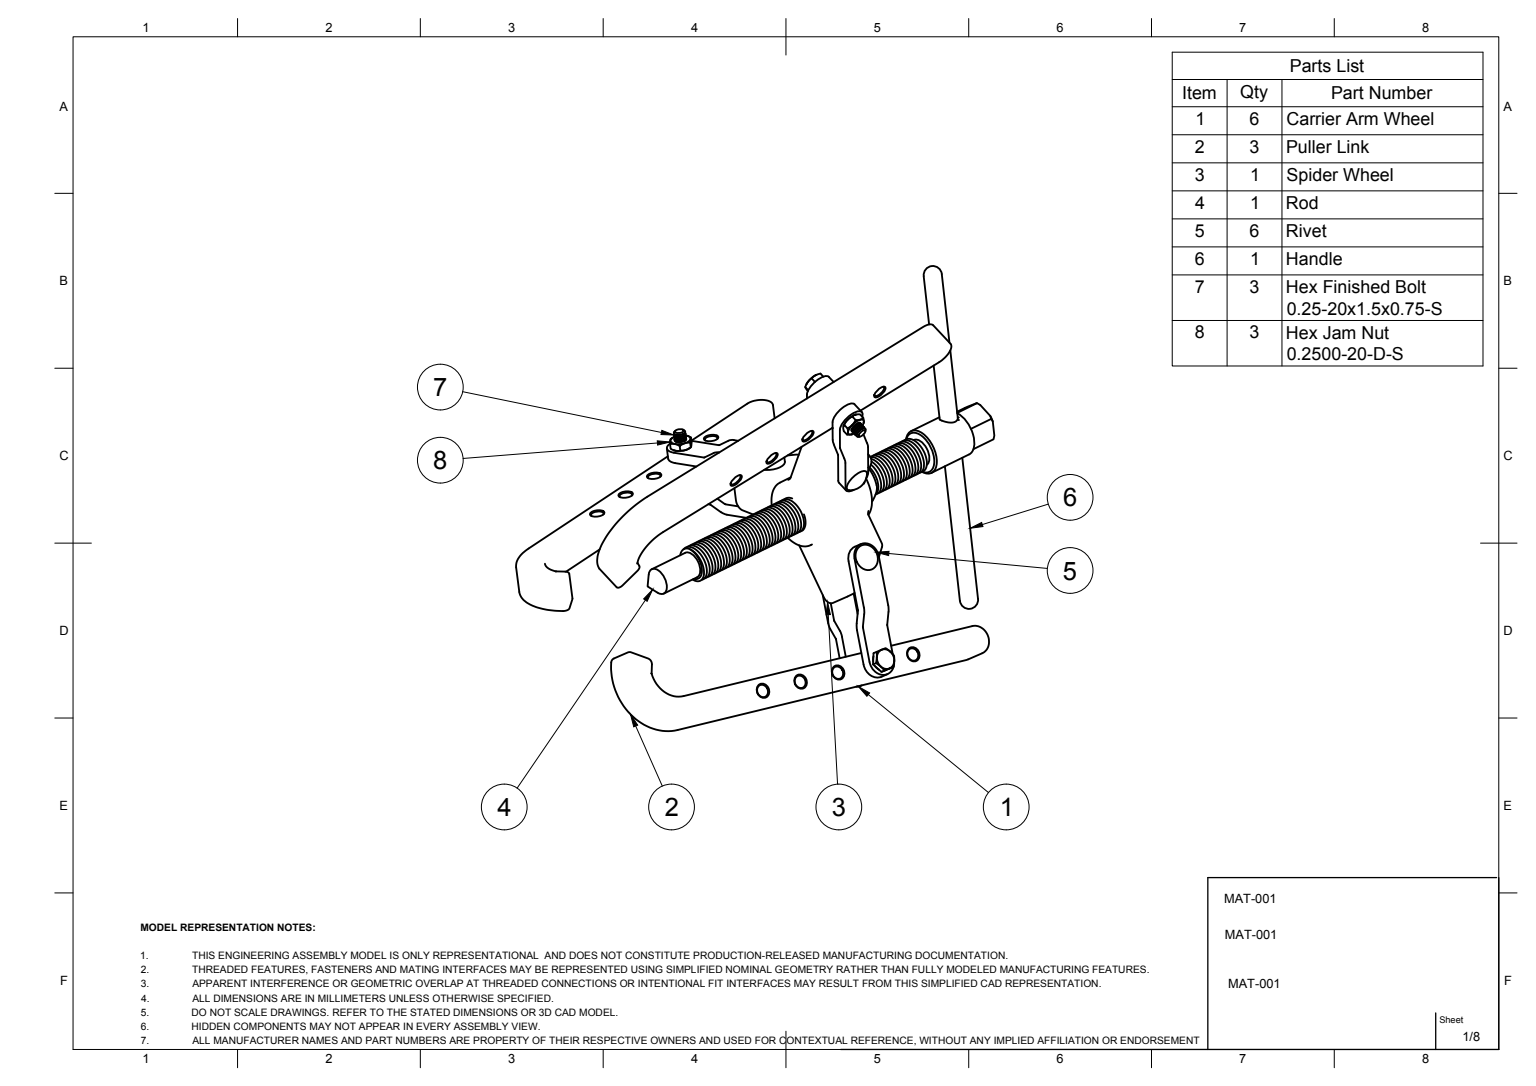
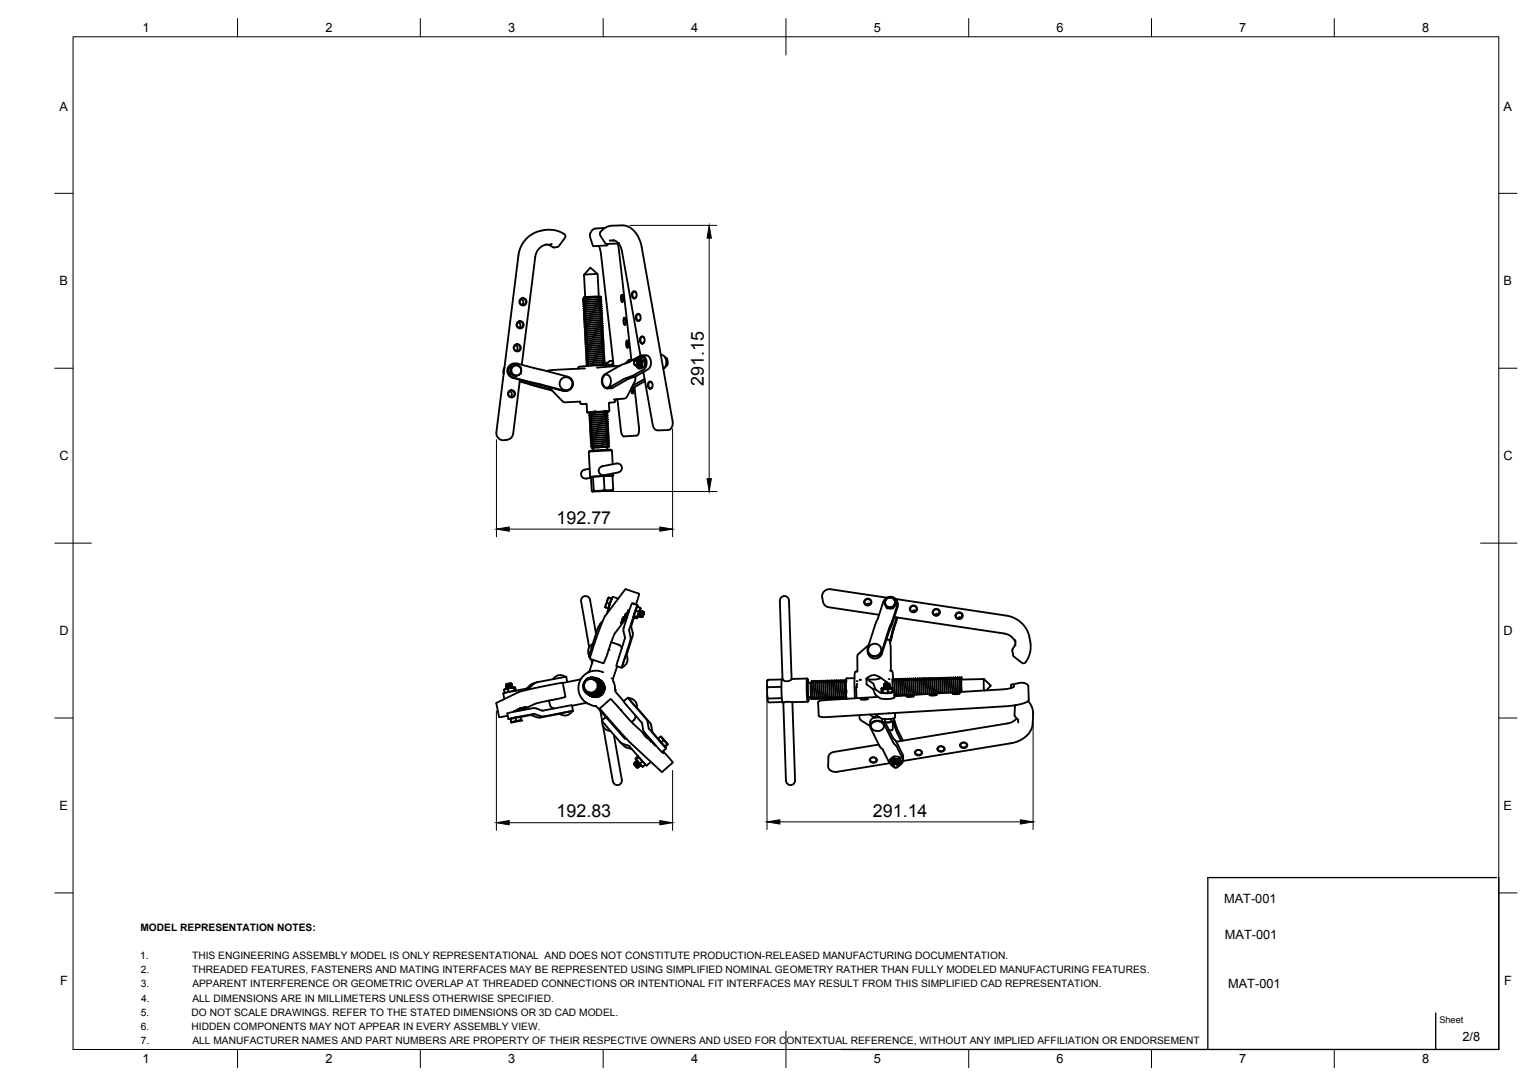
ISO-10303-21;
HEADER;
/* Generated by software containing ST-Developer
 * from STEP Tools, Inc. (www.steptools.com) 
 */

FILE_DESCRIPTION(
/* description */ ('STEP AP214'),
/* implementation_level */ '2;1');

FILE_NAME(
/* name */ 'MAT-001.step',
/* time_stamp */ '2026-11-14T04:30:00-08:00',
/* author */ (''),
/* organization */ (''),
/* preprocessor_version */ 'ST-DEVELOPER v20.2',
/* originating_system */ 'Autodesk Translation Framework v15.17.0.0',
/* authorisation */ '');

FILE_SCHEMA (('AUTOMOTIVE_DESIGN { 1 0 10303 214 3 1 1 }'));
ENDSEC;

DATA;
#10=MECHANICAL_DESIGN_GEOMETRIC_PRESENTATION_REPRESENTATION('',(#123,#124,
#125,#126,#127,#128,#129,#130),#40809);
#11=ITEM_DEFINED_TRANSFORMATION($,$,#7014,#7161);
#12=ITEM_DEFINED_TRANSFORMATION($,$,#7055,#7162);
#13=ITEM_DEFINED_TRANSFORMATION($,$,#6396,#7163);
#14=ITEM_DEFINED_TRANSFORMATION($,$,#6698,#7164);
#15=ITEM_DEFINED_TRANSFORMATION($,$,#6828,#7165);
#16=ITEM_DEFINED_TRANSFORMATION($,$,#6744,#7166);
#17=ITEM_DEFINED_TRANSFORMATION($,$,#6836,#7167);
#18=ITEM_DEFINED_TRANSFORMATION($,$,#6754,#7168);
#19=ITEM_DEFINED_TRANSFORMATION($,$,#7014,#7169);
#20=ITEM_DEFINED_TRANSFORMATION($,$,#6828,#7170);
#21=ITEM_DEFINED_TRANSFORMATION($,$,#7014,#7171);
#22=ITEM_DEFINED_TRANSFORMATION($,$,#7014,#7172);
#23=ITEM_DEFINED_TRANSFORMATION($,$,#6828,#7173);
#24=ITEM_DEFINED_TRANSFORMATION($,$,#6828,#7174);
#25=ITEM_DEFINED_TRANSFORMATION($,$,#6754,#7175);
#26=ITEM_DEFINED_TRANSFORMATION($,$,#6754,#7176);
#27=ITEM_DEFINED_TRANSFORMATION($,$,#6828,#7177);
#28=ITEM_DEFINED_TRANSFORMATION($,$,#6828,#7178);
#29=ITEM_DEFINED_TRANSFORMATION($,$,#6836,#7179);
#30=ITEM_DEFINED_TRANSFORMATION($,$,#6836,#7180);
#31=ITEM_DEFINED_TRANSFORMATION($,$,#7014,#7181);
#32=ITEM_DEFINED_TRANSFORMATION($,$,#7014,#7182);
#33=ITEM_DEFINED_TRANSFORMATION($,$,#7055,#7183);
#34=ITEM_DEFINED_TRANSFORMATION($,$,#7055,#7184);
#35=(
REPRESENTATION_RELATIONSHIP($,$,#40863,#40856)
REPRESENTATION_RELATIONSHIP_WITH_TRANSFORMATION(#11)
SHAPE_REPRESENTATION_RELATIONSHIP()
);
#36=(
REPRESENTATION_RELATIONSHIP($,$,#40864,#40856)
REPRESENTATION_RELATIONSHIP_WITH_TRANSFORMATION(#12)
SHAPE_REPRESENTATION_RELATIONSHIP()
);
#37=(
REPRESENTATION_RELATIONSHIP($,$,#40857,#40856)
REPRESENTATION_RELATIONSHIP_WITH_TRANSFORMATION(#13)
SHAPE_REPRESENTATION_RELATIONSHIP()
);
#38=(
REPRESENTATION_RELATIONSHIP($,$,#40858,#40856)
REPRESENTATION_RELATIONSHIP_WITH_TRANSFORMATION(#14)
SHAPE_REPRESENTATION_RELATIONSHIP()
);
#39=(
REPRESENTATION_RELATIONSHIP($,$,#40861,#40856)
REPRESENTATION_RELATIONSHIP_WITH_TRANSFORMATION(#15)
SHAPE_REPRESENTATION_RELATIONSHIP()
);
#40=(
REPRESENTATION_RELATIONSHIP($,$,#40859,#40856)
REPRESENTATION_RELATIONSHIP_WITH_TRANSFORMATION(#16)
SHAPE_REPRESENTATION_RELATIONSHIP()
);
#41=(
REPRESENTATION_RELATIONSHIP($,$,#40862,#40856)
REPRESENTATION_RELATIONSHIP_WITH_TRANSFORMATION(#17)
SHAPE_REPRESENTATION_RELATIONSHIP()
);
#42=(
REPRESENTATION_RELATIONSHIP($,$,#40860,#40856)
REPRESENTATION_RELATIONSHIP_WITH_TRANSFORMATION(#18)
SHAPE_REPRESENTATION_RELATIONSHIP()
);
#43=(
REPRESENTATION_RELATIONSHIP($,$,#40863,#40856)
REPRESENTATION_RELATIONSHIP_WITH_TRANSFORMATION(#19)
SHAPE_REPRESENTATION_RELATIONSHIP()
);
#44=(
REPRESENTATION_RELATIONSHIP($,$,#40861,#40856)
REPRESENTATION_RELATIONSHIP_WITH_TRANSFORMATION(#20)
SHAPE_REPRESENTATION_RELATIONSHIP()
);
#45=(
REPRESENTATION_RELATIONSHIP($,$,#40863,#40856)
REPRESENTATION_RELATIONSHIP_WITH_TRANSFORMATION(#21)
SHAPE_REPRESENTATION_RELATIONSHIP()
);
#46=(
REPRESENTATION_RELATIONSHIP($,$,#40863,#40856)
REPRESENTATION_RELATIONSHIP_WITH_TRANSFORMATION(#22)
SHAPE_REPRESENTATION_RELATIONSHIP()
);
#47=(
REPRESENTATION_RELATIONSHIP($,$,#40861,#40856)
REPRESENTATION_RELATIONSHIP_WITH_TRANSFORMATION(#23)
SHAPE_REPRESENTATION_RELATIONSHIP()
);
#48=(
REPRESENTATION_RELATIONSHIP($,$,#40861,#40856)
REPRESENTATION_RELATIONSHIP_WITH_TRANSFORMATION(#24)
SHAPE_REPRESENTATION_RELATIONSHIP()
);
#49=(
REPRESENTATION_RELATIONSHIP($,$,#40860,#40856)
REPRESENTATION_RELATIONSHIP_WITH_TRANSFORMATION(#25)
SHAPE_REPRESENTATION_RELATIONSHIP()
);
#50=(
REPRESENTATION_RELATIONSHIP($,$,#40860,#40856)
REPRESENTATION_RELATIONSHIP_WITH_TRANSFORMATION(#26)
SHAPE_REPRESENTATION_RELATIONSHIP()
);
#51=(
REPRESENTATION_RELATIONSHIP($,$,#40861,#40856)
REPRESENTATION_RELATIONSHIP_WITH_TRANSFORMATION(#27)
SHAPE_REPRESENTATION_RELATIONSHIP()
);
#52=(
REPRESENTATION_RELATIONSHIP($,$,#40861,#40856)
REPRESENTATION_RELATIONSHIP_WITH_TRANSFORMATION(#28)
SHAPE_REPRESENTATION_RELATIONSHIP()
);
#53=(
REPRESENTATION_RELATIONSHIP($,$,#40862,#40856)
REPRESENTATION_RELATIONSHIP_WITH_TRANSFORMATION(#29)
SHAPE_REPRESENTATION_RELATIONSHIP()
);
#54=(
REPRESENTATION_RELATIONSHIP($,$,#40862,#40856)
REPRESENTATION_RELATIONSHIP_WITH_TRANSFORMATION(#30)
SHAPE_REPRESENTATION_RELATIONSHIP()
);
#55=(
REPRESENTATION_RELATIONSHIP($,$,#40863,#40856)
REPRESENTATION_RELATIONSHIP_WITH_TRANSFORMATION(#31)
SHAPE_REPRESENTATION_RELATIONSHIP()
);
#56=(
REPRESENTATION_RELATIONSHIP($,$,#40863,#40856)
REPRESENTATION_RELATIONSHIP_WITH_TRANSFORMATION(#32)
SHAPE_REPRESENTATION_RELATIONSHIP()
);
#57=(
REPRESENTATION_RELATIONSHIP($,$,#40864,#40856)
REPRESENTATION_RELATIONSHIP_WITH_TRANSFORMATION(#33)
SHAPE_REPRESENTATION_RELATIONSHIP()
);
#58=(
REPRESENTATION_RELATIONSHIP($,$,#40864,#40856)
REPRESENTATION_RELATIONSHIP_WITH_TRANSFORMATION(#34)
SHAPE_REPRESENTATION_RELATIONSHIP()
);
#59=CONTEXT_DEPENDENT_SHAPE_REPRESENTATION(#35,#40832);
#60=CONTEXT_DEPENDENT_SHAPE_REPRESENTATION(#36,#40833);
#61=CONTEXT_DEPENDENT_SHAPE_REPRESENTATION(#37,#40834);
#62=CONTEXT_DEPENDENT_SHAPE_REPRESENTATION(#38,#40835);
#63=CONTEXT_DEPENDENT_SHAPE_REPRESENTATION(#39,#40836);
#64=CONTEXT_DEPENDENT_SHAPE_REPRESENTATION(#40,#40837);
#65=CONTEXT_DEPENDENT_SHAPE_REPRESENTATION(#41,#40838);
#66=CONTEXT_DEPENDENT_SHAPE_REPRESENTATION(#42,#40839);
#67=CONTEXT_DEPENDENT_SHAPE_REPRESENTATION(#43,#40840);
#68=CONTEXT_DEPENDENT_SHAPE_REPRESENTATION(#44,#40841);
#69=CONTEXT_DEPENDENT_SHAPE_REPRESENTATION(#45,#40842);
#70=CONTEXT_DEPENDENT_SHAPE_REPRESENTATION(#46,#40843);
#71=CONTEXT_DEPENDENT_SHAPE_REPRESENTATION(#47,#40844);
#72=CONTEXT_DEPENDENT_SHAPE_REPRESENTATION(#48,#40845);
#73=CONTEXT_DEPENDENT_SHAPE_REPRESENTATION(#49,#40846);
#74=CONTEXT_DEPENDENT_SHAPE_REPRESENTATION(#50,#40847);
#75=CONTEXT_DEPENDENT_SHAPE_REPRESENTATION(#51,#40848);
#76=CONTEXT_DEPENDENT_SHAPE_REPRESENTATION(#52,#40849);
#77=CONTEXT_DEPENDENT_SHAPE_REPRESENTATION(#53,#40850);
#78=CONTEXT_DEPENDENT_SHAPE_REPRESENTATION(#54,#40851);
#79=CONTEXT_DEPENDENT_SHAPE_REPRESENTATION(#55,#40852);
#80=CONTEXT_DEPENDENT_SHAPE_REPRESENTATION(#56,#40853);
#81=CONTEXT_DEPENDENT_SHAPE_REPRESENTATION(#57,#40854);
#82=CONTEXT_DEPENDENT_SHAPE_REPRESENTATION(#58,#40855);
#83=NEXT_ASSEMBLY_USAGE_OCCURRENCE('Carrier Arm Wheel:1',
'Carrier Arm Wheel:1','Carrier Arm Wheel:1',#40866,#40873,
'Carrier Arm Wheel:1');
#84=NEXT_ASSEMBLY_USAGE_OCCURRENCE('Puller Link:1','Puller Link:1',
'Puller Link:1',#40866,#40874,'Puller Link:1');
#85=NEXT_ASSEMBLY_USAGE_OCCURRENCE('Spider Wheel:1','Spider Wheel:1',
'Spider Wheel:1',#40866,#40867,'Spider Wheel:1');
#86=NEXT_ASSEMBLY_USAGE_OCCURRENCE('Rod:1','Rod:1','Rod:1',#40866,#40868,
'Rod:1');
#87=NEXT_ASSEMBLY_USAGE_OCCURRENCE('Rivet:1','Rivet:1','Rivet:1',#40866,
#40871,'Rivet:1');
#88=NEXT_ASSEMBLY_USAGE_OCCURRENCE('Handle:1','Handle:1','Handle:1',#40866,
#40869,'Handle:1');
#89=NEXT_ASSEMBLY_USAGE_OCCURRENCE(
'Hex Finished Bolt 0.25-20x1.5x0.75-S:1',
'Hex Finished Bolt 0.25-20x1.5x0.75-S:1',
'Hex Finished Bolt 0.25-20x1.5x0.75-S:1',#40866,#40872,
'Hex Finished Bolt 0.25-20x1.5x0.75-S:1');
#90=NEXT_ASSEMBLY_USAGE_OCCURRENCE('Hex Jam Nut 0.2500-20-D-S:1',
'Hex Jam Nut 0.2500-20-D-S:1','Hex Jam Nut 0.2500-20-D-S:1',#40866,#40870,
'Hex Jam Nut 0.2500-20-D-S:1');
#91=NEXT_ASSEMBLY_USAGE_OCCURRENCE('Carrier Arm Wheel:2',
'Carrier Arm Wheel:2','Carrier Arm Wheel:2',#40866,#40873,
'Carrier Arm Wheel:2');
#92=NEXT_ASSEMBLY_USAGE_OCCURRENCE('Rivet:2','Rivet:2','Rivet:2',#40866,
#40871,'Rivet:2');
#93=NEXT_ASSEMBLY_USAGE_OCCURRENCE('Carrier Arm Wheel:3',
'Carrier Arm Wheel:3','Carrier Arm Wheel:3',#40866,#40873,
'Carrier Arm Wheel:3');
#94=NEXT_ASSEMBLY_USAGE_OCCURRENCE('Carrier Arm Wheel:4',
'Carrier Arm Wheel:4','Carrier Arm Wheel:4',#40866,#40873,
'Carrier Arm Wheel:4');
#95=NEXT_ASSEMBLY_USAGE_OCCURRENCE('Rivet:3','Rivet:3','Rivet:3',#40866,
#40871,'Rivet:3');
#96=NEXT_ASSEMBLY_USAGE_OCCURRENCE('Rivet:4','Rivet:4','Rivet:4',#40866,
#40871,'Rivet:4');
#97=NEXT_ASSEMBLY_USAGE_OCCURRENCE('Hex Jam Nut 0.2500-20-D-S:2',
'Hex Jam Nut 0.2500-20-D-S:2','Hex Jam Nut 0.2500-20-D-S:2',#40866,#40870,
'Hex Jam Nut 0.2500-20-D-S:2');
#98=NEXT_ASSEMBLY_USAGE_OCCURRENCE('Hex Jam Nut 0.2500-20-D-S:3',
'Hex Jam Nut 0.2500-20-D-S:3','Hex Jam Nut 0.2500-20-D-S:3',#40866,#40870,
'Hex Jam Nut 0.2500-20-D-S:3');
#99=NEXT_ASSEMBLY_USAGE_OCCURRENCE('Rivet:5','Rivet:5','Rivet:5',#40866,
#40871,'Rivet:5');
#100=NEXT_ASSEMBLY_USAGE_OCCURRENCE('Rivet:6','Rivet:6','Rivet:6',#40866,
#40871,'Rivet:6');
#101=NEXT_ASSEMBLY_USAGE_OCCURRENCE(
'Hex Finished Bolt 0.25-20x1.5x0.75-S:2',
'Hex Finished Bolt 0.25-20x1.5x0.75-S:2',
'Hex Finished Bolt 0.25-20x1.5x0.75-S:2',#40866,#40872,
'Hex Finished Bolt 0.25-20x1.5x0.75-S:2');
#102=NEXT_ASSEMBLY_USAGE_OCCURRENCE(
'Hex Finished Bolt 0.25-20x1.5x0.75-S:3',
'Hex Finished Bolt 0.25-20x1.5x0.75-S:3',
'Hex Finished Bolt 0.25-20x1.5x0.75-S:3',#40866,#40872,
'Hex Finished Bolt 0.25-20x1.5x0.75-S:3');
#103=NEXT_ASSEMBLY_USAGE_OCCURRENCE('Carrier Arm Wheel:5',
'Carrier Arm Wheel:5','Carrier Arm Wheel:5',#40866,#40873,
'Carrier Arm Wheel:5');
#104=NEXT_ASSEMBLY_USAGE_OCCURRENCE('Carrier Arm Wheel:6',
'Carrier Arm Wheel:6','Carrier Arm Wheel:6',#40866,#40873,
'Carrier Arm Wheel:6');
#105=NEXT_ASSEMBLY_USAGE_OCCURRENCE('Puller Link:2','Puller Link:2',
'Puller Link:2',#40866,#40874,'Puller Link:2');
#106=NEXT_ASSEMBLY_USAGE_OCCURRENCE('Puller Link:3','Puller Link:3',
'Puller Link:3',#40866,#40874,'Puller Link:3');
#107=SHAPE_REPRESENTATION_RELATIONSHIP('SRR','None',#40857,#115);
#108=SHAPE_REPRESENTATION_RELATIONSHIP('SRR','None',#40858,#116);
#109=SHAPE_REPRESENTATION_RELATIONSHIP('SRR','None',#40859,#117);
#110=SHAPE_REPRESENTATION_RELATIONSHIP('SRR','None',#40860,#118);
#111=SHAPE_REPRESENTATION_RELATIONSHIP('SRR','None',#40861,#119);
#112=SHAPE_REPRESENTATION_RELATIONSHIP('SRR','None',#40862,#120);
#113=SHAPE_REPRESENTATION_RELATIONSHIP('SRR','None',#40863,#121);
#114=SHAPE_REPRESENTATION_RELATIONSHIP('SRR','None',#40864,#122);
#115=ADVANCED_BREP_SHAPE_REPRESENTATION('',(#131),#40801);
#116=ADVANCED_BREP_SHAPE_REPRESENTATION('',(#132),#40802);
#117=ADVANCED_BREP_SHAPE_REPRESENTATION('',(#133),#40803);
#118=ADVANCED_BREP_SHAPE_REPRESENTATION('',(#134),#40804);
#119=ADVANCED_BREP_SHAPE_REPRESENTATION('',(#135),#40805);
#120=ADVANCED_BREP_SHAPE_REPRESENTATION('',(#136),#40806);
#121=ADVANCED_BREP_SHAPE_REPRESENTATION('',(#137),#40807);
#122=ADVANCED_BREP_SHAPE_REPRESENTATION('',(#138),#40808);
#123=STYLED_ITEM('',(#40906),#131);
#124=STYLED_ITEM('',(#40907),#132);
#125=STYLED_ITEM('',(#40908),#133);
#126=STYLED_ITEM('',(#40909),#134);
#127=STYLED_ITEM('',(#40908),#135);
#128=STYLED_ITEM('',(#40909),#136);
#129=STYLED_ITEM('',(#40906),#137);
#130=STYLED_ITEM('',(#40906),#138);
#131=MANIFOLD_SOLID_BREP('Body1',#6298);
#132=MANIFOLD_SOLID_BREP('Body1',#6299);
#133=MANIFOLD_SOLID_BREP('Body1',#6300);
#134=MANIFOLD_SOLID_BREP('Body1',#6301);
#135=MANIFOLD_SOLID_BREP('Body1',#6302);
#136=MANIFOLD_SOLID_BREP('Body1',#6303);
#137=MANIFOLD_SOLID_BREP('Body1',#6304);
#138=MANIFOLD_SOLID_BREP('Body1',#6305);
#139=SPHERICAL_SURFACE('',#6615,5.);
#140=SPHERICAL_SURFACE('',#6624,5.);
#141=SPHERICAL_SURFACE('',#6633,5.);
#142=SPHERICAL_SURFACE('',#6642,5.);
#143=SPHERICAL_SURFACE('',#6643,5.);
#144=SPHERICAL_SURFACE('',#6652,5.);
#145=SPHERICAL_SURFACE('',#6745,4.975);
#146=SPHERICAL_SURFACE('',#6749,4.975);
#147=SPHERICAL_SURFACE('',#6832,9.31007692307692);
#148=(
BOUNDED_SURFACE()
B_SPLINE_SURFACE(1,2,((#13053,#13054,#13055,#13056,#13057,#13058,#13059,
#13060,#13061,#13062,#13063,#13064,#13065,#13066,#13067,#13068,#13069,#13070,
#13071,#13072,#13073,#13074,#13075,#13076,#13077,#13078,#13079,#13080,#13081,
#13082,#13083,#13084,#13085,#13086,#13087,#13088,#13089,#13090,#13091,#13092,
#13093,#13094,#13095,#13096,#13097,#13098,#13099,#13100,#13101,#13102,#13103,
#13104,#13105,#13106,#13107,#13108,#13109,#13110,#13111,#13112,#13113,#13114,
#13115,#13116,#13117,#13118,#13119,#13120,#13121,#13122,#13123,#13124,#13125,
#13126,#13127,#13128,#13129,#13130,#13131,#13132,#13133,#13134,#13135,#13136,
#13137,#13138,#13139,#13140,#13141,#13142,#13143,#13144,#13145,#13146,#13147,
#13148,#13149,#13150,#13151,#13152,#13153,#13154,#13155,#13156,#13157,#13158,
#13159,#13160,#13161,#13162,#13163,#13164,#13165,#13166,#13167,#13168,#13169,
#13170,#13171,#13172,#13173,#13174,#13175,#13176,#13177,#13178,#13179,#13180,
#13181,#13182,#13183,#13184,#13185,#13186,#13187,#13188,#13189,#13190,#13191,
#13192,#13193,#13194,#13195,#13196,#13197,#13198,#13199,#13200,#13201,#13202,
#13203,#13204,#13205,#13206,#13207,#13208,#13209,#13210,#13211,#13212,#13213,
#13214,#13215,#13216,#13217,#13218,#13219,#13220,#13221,#13222,#13223,#13224,
#13225,#13226,#13227,#13228,#13229,#13230,#13231,#13232,#13233,#13234,#13235,
#13236,#13237,#13238,#13239,#13240,#13241,#13242,#13243,#13244,#13245,#13246,
#13247,#13248,#13249,#13250,#13251,#13252,#13253,#13254,#13255,#13256,#13257,
#13258,#13259,#13260,#13261,#13262,#13263,#13264,#13265,#13266,#13267,#13268,
#13269,#13270,#13271,#13272,#13273,#13274,#13275,#13276,#13277,#13278,#13279,
#13280,#13281,#13282,#13283,#13284,#13285,#13286,#13287,#13288,#13289,#13290,
#13291,#13292,#13293,#13294,#13295,#13296,#13297,#13298,#13299,#13300,#13301,
#13302,#13303,#13304,#13305,#13306,#13307,#13308,#13309,#13310,#13311,#13312,
#13313,#13314,#13315,#13316,#13317,#13318,#13319,#13320,#13321,#13322,#13323,
#13324,#13325,#13326,#13327,#13328,#13329,#13330,#13331,#13332,#13333,#13334,
#13335,#13336,#13337,#13338,#13339,#13340,#13341,#13342,#13343,#13344,#13345,
#13346,#13347,#13348,#13349,#13350,#13351,#13352,#13353,#13354,#13355,#13356,
#13357,#13358,#13359,#13360,#13361,#13362,#13363,#13364,#13365,#13366,#13367,
#13368,#13369,#13370,#13371,#13372,#13373,#13374,#13375,#13376,#13377,#13378,
#13379,#13380,#13381,#13382,#13383,#13384,#13385,#13386,#13387,#13388,#13389,
#13390,#13391,#13392,#13393,#13394,#13395,#13396,#13397,#13398,#13399,#13400,
#13401,#13402,#13403,#13404,#13405,#13406,#13407,#13408,#13409,#13410,#13411,
#13412,#13413,#13414,#13415,#13416,#13417,#13418,#13419,#13420,#13421,#13422,
#13423,#13424,#13425,#13426,#13427,#13428,#13429,#13430,#13431,#13432,#13433,
#13434,#13435,#13436,#13437,#13438,#13439,#13440,#13441,#13442,#13443,#13444,
#13445,#13446,#13447,#13448,#13449,#13450,#13451,#13452,#13453,#13454,#13455,
#13456,#13457,#13458,#13459,#13460,#13461,#13462,#13463,#13464,#13465,#13466,
#13467,#13468,#13469,#13470,#13471,#13472,#13473,#13474,#13475,#13476,#13477,
#13478,#13479,#13480,#13481,#13482,#13483,#13484,#13485,#13486,#13487,#13488,
#13489,#13490,#13491,#13492,#13493,#13494,#13495,#13496,#13497,#13498,#13499,
#13500,#13501,#13502,#13503,#13504,#13505,#13506,#13507,#13508,#13509,#13510,
#13511,#13512,#13513,#13514,#13515,#13516,#13517,#13518,#13519,#13520,#13521,
#13522,#13523,#13524,#13525,#13526,#13527,#13528,#13529,#13530,#13531,#13532,
#13533,#13534,#13535,#13536,#13537,#13538,#13539,#13540,#13541,#13542,#13543,
#13544,#13545,#13546,#13547,#13548,#13549,#13550,#13551,#13552,#13553,#13554,
#13555,#13556,#13557,#13558,#13559,#13560,#13561,#13562,#13563,#13564,#13565,
#13566,#13567,#13568,#13569,#13570,#13571,#13572,#13573,#13574,#13575,#13576,
#13577,#13578,#13579,#13580,#13581,#13582,#13583,#13584,#13585,#13586,#13587,
#13588,#13589,#13590,#13591,#13592,#13593,#13594,#13595,#13596,#13597,#13598,
#13599,#13600,#13601,#13602,#13603,#13604,#13605,#13606,#13607,#13608,#13609,
#13610,#13611,#13612,#13613,#13614,#13615,#13616,#13617,#13618,#13619,#13620,
#13621,#13622,#13623,#13624,#13625,#13626,#13627,#13628,#13629,#13630,#13631,
#13632,#13633,#13634,#13635,#13636,#13637,#13638,#13639,#13640,#13641,#13642,
#13643,#13644,#13645,#13646,#13647,#13648,#13649,#13650,#13651,#13652,#13653,
#13654,#13655,#13656,#13657,#13658,#13659,#13660,#13661,#13662,#13663,#13664,
#13665,#13666,#13667,#13668,#13669,#13670,#13671,#13672,#13673,#13674,#13675,
#13676,#13677,#13678,#13679,#13680,#13681,#13682,#13683,#13684,#13685,#13686,
#13687,#13688,#13689,#13690,#13691,#13692,#13693,#13694,#13695,#13696,#13697,
#13698,#13699,#13700,#13701,#13702,#13703,#13704,#13705,#13706,#13707,#13708,
#13709,#13710,#13711,#13712,#13713,#13714,#13715,#13716,#13717,#13718,#13719,
#13720,#13721,#13722,#13723,#13724,#13725,#13726,#13727,#13728,#13729,#13730,
#13731,#13732,#13733,#13734,#13735,#13736,#13737,#13738,#13739,#13740,#13741,
#13742,#13743,#13744,#13745,#13746,#13747,#13748,#13749,#13750,#13751,#13752,
#13753,#13754,#13755,#13756,#13757,#13758,#13759,#13760,#13761,#13762,#13763,
#13764,#13765,#13766,#13767,#13768,#13769,#13770,#13771,#13772,#13773,#13774,
#13775,#13776,#13777,#13778,#13779,#13780,#13781,#13782,#13783,#13784,#13785,
#13786,#13787,#13788,#13789,#13790,#13791,#13792,#13793,#13794,#13795,#13796,
#13797,#13798,#13799,#13800,#13801,#13802,#13803,#13804,#13805,#13806,#13807,
#13808,#13809,#13810,#13811,#13812,#13813,#13814,#13815,#13816,#13817,#13818,
#13819,#13820,#13821,#13822,#13823,#13824,#13825,#13826,#13827,#13828,#13829,
#13830,#13831,#13832,#13833,#13834,#13835,#13836,#13837,#13838,#13839,#13840,
#13841,#13842,#13843,#13844,#13845,#13846,#13847,#13848,#13849,#13850,#13851,
#13852,#13853,#13854,#13855,#13856,#13857,#13858,#13859,#13860,#13861,#13862,
#13863,#13864,#13865,#13866,#13867,#13868,#13869,#13870,#13871,#13872,#13873,
#13874,#13875,#13876,#13877,#13878,#13879,#13880,#13881,#13882,#13883,#13884,
#13885,#13886,#13887,#13888,#13889,#13890,#13891,#13892,#13893,#13894,#13895,
#13896,#13897,#13898,#13899,#13900,#13901,#13902,#13903,#13904,#13905,#13906,
#13907,#13908,#13909,#13910,#13911,#13912,#13913,#13914,#13915,#13916,#13917,
#13918,#13919,#13920,#13921,#13922,#13923,#13924,#13925,#13926,#13927,#13928,
#13929,#13930,#13931,#13932,#13933,#13934,#13935,#13936,#13937,#13938,#13939,
#13940,#13941,#13942,#13943,#13944,#13945,#13946,#13947,#13948,#13949,#13950,
#13951,#13952,#13953,#13954,#13955,#13956,#13957,#13958,#13959,#13960,#13961,
#13962,#13963,#13964,#13965,#13966,#13967,#13968,#13969,#13970,#13971,#13972,
#13973,#13974,#13975,#13976,#13977,#13978,#13979,#13980,#13981,#13982,#13983,
#13984,#13985,#13986,#13987,#13988,#13989,#13990,#13991,#13992,#13993,#13994,
#13995,#13996,#13997,#13998,#13999,#14000,#14001,#14002,#14003,#14004,#14005,
#14006,#14007,#14008,#14009,#14010,#14011,#14012,#14013,#14014,#14015,#14016,
#14017,#14018,#14019,#14020,#14021,#14022,#14023,#14024,#14025),(#14026,
#14027,#14028,#14029,#14030,#14031,#14032,#14033,#14034,#14035,#14036,#14037,
#14038,#14039,#14040,#14041,#14042,#14043,#14044,#14045,#14046,#14047,#14048,
#14049,#14050,#14051,#14052,#14053,#14054,#14055,#14056,#14057,#14058,#14059,
#14060,#14061,#14062,#14063,#14064,#14065,#14066,#14067,#14068,#14069,#14070,
#14071,#14072,#14073,#14074,#14075,#14076,#14077,#14078,#14079,#14080,#14081,
#14082,#14083,#14084,#14085,#14086,#14087,#14088,#14089,#14090,#14091,#14092,
#14093,#14094,#14095,#14096,#14097,#14098,#14099,#14100,#14101,#14102,#14103,
#14104,#14105,#14106,#14107,#14108,#14109,#14110,#14111,#14112,#14113,#14114,
#14115,#14116,#14117,#14118,#14119,#14120,#14121,#14122,#14123,#14124,#14125,
#14126,#14127,#14128,#14129,#14130,#14131,#14132,#14133,#14134,#14135,#14136,
#14137,#14138,#14139,#14140,#14141,#14142,#14143,#14144,#14145,#14146,#14147,
#14148,#14149,#14150,#14151,#14152,#14153,#14154,#14155,#14156,#14157,#14158,
#14159,#14160,#14161,#14162,#14163,#14164,#14165,#14166,#14167,#14168,#14169,
#14170,#14171,#14172,#14173,#14174,#14175,#14176,#14177,#14178,#14179,#14180,
#14181,#14182,#14183,#14184,#14185,#14186,#14187,#14188,#14189,#14190,#14191,
#14192,#14193,#14194,#14195,#14196,#14197,#14198,#14199,#14200,#14201,#14202,
#14203,#14204,#14205,#14206,#14207,#14208,#14209,#14210,#14211,#14212,#14213,
#14214,#14215,#14216,#14217,#14218,#14219,#14220,#14221,#14222,#14223,#14224,
#14225,#14226,#14227,#14228,#14229,#14230,#14231,#14232,#14233,#14234,#14235,
#14236,#14237,#14238,#14239,#14240,#14241,#14242,#14243,#14244,#14245,#14246,
#14247,#14248,#14249,#14250,#14251,#14252,#14253,#14254,#14255,#14256,#14257,
#14258,#14259,#14260,#14261,#14262,#14263,#14264,#14265,#14266,#14267,#14268,
#14269,#14270,#14271,#14272,#14273,#14274,#14275,#14276,#14277,#14278,#14279,
#14280,#14281,#14282,#14283,#14284,#14285,#14286,#14287,#14288,#14289,#14290,
#14291,#14292,#14293,#14294,#14295,#14296,#14297,#14298,#14299,#14300,#14301,
#14302,#14303,#14304,#14305,#14306,#14307,#14308,#14309,#14310,#14311,#14312,
#14313,#14314,#14315,#14316,#14317,#14318,#14319,#14320,#14321,#14322,#14323,
#14324,#14325,#14326,#14327,#14328,#14329,#14330,#14331,#14332,#14333,#14334,
#14335,#14336,#14337,#14338,#14339,#14340,#14341,#14342,#14343,#14344,#14345,
#14346,#14347,#14348,#14349,#14350,#14351,#14352,#14353,#14354,#14355,#14356,
#14357,#14358,#14359,#14360,#14361,#14362,#14363,#14364,#14365,#14366,#14367,
#14368,#14369,#14370,#14371,#14372,#14373,#14374,#14375,#14376,#14377,#14378,
#14379,#14380,#14381,#14382,#14383,#14384,#14385,#14386,#14387,#14388,#14389,
#14390,#14391,#14392,#14393,#14394,#14395,#14396,#14397,#14398,#14399,#14400,
#14401,#14402,#14403,#14404,#14405,#14406,#14407,#14408,#14409,#14410,#14411,
#14412,#14413,#14414,#14415,#14416,#14417,#14418,#14419,#14420,#14421,#14422,
#14423,#14424,#14425,#14426,#14427,#14428,#14429,#14430,#14431,#14432,#14433,
#14434,#14435,#14436,#14437,#14438,#14439,#14440,#14441,#14442,#14443,#14444,
#14445,#14446,#14447,#14448,#14449,#14450,#14451,#14452,#14453,#14454,#14455,
#14456,#14457,#14458,#14459,#14460,#14461,#14462,#14463,#14464,#14465,#14466,
#14467,#14468,#14469,#14470,#14471,#14472,#14473,#14474,#14475,#14476,#14477,
#14478,#14479,#14480,#14481,#14482,#14483,#14484,#14485,#14486,#14487,#14488,
#14489,#14490,#14491,#14492,#14493,#14494,#14495,#14496,#14497,#14498,#14499,
#14500,#14501,#14502,#14503,#14504,#14505,#14506,#14507,#14508,#14509,#14510,
#14511,#14512,#14513,#14514,#14515,#14516,#14517,#14518,#14519,#14520,#14521,
#14522,#14523,#14524,#14525,#14526,#14527,#14528,#14529,#14530,#14531,#14532,
#14533,#14534,#14535,#14536,#14537,#14538,#14539,#14540,#14541,#14542,#14543,
#14544,#14545,#14546,#14547,#14548,#14549,#14550,#14551,#14552,#14553,#14554,
#14555,#14556,#14557,#14558,#14559,#14560,#14561,#14562,#14563,#14564,#14565,
#14566,#14567,#14568,#14569,#14570,#14571,#14572,#14573,#14574,#14575,#14576,
#14577,#14578,#14579,#14580,#14581,#14582,#14583,#14584,#14585,#14586,#14587,
#14588,#14589,#14590,#14591,#14592,#14593,#14594,#14595,#14596,#14597,#14598,
#14599,#14600,#14601,#14602,#14603,#14604,#14605,#14606,#14607,#14608,#14609,
#14610,#14611,#14612,#14613,#14614,#14615,#14616,#14617,#14618,#14619,#14620,
#14621,#14622,#14623,#14624,#14625,#14626,#14627,#14628,#14629,#14630,#14631,
#14632,#14633,#14634,#14635,#14636,#14637,#14638,#14639,#14640,#14641,#14642,
#14643,#14644,#14645,#14646,#14647,#14648,#14649,#14650,#14651,#14652,#14653,
#14654,#14655,#14656,#14657,#14658,#14659,#14660,#14661,#14662,#14663,#14664,
#14665,#14666,#14667,#14668,#14669,#14670,#14671,#14672,#14673,#14674,#14675,
#14676,#14677,#14678,#14679,#14680,#14681,#14682,#14683,#14684,#14685,#14686,
#14687,#14688,#14689,#14690,#14691,#14692,#14693,#14694,#14695,#14696,#14697,
#14698,#14699,#14700,#14701,#14702,#14703,#14704,#14705,#14706,#14707,#14708,
#14709,#14710,#14711,#14712,#14713,#14714,#14715,#14716,#14717,#14718,#14719,
#14720,#14721,#14722,#14723,#14724,#14725,#14726,#14727,#14728,#14729,#14730,
#14731,#14732,#14733,#14734,#14735,#14736,#14737,#14738,#14739,#14740,#14741,
#14742,#14743,#14744,#14745,#14746,#14747,#14748,#14749,#14750,#14751,#14752,
#14753,#14754,#14755,#14756,#14757,#14758,#14759,#14760,#14761,#14762,#14763,
#14764,#14765,#14766,#14767,#14768,#14769,#14770,#14771,#14772,#14773,#14774,
#14775,#14776,#14777,#14778,#14779,#14780,#14781,#14782,#14783,#14784,#14785,
#14786,#14787,#14788,#14789,#14790,#14791,#14792,#14793,#14794,#14795,#14796,
#14797,#14798,#14799,#14800,#14801,#14802,#14803,#14804,#14805,#14806,#14807,
#14808,#14809,#14810,#14811,#14812,#14813,#14814,#14815,#14816,#14817,#14818,
#14819,#14820,#14821,#14822,#14823,#14824,#14825,#14826,#14827,#14828,#14829,
#14830,#14831,#14832,#14833,#14834,#14835,#14836,#14837,#14838,#14839,#14840,
#14841,#14842,#14843,#14844,#14845,#14846,#14847,#14848,#14849,#14850,#14851,
#14852,#14853,#14854,#14855,#14856,#14857,#14858,#14859,#14860,#14861,#14862,
#14863,#14864,#14865,#14866,#14867,#14868,#14869,#14870,#14871,#14872,#14873,
#14874,#14875,#14876,#14877,#14878,#14879,#14880,#14881,#14882,#14883,#14884,
#14885,#14886,#14887,#14888,#14889,#14890,#14891,#14892,#14893,#14894,#14895,
#14896,#14897,#14898,#14899,#14900,#14901,#14902,#14903,#14904,#14905,#14906,
#14907,#14908,#14909,#14910,#14911,#14912,#14913,#14914,#14915,#14916,#14917,
#14918,#14919,#14920,#14921,#14922,#14923,#14924,#14925,#14926,#14927,#14928,
#14929,#14930,#14931,#14932,#14933,#14934,#14935,#14936,#14937,#14938,#14939,
#14940,#14941,#14942,#14943,#14944,#14945,#14946,#14947,#14948,#14949,#14950,
#14951,#14952,#14953,#14954,#14955,#14956,#14957,#14958,#14959,#14960,#14961,
#14962,#14963,#14964,#14965,#14966,#14967,#14968,#14969,#14970,#14971,#14972,
#14973,#14974,#14975,#14976,#14977,#14978,#14979,#14980,#14981,#14982,#14983,
#14984,#14985,#14986,#14987,#14988,#14989,#14990,#14991,#14992,#14993,#14994,
#14995,#14996,#14997,#14998)),.UNSPECIFIED.,.F.,.F.,.F.)
B_SPLINE_SURFACE_WITH_KNOTS((2,2),(3,2,2,2,2,2,2,2,2,2,2,2,2,2,2,2,2,2,
2,2,2,2,2,2,2,2,2,2,2,2,2,2,2,2,2,2,2,2,2,2,2,2,2,2,2,2,2,2,2,2,2,2,2,2,
2,2,2,2,2,2,2,2,2,2,2,2,2,2,2,2,2,2,2,2,2,2,2,2,2,2,2,2,2,2,2,2,2,2,2,2,
2,2,2,2,2,2,2,2,2,2,2,2,2,2,2,2,2,2,2,2,2,2,2,2,2,2,2,2,2,2,2,2,2,2,2,2,
2,2,2,2,2,2,2,2,2,2,2,2,2,2,2,2,2,2,2,2,2,2,2,2,2,2,2,2,2,2,2,2,2,2,2,2,
2,2,2,2,2,2,2,2,2,2,2,2,2,2,2,2,2,2,2,2,2,2,2,2,2,2,2,2,2,2,2,2,2,2,2,2,
2,2,2,2,2,2,2,2,2,2,2,2,2,2,2,2,2,2,2,2,2,2,2,2,2,2,2,2,2,2,2,2,2,2,2,2,
2,2,2,2,2,2,2,2,2,2,2,2,2,2,2,2,2,2,2,2,2,2,2,2,2,2,2,2,2,2,2,2,2,2,2,2,
2,2,2,2,2,2,2,2,2,2,2,2,2,2,2,2,2,2,2,2,2,2,2,2,2,2,2,2,2,2,2,2,2,2,2,2,
2,2,2,2,2,2,2,2,2,2,2,2,2,2,2,2,2,2,2,2,2,2,2,2,2,2,2,2,2,2,2,2,2,2,2,2,
2,2,2,2,2,2,2,2,2,2,2,2,2,2,2,2,2,2,2,2,2,2,2,2,2,2,2,2,2,2,2,2,2,2,2,2,
2,2,2,2,2,2,2,2,2,2,2,2,2,2,2,2,2,2,2,2,2,2,2,2,2,2,2,2,2,2,2,2,2,2,2,2,
2,2,2,2,2,2,2,2,2,2,2,2,2,2,2,2,2,2,2,2,2,2,2,2,2,2,2,2,2,2,2,2,2,2,2,2,
2,2,2,2,2,2,2,2,2,2,2,2,2,2,2,2,2,2,2,2,2,2,2,2,2,2,2,2,2,2,2,2,2,2,2,2,
3),(0.,1.00000404874212),(0.,0.00205761316872428,0.00411522633744856,0.00617283950617284,
0.00823045267489712,0.0102880658436214,0.0123456790123457,0.01440329218107,
0.0164609053497942,0.0185185185185185,0.0205761316872428,0.0226337448559671,
0.0246913580246914,0.0267489711934156,0.0288065843621399,0.0308641975308642,
0.0329218106995885,0.0349794238683128,0.037037037037037,0.0390946502057613,
0.0411522633744856,0.0432098765432099,0.0452674897119342,0.0473251028806584,
0.0493827160493827,0.051440329218107,0.0534979423868313,0.0555555555555556,
0.0576131687242798,0.0596707818930041,0.0617283950617284,0.0637860082304527,
0.065843621399177,0.0679012345679012,0.0699588477366255,0.0720164609053498,
0.0740740740740741,0.0761316872427984,0.0781893004115226,0.0802469135802469,
0.0823045267489712,0.0843621399176955,0.0864197530864197,0.088477366255144,
0.0905349794238683,0.0925925925925926,0.0946502057613169,0.0967078189300412,
0.0987654320987654,0.10082304526749,0.102880658436214,0.104938271604938,
0.106995884773663,0.109053497942387,0.111111111111111,0.113168724279835,
0.11522633744856,0.117283950617284,0.119341563786008,0.121399176954733,
0.123456790123457,0.125514403292181,0.127572016460905,0.12962962962963,
0.131687242798354,0.133744855967078,0.135802469135802,0.137860082304527,
0.139917695473251,0.141975308641975,0.1440329218107,0.146090534979424,0.148148148148148,
0.150205761316872,0.152263374485597,0.154320987654321,0.156378600823045,
0.15843621399177,0.160493827160494,0.162551440329218,0.164609053497942,
0.166666666666667,0.168724279835391,0.170781893004115,0.172839506172839,
0.174897119341564,0.176954732510288,0.179012345679012,0.181069958847737,
0.183127572016461,0.185185185185185,0.187242798353909,0.189300411522634,
0.191358024691358,0.193415637860082,0.195473251028807,0.197530864197531,
0.199588477366255,0.201646090534979,0.203703703703704,0.205761316872428,
0.207818930041152,0.209876543209877,0.211934156378601,0.213991769547325,
0.216049382716049,0.218106995884774,0.220164609053498,0.222222222222222,
0.224279835390947,0.226337448559671,0.228395061728395,0.230452674897119,
0.232510288065844,0.234567901234568,0.236625514403292,0.238683127572016,
0.240740740740741,0.242798353909465,0.244855967078189,0.246913580246914,
0.248971193415638,0.251028806584362,0.253086419753086,0.255144032921811,
0.257201646090535,0.259259259259259,0.261316872427984,0.263374485596708,
0.265432098765432,0.267489711934156,0.269547325102881,0.271604938271605,
0.273662551440329,0.275720164609054,0.277777777777778,0.279835390946502,
0.281893004115226,0.283950617283951,0.286008230452675,0.288065843621399,
0.290123456790123,0.292181069958848,0.294238683127572,0.296296296296296,
0.298353909465021,0.300411522633745,0.302469135802469,0.304526748971193,
0.306584362139918,0.308641975308642,0.310699588477366,0.312757201646091,
0.314814814814815,0.316872427983539,0.318930041152263,0.320987654320988,
0.323045267489712,0.325102880658436,0.327160493827161,0.329218106995885,
0.331275720164609,0.333333333333333,0.335390946502058,0.337448559670782,
0.339506172839506,0.34156378600823,0.343621399176955,0.345679012345679,
0.347736625514403,0.349794238683128,0.351851851851852,0.353909465020576,
0.3559670781893,0.358024691358025,0.360082304526749,0.362139917695473,0.364197530864198,
0.366255144032922,0.368312757201646,0.37037037037037,0.372427983539095,
0.374485596707819,0.376543209876543,0.378600823045267,0.380658436213992,
0.382716049382716,0.38477366255144,0.386831275720165,0.388888888888889,
0.390946502057613,0.393004115226337,0.395061728395062,0.397119341563786,
0.39917695473251,0.401234567901235,0.403292181069959,0.405349794238683,
0.407407407407407,0.409465020576132,0.411522633744856,0.41358024691358,
0.415637860082305,0.417695473251029,0.419753086419753,0.421810699588477,
0.423868312757202,0.425925925925926,0.42798353909465,0.430041152263374,
0.432098765432099,0.434156378600823,0.436213991769547,0.438271604938272,
0.440329218106996,0.44238683127572,0.444444444444444,0.446502057613169,
0.448559670781893,0.450617283950617,0.452674897119342,0.454732510288066,
0.45679012345679,0.458847736625514,0.460905349794239,0.462962962962963,
0.465020576131687,0.467078189300412,0.469135802469136,0.47119341563786,
0.473251028806584,0.475308641975309,0.477366255144033,0.479423868312757,
0.481481481481481,0.483539094650206,0.48559670781893,0.487654320987654,
0.489711934156379,0.491769547325103,0.493827160493827,0.495884773662551,
0.497942386831276,0.5,0.502057613168724,0.504115226337449,0.506172839506173,
0.508230452674897,0.510288065843621,0.512345679012346,0.51440329218107,
0.516460905349794,0.518518518518518,0.520576131687243,0.522633744855967,
0.524691358024691,0.526748971193416,0.52880658436214,0.530864197530864,
0.532921810699588,0.534979423868313,0.537037037037037,0.539094650205761,
0.541152263374486,0.54320987654321,0.545267489711934,0.547325102880658,
0.549382716049383,0.551440329218107,0.553497942386831,0.555555555555556,
0.55761316872428,0.559670781893004,0.561728395061728,0.563786008230453,
0.565843621399177,0.567901234567901,0.569958847736626,0.57201646090535,
0.574074074074074,0.576131687242798,0.578189300411523,0.580246913580247,
0.582304526748971,0.584362139917695,0.58641975308642,0.588477366255144,
0.590534979423868,0.592592592592593,0.594650205761317,0.596707818930041,
0.598765432098765,0.60082304526749,0.602880658436214,0.604938271604938,
0.606995884773663,0.609053497942387,0.611111111111111,0.613168724279835,
0.61522633744856,0.617283950617284,0.619341563786008,0.621399176954732,
0.623456790123457,0.625514403292181,0.627572016460905,0.62962962962963,
0.631687242798354,0.633744855967078,0.635802469135803,0.637860082304527,
0.639917695473251,0.641975308641975,0.6440329218107,0.646090534979424,0.648148148148148,
0.650205761316872,0.652263374485597,0.654320987654321,0.656378600823045,
0.65843621399177,0.660493827160494,0.662551440329218,0.664609053497942,
0.666666666666667,0.668724279835391,0.670781893004115,0.672839506172839,
0.674897119341564,0.676954732510288,0.679012345679012,0.681069958847737,
0.683127572016461,0.685185185185185,0.687242798353909,0.689300411522634,
0.691358024691358,0.693415637860082,0.695473251028807,0.697530864197531,
0.699588477366255,0.701646090534979,0.703703703703704,0.705761316872428,
0.707818930041152,0.709876543209877,0.711934156378601,0.713991769547325,
0.716049382716049,0.718106995884774,0.720164609053498,0.722222222222222,
0.724279835390947,0.726337448559671,0.728395061728395,0.730452674897119,
0.732510288065844,0.734567901234568,0.736625514403292,0.738683127572016,
0.740740740740741,0.742798353909465,0.744855967078189,0.746913580246914,
0.748971193415638,0.751028806584362,0.753086419753086,0.755144032921811,
0.757201646090535,0.759259259259259,0.761316872427984,0.763374485596708,
0.765432098765432,0.767489711934156,0.769547325102881,0.771604938271605,
0.773662551440329,0.775720164609053,0.777777777777778,0.779835390946502,
0.781893004115226,0.783950617283951,0.786008230452675,0.788065843621399,
0.790123456790123,0.792181069958848,0.794238683127572,0.796296296296296,
0.798353909465021,0.800411522633745,0.802469135802469,0.804526748971193,
0.806584362139918,0.808641975308642,0.810699588477366,0.812757201646091,
0.814814814814815,0.816872427983539,0.818930041152263,0.820987654320988,
0.823045267489712,0.825102880658436,0.827160493827161,0.829218106995885,
0.831275720164609,0.833333333333333,0.835390946502058,0.837448559670782,
0.839506172839506,0.84156378600823,0.843621399176955,0.845679012345679,
0.847736625514403,0.849794238683128,0.851851851851852,0.853909465020576,
0.8559670781893,0.858024691358025,0.860082304526749,0.862139917695473,0.864197530864197,
0.866255144032922,0.868312757201646,0.87037037037037,0.872427983539095,
0.874485596707819,0.876543209876543,0.878600823045268,0.880658436213992,
0.882716049382716,0.88477366255144,0.886831275720165,0.888888888888889,
0.890946502057613,0.893004115226337,0.895061728395062,0.897119341563786,
0.89917695473251,0.901234567901235,0.903292181069959,0.905349794238683,
0.907407407407407,0.909465020576132,0.911522633744856,0.91358024691358,
0.915637860082305,0.917695473251029,0.919753086419753,0.921810699588477,
0.923868312757202,0.925925925925926,0.92798353909465,0.930041152263374,
0.932098765432099,0.934156378600823,0.936213991769547,0.938271604938272,
0.940329218106996,0.94238683127572,0.944444444444444,0.946502057613169,
0.948559670781893,0.950617283950617,0.952674897119342,0.954732510288066,
0.95679012345679,0.958847736625514,0.960905349794239,0.962962962962963,
0.965020576131687,0.967078189300412,0.969135802469136,0.97119341563786,
0.973251028806584,0.975308641975309,0.977366255144033,0.979423868312757,
0.981481481481482,0.983539094650206,0.98559670781893,0.987654320987654,
0.989711934156379,0.991769547325103,0.993827160493827,0.995884773662551,
0.997942386831276,1.),.UNSPECIFIED.)
GEOMETRIC_REPRESENTATION_ITEM()
RATIONAL_B_SPLINE_SURFACE(((1.,0.866025403784439,1.,0.866025403784439,1.,
0.866025403784439,1.,0.866025403784439,1.,0.866025403784439,1.,0.866025403784439,
1.,0.866025403784439,1.,0.866025403784439,1.,0.866025403784439,1.,0.866025403784439,
1.,0.866025403784439,1.,0.866025403784439,1.,0.866025403784439,1.,0.866025403784439,
1.,0.866025403784439,1.,0.866025403784439,1.,0.866025403784439,1.,0.866025403784439,
1.,0.866025403784439,1.,0.866025403784439,1.,0.866025403784439,1.,0.866025403784439,
1.,0.866025403784439,1.,0.866025403784439,1.,0.866025403784439,1.,0.866025403784439,
1.,0.866025403784439,1.,0.866025403784439,1.,0.866025403784439,1.,0.866025403784439,
1.,0.866025403784439,1.,0.866025403784439,1.,0.866025403784439,1.,0.866025403784439,
1.,0.866025403784439,1.,0.866025403784439,1.,0.866025403784439,1.,0.866025403784439,
1.,0.866025403784439,1.,0.866025403784439,1.,0.866025403784439,1.,0.866025403784439,
1.,0.866025403784439,1.,0.866025403784439,1.,0.866025403784439,1.,0.866025403784439,
1.,0.866025403784439,1.,0.866025403784439,1.,0.866025403784439,1.,0.866025403784439,
1.,0.866025403784439,1.,0.866025403784439,1.,0.866025403784439,1.,0.866025403784439,
1.,0.866025403784439,1.,0.866025403784439,1.,0.866025403784439,1.,0.866025403784439,
1.,0.866025403784439,1.,0.866025403784439,1.,0.866025403784439,1.,0.866025403784439,
1.,0.866025403784439,1.,0.866025403784439,1.,0.866025403784439,1.,0.866025403784439,
1.,0.866025403784439,1.,0.866025403784439,1.,0.866025403784439,1.,0.866025403784439,
1.,0.866025403784439,1.,0.866025403784439,1.,0.866025403784439,1.,0.866025403784439,
1.,0.866025403784439,1.,0.866025403784439,1.,0.866025403784439,1.,0.866025403784439,
1.,0.866025403784439,1.,0.866025403784439,1.,0.866025403784439,1.,0.866025403784439,
1.,0.866025403784439,1.,0.866025403784439,1.,0.866025403784439,1.,0.866025403784439,
1.,0.866025403784439,1.,0.866025403784439,1.,0.866025403784439,1.,0.866025403784439,
1.,0.866025403784439,1.,0.866025403784439,1.,0.866025403784439,1.,0.866025403784439,
1.,0.866025403784439,1.,0.866025403784439,1.,0.866025403784439,1.,0.866025403784439,
1.,0.866025403784439,1.,0.866025403784439,1.,0.866025403784439,1.,0.866025403784439,
1.,0.866025403784439,1.,0.866025403784439,1.,0.866025403784439,1.,0.866025403784439,
1.,0.866025403784439,1.,0.866025403784439,1.,0.866025403784439,1.,0.866025403784439,
1.,0.866025403784439,1.,0.866025403784439,1.,0.866025403784439,1.,0.866025403784439,
1.,0.866025403784439,1.,0.866025403784439,1.,0.866025403784439,1.,0.866025403784439,
1.,0.866025403784439,1.,0.866025403784439,1.,0.866025403784439,1.,0.866025403784439,
1.,0.866025403784439,1.,0.866025403784439,1.,0.866025403784439,1.,0.866025403784439,
1.,0.866025403784439,1.,0.866025403784439,1.,0.866025403784439,1.,0.866025403784439,
1.,0.866025403784439,1.,0.866025403784439,1.,0.866025403784439,1.,0.866025403784439,
1.,0.866025403784439,1.,0.866025403784439,1.,0.866025403784439,1.,0.866025403784439,
1.,0.866025403784439,1.,0.866025403784439,1.,0.866025403784439,1.,0.866025403784439,
1.,0.866025403784439,1.,0.866025403784439,1.,0.866025403784439,1.,0.866025403784439,
1.,0.866025403784439,1.,0.866025403784439,1.,0.866025403784439,1.,0.866025403784439,
1.,0.866025403784439,1.,0.866025403784439,1.,0.866025403784439,1.,0.866025403784439,
1.,0.866025403784439,1.,0.866025403784439,1.,0.866025403784439,1.,0.866025403784439,
1.,0.866025403784439,1.,0.866025403784439,1.,0.866025403784439,1.,0.866025403784439,
1.,0.866025403784439,1.,0.866025403784439,1.,0.866025403784439,1.,0.866025403784439,
1.,0.866025403784439,1.,0.866025403784439,1.,0.866025403784439,1.,0.866025403784439,
1.,0.866025403784439,1.,0.866025403784439,1.,0.866025403784439,1.,0.866025403784439,
1.,0.866025403784439,1.,0.866025403784439,1.,0.866025403784439,1.,0.866025403784439,
1.,0.866025403784439,1.,0.866025403784439,1.,0.866025403784439,1.,0.866025403784439,
1.,0.866025403784439,1.,0.866025403784439,1.,0.866025403784439,1.,0.866025403784439,
1.,0.866025403784439,1.,0.866025403784439,1.,0.866025403784439,1.,0.866025403784439,
1.,0.866025403784439,1.,0.866025403784439,1.,0.866025403784439,1.,0.866025403784439,
1.,0.866025403784439,1.,0.866025403784439,1.,0.866025403784439,1.,0.866025403784439,
1.,0.866025403784439,1.,0.866025403784439,1.,0.866025403784439,1.,0.866025403784439,
1.,0.866025403784439,1.,0.866025403784439,1.,0.866025403784439,1.,0.866025403784439,
1.,0.866025403784439,1.,0.866025403784439,1.,0.866025403784439,1.,0.866025403784439,
1.,0.866025403784439,1.,0.866025403784439,1.,0.866025403784439,1.,0.866025403784439,
1.,0.866025403784439,1.,0.866025403784439,1.,0.866025403784439,1.,0.866025403784439,
1.,0.866025403784439,1.,0.866025403784439,1.,0.866025403784439,1.,0.866025403784439,
1.,0.866025403784439,1.,0.866025403784439,1.,0.866025403784439,1.,0.866025403784439,
1.,0.866025403784439,1.,0.866025403784439,1.,0.866025403784439,1.,0.866025403784439,
1.,0.866025403784439,1.,0.866025403784439,1.,0.866025403784439,1.,0.866025403784439,
1.,0.866025403784439,1.,0.866025403784439,1.,0.866025403784439,1.,0.866025403784439,
1.,0.866025403784439,1.,0.866025403784439,1.,0.866025403784439,1.,0.866025403784439,
1.,0.866025403784439,1.,0.866025403784439,1.,0.866025403784439,1.,0.866025403784439,
1.,0.866025403784439,1.,0.866025403784439,1.,0.866025403784439,1.,0.866025403784439,
1.,0.866025403784439,1.,0.866025403784439,1.,0.866025403784439,1.,0.866025403784439,
1.,0.866025403784439,1.,0.866025403784439,1.,0.866025403784439,1.,0.866025403784439,
1.,0.866025403784439,1.,0.866025403784439,1.,0.866025403784439,1.,0.866025403784439,
1.,0.866025403784439,1.,0.866025403784439,1.,0.866025403784439,1.,0.866025403784439,
1.,0.866025403784439,1.,0.866025403784439,1.,0.866025403784439,1.,0.866025403784439,
1.,0.866025403784439,1.,0.866025403784439,1.,0.866025403784439,1.,0.866025403784439,
1.,0.866025403784439,1.,0.866025403784439,1.,0.866025403784439,1.,0.866025403784439,
1.,0.866025403784439,1.,0.866025403784439,1.,0.866025403784439,1.,0.866025403784439,
1.,0.866025403784439,1.,0.866025403784439,1.,0.866025403784439,1.,0.866025403784439,
1.,0.866025403784439,1.,0.866025403784439,1.,0.866025403784439,1.,0.866025403784439,
1.,0.866025403784439,1.,0.866025403784439,1.,0.866025403784439,1.,0.866025403784439,
1.,0.866025403784439,1.,0.866025403784439,1.,0.866025403784439,1.,0.866025403784439,
1.,0.866025403784439,1.,0.866025403784439,1.,0.866025403784439,1.,0.866025403784439,
1.,0.866025403784439,1.,0.866025403784439,1.,0.866025403784439,1.,0.866025403784439,
1.,0.866025403784439,1.,0.866025403784439,1.,0.866025403784439,1.,0.866025403784439,
1.,0.866025403784439,1.,0.866025403784439,1.,0.866025403784439,1.,0.866025403784439,
1.,0.866025403784439,1.,0.866025403784439,1.,0.866025403784439,1.,0.866025403784439,
1.,0.866025403784439,1.,0.866025403784439,1.,0.866025403784439,1.,0.866025403784439,
1.,0.866025403784439,1.,0.866025403784439,1.,0.866025403784439,1.,0.866025403784439,
1.,0.866025403784439,1.,0.866025403784439,1.,0.866025403784439,1.,0.866025403784439,
1.,0.866025403784439,1.,0.866025403784439,1.,0.866025403784439,1.,0.866025403784439,
1.,0.866025403784439,1.,0.866025403784439,1.,0.866025403784439,1.,0.866025403784439,
1.,0.866025403784439,1.,0.866025403784439,1.,0.866025403784439,1.,0.866025403784439,
1.,0.866025403784439,1.,0.866025403784439,1.,0.866025403784439,1.,0.866025403784439,
1.,0.866025403784439,1.,0.866025403784439,1.,0.866025403784439,1.,0.866025403784439,
1.,0.866025403784439,1.,0.866025403784439,1.,0.866025403784439,1.,0.866025403784439,
1.,0.866025403784439,1.,0.866025403784439,1.,0.866025403784439,1.,0.866025403784439,
1.,0.866025403784439,1.,0.866025403784439,1.,0.866025403784439,1.,0.866025403784439,
1.,0.866025403784439,1.,0.866025403784439,1.,0.866025403784439,1.,0.866025403784439,
1.,0.866025403784439,1.,0.866025403784439,1.,0.866025403784439,1.,0.866025403784439,
1.,0.866025403784439,1.,0.866025403784439,1.,0.866025403784439,1.,0.866025403784439,
1.,0.866025403784439,1.,0.866025403784439,1.,0.866025403784439,1.,0.866025403784439,
1.,0.866025403784439,1.,0.866025403784439,1.,0.866025403784439,1.,0.866025403784439,
1.,0.866025403784439,1.,0.866025403784439,1.,0.866025403784439,1.,0.866025403784439,
1.,0.866025403784439,1.,0.866025403784439,1.,0.866025403784439,1.,0.866025403784439,
1.,0.866025403784439,1.,0.866025403784439,1.,0.866025403784439,1.,0.866025403784439,
1.,0.866025403784439,1.,0.866025403784439,1.,0.866025403784439,1.,0.866025403784439,
1.,0.866025403784439,1.,0.866025403784439,1.,0.866025403784439,1.,0.866025403784439,
1.,0.866025403784439,1.,0.866025403784439,1.,0.866025403784439,1.,0.866025403784439,
1.,0.866025403784439,1.,0.866025403784439,1.,0.866025403784439,1.,0.866025403784439,
1.,0.866025403784439,1.,0.866025403784439,1.,0.866025403784439,1.,0.866025403784439,
1.,0.866025403784439,1.,0.866025403784439,1.,0.866025403784439,1.,0.866025403784439,
1.,0.866025403784439,1.,0.866025403784439,1.,0.866025403784439,1.,0.866025403784439,
1.,0.866025403784439,1.,0.866025403784439,1.,0.866025403784439,1.,0.866025403784439,
1.,0.866025403784439,1.,0.866025403784439,1.,0.866025403784439,1.,0.866025403784439,
1.,0.866025403784439,1.,0.866025403784439,1.,0.866025403784439,1.,0.866025403784439,
1.,0.866025403784439,1.,0.866025403784439,1.,0.866025403784439,1.,0.866025403784439,
1.,0.866025403784439,1.,0.866025403784439,1.,0.866025403784439,1.,0.866025403784439,
1.,0.866025403784439,1.,0.866025403784439,1.,0.866025403784439,1.,0.866025403784439,
1.,0.866025403784439,1.,0.866025403784439,1.,0.866025403784439,1.,0.866025403784439,
1.,0.866025403784439,1.,0.866025403784439,1.,0.866025403784439,1.,0.866025403784439,
1.,0.866025403784439,1.,0.866025403784439,1.,0.866025403784439,1.,0.866025403784439,
1.,0.866025403784439,1.,0.866025403784439,1.,0.866025403784439,1.,0.866025403784439,
1.,0.866025403784439,1.,0.866025403784439,1.,0.866025403784439,1.,0.866025403784439,
1.,0.866025403784439,1.,0.866025403784439,1.,0.866025403784439,1.,0.866025403784439,
1.,0.866025403784439,1.,0.866025403784439,1.,0.866025403784439,1.,0.866025403784439,
1.,0.866025403784439,1.,0.866025403784439,1.,0.866025403784439,1.,0.866025403784439,
1.,0.866025403784439,1.,0.866025403784439,1.,0.866025403784439,1.,0.866025403784439,
1.,0.866025403784439,1.,0.866025403784439,1.,0.866025403784439,1.,0.866025403784439,
1.),(1.,0.866025403784439,1.,0.866025403784439,1.,0.866025403784439,1.,
0.866025403784439,1.,0.866025403784439,1.,0.866025403784439,1.,0.866025403784439,
1.,0.866025403784439,1.,0.866025403784439,1.,0.866025403784439,1.,0.866025403784439,
1.,0.866025403784439,1.,0.866025403784439,1.,0.866025403784439,1.,0.866025403784439,
1.,0.866025403784439,1.,0.866025403784439,1.,0.866025403784439,1.,0.866025403784439,
1.,0.866025403784439,1.,0.866025403784439,1.,0.866025403784439,1.,0.866025403784439,
1.,0.866025403784439,1.,0.866025403784439,1.,0.866025403784439,1.,0.866025403784439,
1.,0.866025403784439,1.,0.866025403784439,1.,0.866025403784439,1.,0.866025403784439,
1.,0.866025403784439,1.,0.866025403784439,1.,0.866025403784439,1.,0.866025403784439,
1.,0.866025403784439,1.,0.866025403784439,1.,0.866025403784439,1.,0.866025403784439,
1.,0.866025403784439,1.,0.866025403784439,1.,0.866025403784439,1.,0.866025403784439,
1.,0.866025403784439,1.,0.866025403784439,1.,0.866025403784439,1.,0.866025403784439,
1.,0.866025403784439,1.,0.866025403784439,1.,0.866025403784439,1.,0.866025403784439,
1.,0.866025403784439,1.,0.866025403784439,1.,0.866025403784439,1.,0.866025403784439,
1.,0.866025403784439,1.,0.866025403784439,1.,0.866025403784439,1.,0.866025403784439,
1.,0.866025403784439,1.,0.866025403784439,1.,0.866025403784439,1.,0.866025403784439,
1.,0.866025403784439,1.,0.866025403784439,1.,0.866025403784439,1.,0.866025403784439,
1.,0.866025403784439,1.,0.866025403784439,1.,0.866025403784439,1.,0.866025403784439,
1.,0.866025403784439,1.,0.866025403784439,1.,0.866025403784439,1.,0.866025403784439,
1.,0.866025403784439,1.,0.866025403784439,1.,0.866025403784439,1.,0.866025403784439,
1.,0.866025403784439,1.,0.866025403784439,1.,0.866025403784439,1.,0.866025403784439,
1.,0.866025403784439,1.,0.866025403784439,1.,0.866025403784439,1.,0.866025403784439,
1.,0.866025403784439,1.,0.866025403784439,1.,0.866025403784439,1.,0.866025403784439,
1.,0.866025403784439,1.,0.866025403784439,1.,0.866025403784439,1.,0.866025403784439,
1.,0.866025403784439,1.,0.866025403784439,1.,0.866025403784439,1.,0.866025403784439,
1.,0.866025403784439,1.,0.866025403784439,1.,0.866025403784439,1.,0.866025403784439,
1.,0.866025403784439,1.,0.866025403784439,1.,0.866025403784439,1.,0.866025403784439,
1.,0.866025403784439,1.,0.866025403784439,1.,0.866025403784439,1.,0.866025403784439,
1.,0.866025403784439,1.,0.866025403784439,1.,0.866025403784439,1.,0.866025403784439,
1.,0.866025403784439,1.,0.866025403784439,1.,0.866025403784439,1.,0.866025403784439,
1.,0.866025403784439,1.,0.866025403784439,1.,0.866025403784439,1.,0.866025403784439,
1.,0.866025403784439,1.,0.866025403784439,1.,0.866025403784439,1.,0.866025403784439,
1.,0.866025403784439,1.,0.866025403784439,1.,0.866025403784439,1.,0.866025403784439,
1.,0.866025403784439,1.,0.866025403784439,1.,0.866025403784439,1.,0.866025403784439,
1.,0.866025403784439,1.,0.866025403784439,1.,0.866025403784439,1.,0.866025403784439,
1.,0.866025403784439,1.,0.866025403784439,1.,0.866025403784439,1.,0.866025403784439,
1.,0.866025403784439,1.,0.866025403784439,1.,0.866025403784439,1.,0.866025403784439,
1.,0.866025403784439,1.,0.866025403784439,1.,0.866025403784439,1.,0.866025403784439,
1.,0.866025403784439,1.,0.866025403784439,1.,0.866025403784439,1.,0.866025403784439,
1.,0.866025403784439,1.,0.866025403784439,1.,0.866025403784439,1.,0.866025403784439,
1.,0.866025403784439,1.,0.866025403784439,1.,0.866025403784439,1.,0.866025403784439,
1.,0.866025403784439,1.,0.866025403784439,1.,0.866025403784439,1.,0.866025403784439,
1.,0.866025403784439,1.,0.866025403784439,1.,0.866025403784439,1.,0.866025403784439,
1.,0.866025403784439,1.,0.866025403784439,1.,0.866025403784439,1.,0.866025403784439,
1.,0.866025403784439,1.,0.866025403784439,1.,0.866025403784439,1.,0.866025403784439,
1.,0.866025403784439,1.,0.866025403784439,1.,0.866025403784439,1.,0.866025403784439,
1.,0.866025403784439,1.,0.866025403784439,1.,0.866025403784439,1.,0.866025403784439,
1.,0.866025403784439,1.,0.866025403784439,1.,0.866025403784439,1.,0.866025403784439,
1.,0.866025403784439,1.,0.866025403784439,1.,0.866025403784439,1.,0.866025403784439,
1.,0.866025403784439,1.,0.866025403784439,1.,0.866025403784439,1.,0.866025403784439,
1.,0.866025403784439,1.,0.866025403784439,1.,0.866025403784439,1.,0.866025403784439,
1.,0.866025403784439,1.,0.866025403784439,1.,0.866025403784439,1.,0.866025403784439,
1.,0.866025403784439,1.,0.866025403784439,1.,0.866025403784439,1.,0.866025403784439,
1.,0.866025403784439,1.,0.866025403784439,1.,0.866025403784439,1.,0.866025403784439,
1.,0.866025403784439,1.,0.866025403784439,1.,0.866025403784439,1.,0.866025403784439,
1.,0.866025403784439,1.,0.866025403784439,1.,0.866025403784439,1.,0.866025403784439,
1.,0.866025403784439,1.,0.866025403784439,1.,0.866025403784439,1.,0.866025403784439,
1.,0.866025403784439,1.,0.866025403784439,1.,0.866025403784439,1.,0.866025403784439,
1.,0.866025403784439,1.,0.866025403784439,1.,0.866025403784439,1.,0.866025403784439,
1.,0.866025403784439,1.,0.866025403784439,1.,0.866025403784439,1.,0.866025403784439,
1.,0.866025403784439,1.,0.866025403784439,1.,0.866025403784439,1.,0.866025403784439,
1.,0.866025403784439,1.,0.866025403784439,1.,0.866025403784439,1.,0.866025403784439,
1.,0.866025403784439,1.,0.866025403784439,1.,0.866025403784439,1.,0.866025403784439,
1.,0.866025403784439,1.,0.866025403784439,1.,0.866025403784439,1.,0.866025403784439,
1.,0.866025403784439,1.,0.866025403784439,1.,0.866025403784439,1.,0.866025403784439,
1.,0.866025403784439,1.,0.866025403784439,1.,0.866025403784439,1.,0.866025403784439,
1.,0.866025403784439,1.,0.866025403784439,1.,0.866025403784439,1.,0.866025403784439,
1.,0.866025403784439,1.,0.866025403784439,1.,0.866025403784439,1.,0.866025403784439,
1.,0.866025403784439,1.,0.866025403784439,1.,0.866025403784439,1.,0.866025403784439,
1.,0.866025403784439,1.,0.866025403784439,1.,0.866025403784439,1.,0.866025403784439,
1.,0.866025403784439,1.,0.866025403784439,1.,0.866025403784439,1.,0.866025403784439,
1.,0.866025403784439,1.,0.866025403784439,1.,0.866025403784439,1.,0.866025403784439,
1.,0.866025403784439,1.,0.866025403784439,1.,0.866025403784439,1.,0.866025403784439,
1.,0.866025403784439,1.,0.866025403784439,1.,0.866025403784439,1.,0.866025403784439,
1.,0.866025403784439,1.,0.866025403784439,1.,0.866025403784439,1.,0.866025403784439,
1.,0.866025403784439,1.,0.866025403784439,1.,0.866025403784439,1.,0.866025403784439,
1.,0.866025403784439,1.,0.866025403784439,1.,0.866025403784439,1.,0.866025403784439,
1.,0.866025403784439,1.,0.866025403784439,1.,0.866025403784439,1.,0.866025403784439,
1.,0.866025403784439,1.,0.866025403784439,1.,0.866025403784439,1.,0.866025403784439,
1.,0.866025403784439,1.,0.866025403784439,1.,0.866025403784439,1.,0.866025403784439,
1.,0.866025403784439,1.,0.866025403784439,1.,0.866025403784439,1.,0.866025403784439,
1.,0.866025403784439,1.,0.866025403784439,1.,0.866025403784439,1.,0.866025403784439,
1.,0.866025403784439,1.,0.866025403784439,1.,0.866025403784439,1.,0.866025403784439,
1.,0.866025403784439,1.,0.866025403784439,1.,0.866025403784439,1.,0.866025403784439,
1.,0.866025403784439,1.,0.866025403784439,1.,0.866025403784439,1.,0.866025403784439,
1.,0.866025403784439,1.,0.866025403784439,1.,0.866025403784439,1.,0.866025403784439,
1.,0.866025403784439,1.,0.866025403784439,1.,0.866025403784439,1.,0.866025403784439,
1.,0.866025403784439,1.,0.866025403784439,1.,0.866025403784439,1.,0.866025403784439,
1.,0.866025403784439,1.,0.866025403784439,1.,0.866025403784439,1.,0.866025403784439,
1.,0.866025403784439,1.,0.866025403784439,1.,0.866025403784439,1.,0.866025403784439,
1.,0.866025403784439,1.,0.866025403784439,1.,0.866025403784439,1.,0.866025403784439,
1.,0.866025403784439,1.,0.866025403784439,1.,0.866025403784439,1.,0.866025403784439,
1.,0.866025403784439,1.,0.866025403784439,1.,0.866025403784439,1.,0.866025403784439,
1.,0.866025403784439,1.,0.866025403784439,1.,0.866025403784439,1.,0.866025403784439,
1.,0.866025403784439,1.,0.866025403784439,1.,0.866025403784439,1.,0.866025403784439,
1.,0.866025403784439,1.,0.866025403784439,1.,0.866025403784439,1.,0.866025403784439,
1.,0.866025403784439,1.,0.866025403784439,1.,0.866025403784439,1.,0.866025403784439,
1.,0.866025403784439,1.,0.866025403784439,1.,0.866025403784439,1.,0.866025403784439,
1.,0.866025403784439,1.,0.866025403784439,1.,0.866025403784439,1.,0.866025403784439,
1.,0.866025403784439,1.,0.866025403784439,1.,0.866025403784439,1.,0.866025403784439,
1.,0.866025403784439,1.,0.866025403784439,1.,0.866025403784439,1.,0.866025403784439,
1.,0.866025403784439,1.,0.866025403784439,1.,0.866025403784439,1.,0.866025403784439,
1.,0.866025403784439,1.,0.866025403784439,1.,0.866025403784439,1.,0.866025403784439,
1.,0.866025403784439,1.,0.866025403784439,1.,0.866025403784439,1.,0.866025403784439,
1.,0.866025403784439,1.,0.866025403784439,1.,0.866025403784439,1.,0.866025403784439,
1.,0.866025403784439,1.,0.866025403784439,1.,0.866025403784439,1.,0.866025403784439,
1.,0.866025403784439,1.,0.866025403784439,1.,0.866025403784439,1.,0.866025403784439,
1.,0.866025403784439,1.,0.866025403784439,1.,0.866025403784439,1.,0.866025403784439,
1.,0.866025403784439,1.,0.866025403784439,1.,0.866025403784439,1.,0.866025403784439,
1.,0.866025403784439,1.,0.866025403784439,1.,0.866025403784439,1.,0.866025403784439,
1.,0.866025403784439,1.,0.866025403784439,1.,0.866025403784439,1.,0.866025403784439,
1.,0.866025403784439,1.,0.866025403784439,1.,0.866025403784439,1.,0.866025403784439,
1.,0.866025403784439,1.,0.866025403784439,1.,0.866025403784439,1.,0.866025403784439,
1.,0.866025403784439,1.,0.866025403784439,1.,0.866025403784439,1.,0.866025403784439,
1.,0.866025403784439,1.,0.866025403784439,1.,0.866025403784439,1.,0.866025403784439,
1.,0.866025403784439,1.,0.866025403784439,1.,0.866025403784439,1.,0.866025403784439,
1.,0.866025403784439,1.,0.866025403784439,1.,0.866025403784439,1.,0.866025403784439,
1.,0.866025403784439,1.,0.866025403784439,1.,0.866025403784439,1.,0.866025403784439,
1.,0.866025403784439,1.,0.866025403784439,1.,0.866025403784439,1.,0.866025403784439,
1.,0.866025403784439,1.,0.866025403784439,1.,0.866025403784439,1.,0.866025403784439,
1.,0.866025403784439,1.,0.866025403784439,1.,0.866025403784439,1.,0.866025403784439,
1.,0.866025403784439,1.,0.866025403784439,1.,0.866025403784439,1.)))
REPRESENTATION_ITEM('')
SURFACE()
);
#149=(
BOUNDED_SURFACE()
B_SPLINE_SURFACE(3,2,((#15547,#15548,#15549,#15550,#15551,#15552,#15553,
#15554,#15555,#15556,#15557,#15558,#15559,#15560,#15561,#15562,#15563,#15564,
#15565,#15566,#15567,#15568,#15569,#15570,#15571,#15572,#15573,#15574,#15575,
#15576,#15577,#15578,#15579,#15580,#15581,#15582,#15583,#15584,#15585,#15586,
#15587,#15588,#15589,#15590,#15591,#15592,#15593,#15594,#15595,#15596,#15597,
#15598,#15599,#15600,#15601,#15602,#15603,#15604,#15605,#15606,#15607,#15608,
#15609,#15610,#15611,#15612,#15613,#15614,#15615,#15616,#15617,#15618,#15619,
#15620,#15621,#15622,#15623,#15624,#15625,#15626,#15627,#15628,#15629,#15630,
#15631,#15632,#15633,#15634,#15635,#15636,#15637,#15638,#15639,#15640,#15641,
#15642,#15643,#15644,#15645,#15646,#15647,#15648,#15649,#15650,#15651,#15652,
#15653,#15654,#15655,#15656,#15657,#15658,#15659,#15660,#15661,#15662,#15663,
#15664,#15665,#15666,#15667,#15668,#15669,#15670,#15671,#15672,#15673,#15674,
#15675,#15676,#15677,#15678,#15679,#15680,#15681,#15682,#15683,#15684,#15685,
#15686,#15687,#15688,#15689,#15690,#15691,#15692,#15693,#15694,#15695,#15696,
#15697,#15698,#15699,#15700,#15701,#15702,#15703,#15704,#15705,#15706,#15707,
#15708,#15709,#15710,#15711,#15712,#15713,#15714,#15715,#15716,#15717,#15718,
#15719,#15720,#15721,#15722,#15723,#15724,#15725,#15726,#15727,#15728,#15729,
#15730,#15731,#15732,#15733,#15734,#15735,#15736,#15737,#15738,#15739,#15740,
#15741,#15742,#15743,#15744,#15745,#15746,#15747,#15748,#15749,#15750,#15751,
#15752,#15753,#15754,#15755,#15756,#15757,#15758,#15759,#15760,#15761,#15762,
#15763,#15764,#15765,#15766,#15767,#15768,#15769,#15770,#15771,#15772,#15773,
#15774,#15775,#15776,#15777,#15778,#15779,#15780,#15781,#15782,#15783,#15784,
#15785,#15786,#15787,#15788,#15789,#15790,#15791,#15792,#15793,#15794,#15795,
#15796,#15797,#15798,#15799,#15800,#15801,#15802,#15803,#15804,#15805,#15806,
#15807,#15808,#15809,#15810,#15811,#15812,#15813,#15814,#15815,#15816,#15817,
#15818,#15819,#15820,#15821,#15822,#15823,#15824,#15825,#15826,#15827,#15828,
#15829,#15830,#15831,#15832,#15833,#15834,#15835,#15836,#15837,#15838,#15839,
#15840,#15841,#15842,#15843,#15844,#15845,#15846,#15847,#15848,#15849,#15850,
#15851,#15852,#15853,#15854,#15855,#15856,#15857,#15858,#15859,#15860,#15861,
#15862,#15863,#15864,#15865,#15866,#15867,#15868,#15869,#15870,#15871,#15872,
#15873,#15874,#15875,#15876,#15877,#15878,#15879,#15880,#15881,#15882,#15883,
#15884,#15885,#15886,#15887,#15888,#15889,#15890,#15891,#15892,#15893,#15894,
#15895,#15896,#15897,#15898,#15899,#15900,#15901,#15902,#15903,#15904,#15905,
#15906,#15907,#15908,#15909,#15910,#15911,#15912,#15913,#15914,#15915,#15916,
#15917,#15918,#15919,#15920,#15921,#15922,#15923,#15924,#15925,#15926,#15927,
#15928,#15929,#15930,#15931,#15932,#15933,#15934,#15935,#15936,#15937,#15938,
#15939,#15940,#15941,#15942,#15943,#15944,#15945,#15946,#15947,#15948,#15949,
#15950,#15951,#15952,#15953,#15954,#15955,#15956,#15957,#15958,#15959,#15960,
#15961,#15962,#15963,#15964,#15965,#15966,#15967,#15968,#15969,#15970,#15971,
#15972,#15973,#15974,#15975,#15976,#15977,#15978,#15979,#15980,#15981,#15982,
#15983,#15984,#15985,#15986,#15987,#15988,#15989,#15990,#15991,#15992,#15993,
#15994,#15995,#15996,#15997,#15998,#15999,#16000,#16001,#16002,#16003,#16004,
#16005,#16006,#16007,#16008,#16009,#16010,#16011,#16012,#16013,#16014,#16015,
#16016,#16017,#16018,#16019,#16020,#16021,#16022,#16023,#16024,#16025,#16026,
#16027,#16028,#16029,#16030,#16031,#16032,#16033,#16034,#16035,#16036,#16037,
#16038,#16039,#16040,#16041,#16042,#16043,#16044,#16045,#16046,#16047,#16048,
#16049,#16050,#16051,#16052,#16053,#16054,#16055,#16056,#16057,#16058,#16059,
#16060,#16061,#16062,#16063,#16064,#16065,#16066,#16067,#16068,#16069,#16070,
#16071,#16072,#16073,#16074,#16075,#16076,#16077,#16078,#16079,#16080,#16081,
#16082,#16083,#16084,#16085,#16086,#16087,#16088,#16089,#16090,#16091,#16092,
#16093,#16094,#16095,#16096,#16097,#16098,#16099,#16100,#16101,#16102,#16103,
#16104,#16105,#16106,#16107,#16108,#16109,#16110,#16111,#16112,#16113,#16114,
#16115,#16116,#16117,#16118,#16119,#16120,#16121,#16122,#16123,#16124,#16125,
#16126,#16127,#16128,#16129,#16130,#16131,#16132,#16133,#16134,#16135,#16136,
#16137,#16138,#16139,#16140,#16141,#16142,#16143,#16144,#16145,#16146,#16147,
#16148,#16149,#16150,#16151,#16152,#16153,#16154,#16155,#16156,#16157,#16158,
#16159,#16160,#16161,#16162,#16163,#16164,#16165,#16166,#16167,#16168,#16169,
#16170,#16171,#16172,#16173,#16174,#16175,#16176,#16177,#16178,#16179,#16180,
#16181,#16182,#16183,#16184,#16185,#16186,#16187,#16188,#16189,#16190,#16191,
#16192,#16193,#16194,#16195,#16196,#16197,#16198,#16199,#16200,#16201,#16202,
#16203,#16204,#16205,#16206,#16207,#16208,#16209,#16210,#16211,#16212,#16213,
#16214,#16215,#16216,#16217,#16218,#16219,#16220,#16221,#16222,#16223,#16224,
#16225,#16226,#16227,#16228,#16229,#16230,#16231,#16232,#16233,#16234,#16235,
#16236,#16237,#16238,#16239,#16240,#16241,#16242,#16243,#16244,#16245,#16246,
#16247,#16248,#16249,#16250,#16251,#16252,#16253,#16254,#16255,#16256,#16257,
#16258,#16259,#16260,#16261,#16262,#16263,#16264,#16265,#16266,#16267,#16268,
#16269,#16270,#16271,#16272,#16273,#16274,#16275,#16276,#16277,#16278,#16279,
#16280,#16281,#16282,#16283,#16284,#16285,#16286,#16287,#16288,#16289,#16290,
#16291,#16292,#16293,#16294,#16295,#16296,#16297,#16298,#16299,#16300,#16301,
#16302,#16303,#16304,#16305,#16306,#16307,#16308,#16309,#16310,#16311,#16312,
#16313,#16314,#16315,#16316,#16317,#16318,#16319,#16320,#16321,#16322,#16323,
#16324,#16325,#16326,#16327,#16328,#16329,#16330,#16331,#16332,#16333,#16334,
#16335,#16336,#16337,#16338,#16339,#16340,#16341,#16342,#16343,#16344,#16345,
#16346,#16347,#16348,#16349,#16350,#16351,#16352,#16353,#16354,#16355,#16356,
#16357,#16358,#16359,#16360,#16361,#16362,#16363,#16364,#16365,#16366,#16367,
#16368,#16369,#16370,#16371,#16372,#16373,#16374,#16375,#16376,#16377,#16378,
#16379,#16380,#16381,#16382,#16383,#16384,#16385,#16386,#16387,#16388,#16389,
#16390,#16391,#16392,#16393,#16394,#16395,#16396,#16397,#16398,#16399,#16400,
#16401,#16402,#16403,#16404,#16405,#16406,#16407,#16408,#16409,#16410,#16411,
#16412,#16413,#16414,#16415,#16416,#16417,#16418,#16419,#16420,#16421,#16422,
#16423,#16424,#16425,#16426,#16427,#16428,#16429,#16430,#16431,#16432,#16433,
#16434,#16435,#16436,#16437,#16438,#16439,#16440,#16441,#16442,#16443,#16444,
#16445,#16446,#16447,#16448,#16449,#16450,#16451,#16452,#16453,#16454,#16455,
#16456,#16457,#16458,#16459,#16460,#16461,#16462,#16463,#16464,#16465,#16466,
#16467,#16468,#16469,#16470,#16471,#16472,#16473,#16474,#16475,#16476,#16477,
#16478,#16479,#16480,#16481,#16482,#16483,#16484,#16485,#16486,#16487,#16488,
#16489,#16490,#16491,#16492,#16493,#16494,#16495,#16496,#16497,#16498,#16499,
#16500,#16501,#16502,#16503,#16504,#16505,#16506,#16507,#16508,#16509,#16510,
#16511,#16512,#16513,#16514,#16515,#16516,#16517,#16518,#16519),(#16520,
#16521,#16522,#16523,#16524,#16525,#16526,#16527,#16528,#16529,#16530,#16531,
#16532,#16533,#16534,#16535,#16536,#16537,#16538,#16539,#16540,#16541,#16542,
#16543,#16544,#16545,#16546,#16547,#16548,#16549,#16550,#16551,#16552,#16553,
#16554,#16555,#16556,#16557,#16558,#16559,#16560,#16561,#16562,#16563,#16564,
#16565,#16566,#16567,#16568,#16569,#16570,#16571,#16572,#16573,#16574,#16575,
#16576,#16577,#16578,#16579,#16580,#16581,#16582,#16583,#16584,#16585,#16586,
#16587,#16588,#16589,#16590,#16591,#16592,#16593,#16594,#16595,#16596,#16597,
#16598,#16599,#16600,#16601,#16602,#16603,#16604,#16605,#16606,#16607,#16608,
#16609,#16610,#16611,#16612,#16613,#16614,#16615,#16616,#16617,#16618,#16619,
#16620,#16621,#16622,#16623,#16624,#16625,#16626,#16627,#16628,#16629,#16630,
#16631,#16632,#16633,#16634,#16635,#16636,#16637,#16638,#16639,#16640,#16641,
#16642,#16643,#16644,#16645,#16646,#16647,#16648,#16649,#16650,#16651,#16652,
#16653,#16654,#16655,#16656,#16657,#16658,#16659,#16660,#16661,#16662,#16663,
#16664,#16665,#16666,#16667,#16668,#16669,#16670,#16671,#16672,#16673,#16674,
#16675,#16676,#16677,#16678,#16679,#16680,#16681,#16682,#16683,#16684,#16685,
#16686,#16687,#16688,#16689,#16690,#16691,#16692,#16693,#16694,#16695,#16696,
#16697,#16698,#16699,#16700,#16701,#16702,#16703,#16704,#16705,#16706,#16707,
#16708,#16709,#16710,#16711,#16712,#16713,#16714,#16715,#16716,#16717,#16718,
#16719,#16720,#16721,#16722,#16723,#16724,#16725,#16726,#16727,#16728,#16729,
#16730,#16731,#16732,#16733,#16734,#16735,#16736,#16737,#16738,#16739,#16740,
#16741,#16742,#16743,#16744,#16745,#16746,#16747,#16748,#16749,#16750,#16751,
#16752,#16753,#16754,#16755,#16756,#16757,#16758,#16759,#16760,#16761,#16762,
#16763,#16764,#16765,#16766,#16767,#16768,#16769,#16770,#16771,#16772,#16773,
#16774,#16775,#16776,#16777,#16778,#16779,#16780,#16781,#16782,#16783,#16784,
#16785,#16786,#16787,#16788,#16789,#16790,#16791,#16792,#16793,#16794,#16795,
#16796,#16797,#16798,#16799,#16800,#16801,#16802,#16803,#16804,#16805,#16806,
#16807,#16808,#16809,#16810,#16811,#16812,#16813,#16814,#16815,#16816,#16817,
#16818,#16819,#16820,#16821,#16822,#16823,#16824,#16825,#16826,#16827,#16828,
#16829,#16830,#16831,#16832,#16833,#16834,#16835,#16836,#16837,#16838,#16839,
#16840,#16841,#16842,#16843,#16844,#16845,#16846,#16847,#16848,#16849,#16850,
#16851,#16852,#16853,#16854,#16855,#16856,#16857,#16858,#16859,#16860,#16861,
#16862,#16863,#16864,#16865,#16866,#16867,#16868,#16869,#16870,#16871,#16872,
#16873,#16874,#16875,#16876,#16877,#16878,#16879,#16880,#16881,#16882,#16883,
#16884,#16885,#16886,#16887,#16888,#16889,#16890,#16891,#16892,#16893,#16894,
#16895,#16896,#16897,#16898,#16899,#16900,#16901,#16902,#16903,#16904,#16905,
#16906,#16907,#16908,#16909,#16910,#16911,#16912,#16913,#16914,#16915,#16916,
#16917,#16918,#16919,#16920,#16921,#16922,#16923,#16924,#16925,#16926,#16927,
#16928,#16929,#16930,#16931,#16932,#16933,#16934,#16935,#16936,#16937,#16938,
#16939,#16940,#16941,#16942,#16943,#16944,#16945,#16946,#16947,#16948,#16949,
#16950,#16951,#16952,#16953,#16954,#16955,#16956,#16957,#16958,#16959,#16960,
#16961,#16962,#16963,#16964,#16965,#16966,#16967,#16968,#16969,#16970,#16971,
#16972,#16973,#16974,#16975,#16976,#16977,#16978,#16979,#16980,#16981,#16982,
#16983,#16984,#16985,#16986,#16987,#16988,#16989,#16990,#16991,#16992,#16993,
#16994,#16995,#16996,#16997,#16998,#16999,#17000,#17001,#17002,#17003,#17004,
#17005,#17006,#17007,#17008,#17009,#17010,#17011,#17012,#17013,#17014,#17015,
#17016,#17017,#17018,#17019,#17020,#17021,#17022,#17023,#17024,#17025,#17026,
#17027,#17028,#17029,#17030,#17031,#17032,#17033,#17034,#17035,#17036,#17037,
#17038,#17039,#17040,#17041,#17042,#17043,#17044,#17045,#17046,#17047,#17048,
#17049,#17050,#17051,#17052,#17053,#17054,#17055,#17056,#17057,#17058,#17059,
#17060,#17061,#17062,#17063,#17064,#17065,#17066,#17067,#17068,#17069,#17070,
#17071,#17072,#17073,#17074,#17075,#17076,#17077,#17078,#17079,#17080,#17081,
#17082,#17083,#17084,#17085,#17086,#17087,#17088,#17089,#17090,#17091,#17092,
#17093,#17094,#17095,#17096,#17097,#17098,#17099,#17100,#17101,#17102,#17103,
#17104,#17105,#17106,#17107,#17108,#17109,#17110,#17111,#17112,#17113,#17114,
#17115,#17116,#17117,#17118,#17119,#17120,#17121,#17122,#17123,#17124,#17125,
#17126,#17127,#17128,#17129,#17130,#17131,#17132,#17133,#17134,#17135,#17136,
#17137,#17138,#17139,#17140,#17141,#17142,#17143,#17144,#17145,#17146,#17147,
#17148,#17149,#17150,#17151,#17152,#17153,#17154,#17155,#17156,#17157,#17158,
#17159,#17160,#17161,#17162,#17163,#17164,#17165,#17166,#17167,#17168,#17169,
#17170,#17171,#17172,#17173,#17174,#17175,#17176,#17177,#17178,#17179,#17180,
#17181,#17182,#17183,#17184,#17185,#17186,#17187,#17188,#17189,#17190,#17191,
#17192,#17193,#17194,#17195,#17196,#17197,#17198,#17199,#17200,#17201,#17202,
#17203,#17204,#17205,#17206,#17207,#17208,#17209,#17210,#17211,#17212,#17213,
#17214,#17215,#17216,#17217,#17218,#17219,#17220,#17221,#17222,#17223,#17224,
#17225,#17226,#17227,#17228,#17229,#17230,#17231,#17232,#17233,#17234,#17235,
#17236,#17237,#17238,#17239,#17240,#17241,#17242,#17243,#17244,#17245,#17246,
#17247,#17248,#17249,#17250,#17251,#17252,#17253,#17254,#17255,#17256,#17257,
#17258,#17259,#17260,#17261,#17262,#17263,#17264,#17265,#17266,#17267,#17268,
#17269,#17270,#17271,#17272,#17273,#17274,#17275,#17276,#17277,#17278,#17279,
#17280,#17281,#17282,#17283,#17284,#17285,#17286,#17287,#17288,#17289,#17290,
#17291,#17292,#17293,#17294,#17295,#17296,#17297,#17298,#17299,#17300,#17301,
#17302,#17303,#17304,#17305,#17306,#17307,#17308,#17309,#17310,#17311,#17312,
#17313,#17314,#17315,#17316,#17317,#17318,#17319,#17320,#17321,#17322,#17323,
#17324,#17325,#17326,#17327,#17328,#17329,#17330,#17331,#17332,#17333,#17334,
#17335,#17336,#17337,#17338,#17339,#17340,#17341,#17342,#17343,#17344,#17345,
#17346,#17347,#17348,#17349,#17350,#17351,#17352,#17353,#17354,#17355,#17356,
#17357,#17358,#17359,#17360,#17361,#17362,#17363,#17364,#17365,#17366,#17367,
#17368,#17369,#17370,#17371,#17372,#17373,#17374,#17375,#17376,#17377,#17378,
#17379,#17380,#17381,#17382,#17383,#17384,#17385,#17386,#17387,#17388,#17389,
#17390,#17391,#17392,#17393,#17394,#17395,#17396,#17397,#17398,#17399,#17400,
#17401,#17402,#17403,#17404,#17405,#17406,#17407,#17408,#17409,#17410,#17411,
#17412,#17413,#17414,#17415,#17416,#17417,#17418,#17419,#17420,#17421,#17422,
#17423,#17424,#17425,#17426,#17427,#17428,#17429,#17430,#17431,#17432,#17433,
#17434,#17435,#17436,#17437,#17438,#17439,#17440,#17441,#17442,#17443,#17444,
#17445,#17446,#17447,#17448,#17449,#17450,#17451,#17452,#17453,#17454,#17455,
#17456,#17457,#17458,#17459,#17460,#17461,#17462,#17463,#17464,#17465,#17466,
#17467,#17468,#17469,#17470,#17471,#17472,#17473,#17474,#17475,#17476,#17477,
#17478,#17479,#17480,#17481,#17482,#17483,#17484,#17485,#17486,#17487,#17488,
#17489,#17490,#17491,#17492),(#17493,#17494,#17495,#17496,#17497,#17498,
#17499,#17500,#17501,#17502,#17503,#17504,#17505,#17506,#17507,#17508,#17509,
#17510,#17511,#17512,#17513,#17514,#17515,#17516,#17517,#17518,#17519,#17520,
#17521,#17522,#17523,#17524,#17525,#17526,#17527,#17528,#17529,#17530,#17531,
#17532,#17533,#17534,#17535,#17536,#17537,#17538,#17539,#17540,#17541,#17542,
#17543,#17544,#17545,#17546,#17547,#17548,#17549,#17550,#17551,#17552,#17553,
#17554,#17555,#17556,#17557,#17558,#17559,#17560,#17561,#17562,#17563,#17564,
#17565,#17566,#17567,#17568,#17569,#17570,#17571,#17572,#17573,#17574,#17575,
#17576,#17577,#17578,#17579,#17580,#17581,#17582,#17583,#17584,#17585,#17586,
#17587,#17588,#17589,#17590,#17591,#17592,#17593,#17594,#17595,#17596,#17597,
#17598,#17599,#17600,#17601,#17602,#17603,#17604,#17605,#17606,#17607,#17608,
#17609,#17610,#17611,#17612,#17613,#17614,#17615,#17616,#17617,#17618,#17619,
#17620,#17621,#17622,#17623,#17624,#17625,#17626,#17627,#17628,#17629,#17630,
#17631,#17632,#17633,#17634,#17635,#17636,#17637,#17638,#17639,#17640,#17641,
#17642,#17643,#17644,#17645,#17646,#17647,#17648,#17649,#17650,#17651,#17652,
#17653,#17654,#17655,#17656,#17657,#17658,#17659,#17660,#17661,#17662,#17663,
#17664,#17665,#17666,#17667,#17668,#17669,#17670,#17671,#17672,#17673,#17674,
#17675,#17676,#17677,#17678,#17679,#17680,#17681,#17682,#17683,#17684,#17685,
#17686,#17687,#17688,#17689,#17690,#17691,#17692,#17693,#17694,#17695,#17696,
#17697,#17698,#17699,#17700,#17701,#17702,#17703,#17704,#17705,#17706,#17707,
#17708,#17709,#17710,#17711,#17712,#17713,#17714,#17715,#17716,#17717,#17718,
#17719,#17720,#17721,#17722,#17723,#17724,#17725,#17726,#17727,#17728,#17729,
#17730,#17731,#17732,#17733,#17734,#17735,#17736,#17737,#17738,#17739,#17740,
#17741,#17742,#17743,#17744,#17745,#17746,#17747,#17748,#17749,#17750,#17751,
#17752,#17753,#17754,#17755,#17756,#17757,#17758,#17759,#17760,#17761,#17762,
#17763,#17764,#17765,#17766,#17767,#17768,#17769,#17770,#17771,#17772,#17773,
#17774,#17775,#17776,#17777,#17778,#17779,#17780,#17781,#17782,#17783,#17784,
#17785,#17786,#17787,#17788,#17789,#17790,#17791,#17792,#17793,#17794,#17795,
#17796,#17797,#17798,#17799,#17800,#17801,#17802,#17803,#17804,#17805,#17806,
#17807,#17808,#17809,#17810,#17811,#17812,#17813,#17814,#17815,#17816,#17817,
#17818,#17819,#17820,#17821,#17822,#17823,#17824,#17825,#17826,#17827,#17828,
#17829,#17830,#17831,#17832,#17833,#17834,#17835,#17836,#17837,#17838,#17839,
#17840,#17841,#17842,#17843,#17844,#17845,#17846,#17847,#17848,#17849,#17850,
#17851,#17852,#17853,#17854,#17855,#17856,#17857,#17858,#17859,#17860,#17861,
#17862,#17863,#17864,#17865,#17866,#17867,#17868,#17869,#17870,#17871,#17872,
#17873,#17874,#17875,#17876,#17877,#17878,#17879,#17880,#17881,#17882,#17883,
#17884,#17885,#17886,#17887,#17888,#17889,#17890,#17891,#17892,#17893,#17894,
#17895,#17896,#17897,#17898,#17899,#17900,#17901,#17902,#17903,#17904,#17905,
#17906,#17907,#17908,#17909,#17910,#17911,#17912,#17913,#17914,#17915,#17916,
#17917,#17918,#17919,#17920,#17921,#17922,#17923,#17924,#17925,#17926,#17927,
#17928,#17929,#17930,#17931,#17932,#17933,#17934,#17935,#17936,#17937,#17938,
#17939,#17940,#17941,#17942,#17943,#17944,#17945,#17946,#17947,#17948,#17949,
#17950,#17951,#17952,#17953,#17954,#17955,#17956,#17957,#17958,#17959,#17960,
#17961,#17962,#17963,#17964,#17965,#17966,#17967,#17968,#17969,#17970,#17971,
#17972,#17973,#17974,#17975,#17976,#17977,#17978,#17979,#17980,#17981,#17982,
#17983,#17984,#17985,#17986,#17987,#17988,#17989,#17990,#17991,#17992,#17993,
#17994,#17995,#17996,#17997,#17998,#17999,#18000,#18001,#18002,#18003,#18004,
#18005,#18006,#18007,#18008,#18009,#18010,#18011,#18012,#18013,#18014,#18015,
#18016,#18017,#18018,#18019,#18020,#18021,#18022,#18023,#18024,#18025,#18026,
#18027,#18028,#18029,#18030,#18031,#18032,#18033,#18034,#18035,#18036,#18037,
#18038,#18039,#18040,#18041,#18042,#18043,#18044,#18045,#18046,#18047,#18048,
#18049,#18050,#18051,#18052,#18053,#18054,#18055,#18056,#18057,#18058,#18059,
#18060,#18061,#18062,#18063,#18064,#18065,#18066,#18067,#18068,#18069,#18070,
#18071,#18072,#18073,#18074,#18075,#18076,#18077,#18078,#18079,#18080,#18081,
#18082,#18083,#18084,#18085,#18086,#18087,#18088,#18089,#18090,#18091,#18092,
#18093,#18094,#18095,#18096,#18097,#18098,#18099,#18100,#18101,#18102,#18103,
#18104,#18105,#18106,#18107,#18108,#18109,#18110,#18111,#18112,#18113,#18114,
#18115,#18116,#18117,#18118,#18119,#18120,#18121,#18122,#18123,#18124,#18125,
#18126,#18127,#18128,#18129,#18130,#18131,#18132,#18133,#18134,#18135,#18136,
#18137,#18138,#18139,#18140,#18141,#18142,#18143,#18144,#18145,#18146,#18147,
#18148,#18149,#18150,#18151,#18152,#18153,#18154,#18155,#18156,#18157,#18158,
#18159,#18160,#18161,#18162,#18163,#18164,#18165,#18166,#18167,#18168,#18169,
#18170,#18171,#18172,#18173,#18174,#18175,#18176,#18177,#18178,#18179,#18180,
#18181,#18182,#18183,#18184,#18185,#18186,#18187,#18188,#18189,#18190,#18191,
#18192,#18193,#18194,#18195,#18196,#18197,#18198,#18199,#18200,#18201,#18202,
#18203,#18204,#18205,#18206,#18207,#18208,#18209,#18210,#18211,#18212,#18213,
#18214,#18215,#18216,#18217,#18218,#18219,#18220,#18221,#18222,#18223,#18224,
#18225,#18226,#18227,#18228,#18229,#18230,#18231,#18232,#18233,#18234,#18235,
#18236,#18237,#18238,#18239,#18240,#18241,#18242,#18243,#18244,#18245,#18246,
#18247,#18248,#18249,#18250,#18251,#18252,#18253,#18254,#18255,#18256,#18257,
#18258,#18259,#18260,#18261,#18262,#18263,#18264,#18265,#18266,#18267,#18268,
#18269,#18270,#18271,#18272,#18273,#18274,#18275,#18276,#18277,#18278,#18279,
#18280,#18281,#18282,#18283,#18284,#18285,#18286,#18287,#18288,#18289,#18290,
#18291,#18292,#18293,#18294,#18295,#18296,#18297,#18298,#18299,#18300,#18301,
#18302,#18303,#18304,#18305,#18306,#18307,#18308,#18309,#18310,#18311,#18312,
#18313,#18314,#18315,#18316,#18317,#18318,#18319,#18320,#18321,#18322,#18323,
#18324,#18325,#18326,#18327,#18328,#18329,#18330,#18331,#18332,#18333,#18334,
#18335,#18336,#18337,#18338,#18339,#18340,#18341,#18342,#18343,#18344,#18345,
#18346,#18347,#18348,#18349,#18350,#18351,#18352,#18353,#18354,#18355,#18356,
#18357,#18358,#18359,#18360,#18361,#18362,#18363,#18364,#18365,#18366,#18367,
#18368,#18369,#18370,#18371,#18372,#18373,#18374,#18375,#18376,#18377,#18378,
#18379,#18380,#18381,#18382,#18383,#18384,#18385,#18386,#18387,#18388,#18389,
#18390,#18391,#18392,#18393,#18394,#18395,#18396,#18397,#18398,#18399,#18400,
#18401,#18402,#18403,#18404,#18405,#18406,#18407,#18408,#18409,#18410,#18411,
#18412,#18413,#18414,#18415,#18416,#18417,#18418,#18419,#18420,#18421,#18422,
#18423,#18424,#18425,#18426,#18427,#18428,#18429,#18430,#18431,#18432,#18433,
#18434,#18435,#18436,#18437,#18438,#18439,#18440,#18441,#18442,#18443,#18444,
#18445,#18446,#18447,#18448,#18449,#18450,#18451,#18452,#18453,#18454,#18455,
#18456,#18457,#18458,#18459,#18460,#18461,#18462,#18463,#18464,#18465),
(#18466,#18467,#18468,#18469,#18470,#18471,#18472,#18473,#18474,#18475,
#18476,#18477,#18478,#18479,#18480,#18481,#18482,#18483,#18484,#18485,#18486,
#18487,#18488,#18489,#18490,#18491,#18492,#18493,#18494,#18495,#18496,#18497,
#18498,#18499,#18500,#18501,#18502,#18503,#18504,#18505,#18506,#18507,#18508,
#18509,#18510,#18511,#18512,#18513,#18514,#18515,#18516,#18517,#18518,#18519,
#18520,#18521,#18522,#18523,#18524,#18525,#18526,#18527,#18528,#18529,#18530,
#18531,#18532,#18533,#18534,#18535,#18536,#18537,#18538,#18539,#18540,#18541,
#18542,#18543,#18544,#18545,#18546,#18547,#18548,#18549,#18550,#18551,#18552,
#18553,#18554,#18555,#18556,#18557,#18558,#18559,#18560,#18561,#18562,#18563,
#18564,#18565,#18566,#18567,#18568,#18569,#18570,#18571,#18572,#18573,#18574,
#18575,#18576,#18577,#18578,#18579,#18580,#18581,#18582,#18583,#18584,#18585,
#18586,#18587,#18588,#18589,#18590,#18591,#18592,#18593,#18594,#18595,#18596,
#18597,#18598,#18599,#18600,#18601,#18602,#18603,#18604,#18605,#18606,#18607,
#18608,#18609,#18610,#18611,#18612,#18613,#18614,#18615,#18616,#18617,#18618,
#18619,#18620,#18621,#18622,#18623,#18624,#18625,#18626,#18627,#18628,#18629,
#18630,#18631,#18632,#18633,#18634,#18635,#18636,#18637,#18638,#18639,#18640,
#18641,#18642,#18643,#18644,#18645,#18646,#18647,#18648,#18649,#18650,#18651,
#18652,#18653,#18654,#18655,#18656,#18657,#18658,#18659,#18660,#18661,#18662,
#18663,#18664,#18665,#18666,#18667,#18668,#18669,#18670,#18671,#18672,#18673,
#18674,#18675,#18676,#18677,#18678,#18679,#18680,#18681,#18682,#18683,#18684,
#18685,#18686,#18687,#18688,#18689,#18690,#18691,#18692,#18693,#18694,#18695,
#18696,#18697,#18698,#18699,#18700,#18701,#18702,#18703,#18704,#18705,#18706,
#18707,#18708,#18709,#18710,#18711,#18712,#18713,#18714,#18715,#18716,#18717,
#18718,#18719,#18720,#18721,#18722,#18723,#18724,#18725,#18726,#18727,#18728,
#18729,#18730,#18731,#18732,#18733,#18734,#18735,#18736,#18737,#18738,#18739,
#18740,#18741,#18742,#18743,#18744,#18745,#18746,#18747,#18748,#18749,#18750,
#18751,#18752,#18753,#18754,#18755,#18756,#18757,#18758,#18759,#18760,#18761,
#18762,#18763,#18764,#18765,#18766,#18767,#18768,#18769,#18770,#18771,#18772,
#18773,#18774,#18775,#18776,#18777,#18778,#18779,#18780,#18781,#18782,#18783,
#18784,#18785,#18786,#18787,#18788,#18789,#18790,#18791,#18792,#18793,#18794,
#18795,#18796,#18797,#18798,#18799,#18800,#18801,#18802,#18803,#18804,#18805,
#18806,#18807,#18808,#18809,#18810,#18811,#18812,#18813,#18814,#18815,#18816,
#18817,#18818,#18819,#18820,#18821,#18822,#18823,#18824,#18825,#18826,#18827,
#18828,#18829,#18830,#18831,#18832,#18833,#18834,#18835,#18836,#18837,#18838,
#18839,#18840,#18841,#18842,#18843,#18844,#18845,#18846,#18847,#18848,#18849,
#18850,#18851,#18852,#18853,#18854,#18855,#18856,#18857,#18858,#18859,#18860,
#18861,#18862,#18863,#18864,#18865,#18866,#18867,#18868,#18869,#18870,#18871,
#18872,#18873,#18874,#18875,#18876,#18877,#18878,#18879,#18880,#18881,#18882,
#18883,#18884,#18885,#18886,#18887,#18888,#18889,#18890,#18891,#18892,#18893,
#18894,#18895,#18896,#18897,#18898,#18899,#18900,#18901,#18902,#18903,#18904,
#18905,#18906,#18907,#18908,#18909,#18910,#18911,#18912,#18913,#18914,#18915,
#18916,#18917,#18918,#18919,#18920,#18921,#18922,#18923,#18924,#18925,#18926,
#18927,#18928,#18929,#18930,#18931,#18932,#18933,#18934,#18935,#18936,#18937,
#18938,#18939,#18940,#18941,#18942,#18943,#18944,#18945,#18946,#18947,#18948,
#18949,#18950,#18951,#18952,#18953,#18954,#18955,#18956,#18957,#18958,#18959,
#18960,#18961,#18962,#18963,#18964,#18965,#18966,#18967,#18968,#18969,#18970,
#18971,#18972,#18973,#18974,#18975,#18976,#18977,#18978,#18979,#18980,#18981,
#18982,#18983,#18984,#18985,#18986,#18987,#18988,#18989,#18990,#18991,#18992,
#18993,#18994,#18995,#18996,#18997,#18998,#18999,#19000,#19001,#19002,#19003,
#19004,#19005,#19006,#19007,#19008,#19009,#19010,#19011,#19012,#19013,#19014,
#19015,#19016,#19017,#19018,#19019,#19020,#19021,#19022,#19023,#19024,#19025,
#19026,#19027,#19028,#19029,#19030,#19031,#19032,#19033,#19034,#19035,#19036,
#19037,#19038,#19039,#19040,#19041,#19042,#19043,#19044,#19045,#19046,#19047,
#19048,#19049,#19050,#19051,#19052,#19053,#19054,#19055,#19056,#19057,#19058,
#19059,#19060,#19061,#19062,#19063,#19064,#19065,#19066,#19067,#19068,#19069,
#19070,#19071,#19072,#19073,#19074,#19075,#19076,#19077,#19078,#19079,#19080,
#19081,#19082,#19083,#19084,#19085,#19086,#19087,#19088,#19089,#19090,#19091,
#19092,#19093,#19094,#19095,#19096,#19097,#19098,#19099,#19100,#19101,#19102,
#19103,#19104,#19105,#19106,#19107,#19108,#19109,#19110,#19111,#19112,#19113,
#19114,#19115,#19116,#19117,#19118,#19119,#19120,#19121,#19122,#19123,#19124,
#19125,#19126,#19127,#19128,#19129,#19130,#19131,#19132,#19133,#19134,#19135,
#19136,#19137,#19138,#19139,#19140,#19141,#19142,#19143,#19144,#19145,#19146,
#19147,#19148,#19149,#19150,#19151,#19152,#19153,#19154,#19155,#19156,#19157,
#19158,#19159,#19160,#19161,#19162,#19163,#19164,#19165,#19166,#19167,#19168,
#19169,#19170,#19171,#19172,#19173,#19174,#19175,#19176,#19177,#19178,#19179,
#19180,#19181,#19182,#19183,#19184,#19185,#19186,#19187,#19188,#19189,#19190,
#19191,#19192,#19193,#19194,#19195,#19196,#19197,#19198,#19199,#19200,#19201,
#19202,#19203,#19204,#19205,#19206,#19207,#19208,#19209,#19210,#19211,#19212,
#19213,#19214,#19215,#19216,#19217,#19218,#19219,#19220,#19221,#19222,#19223,
#19224,#19225,#19226,#19227,#19228,#19229,#19230,#19231,#19232,#19233,#19234,
#19235,#19236,#19237,#19238,#19239,#19240,#19241,#19242,#19243,#19244,#19245,
#19246,#19247,#19248,#19249,#19250,#19251,#19252,#19253,#19254,#19255,#19256,
#19257,#19258,#19259,#19260,#19261,#19262,#19263,#19264,#19265,#19266,#19267,
#19268,#19269,#19270,#19271,#19272,#19273,#19274,#19275,#19276,#19277,#19278,
#19279,#19280,#19281,#19282,#19283,#19284,#19285,#19286,#19287,#19288,#19289,
#19290,#19291,#19292,#19293,#19294,#19295,#19296,#19297,#19298,#19299,#19300,
#19301,#19302,#19303,#19304,#19305,#19306,#19307,#19308,#19309,#19310,#19311,
#19312,#19313,#19314,#19315,#19316,#19317,#19318,#19319,#19320,#19321,#19322,
#19323,#19324,#19325,#19326,#19327,#19328,#19329,#19330,#19331,#19332,#19333,
#19334,#19335,#19336,#19337,#19338,#19339,#19340,#19341,#19342,#19343,#19344,
#19345,#19346,#19347,#19348,#19349,#19350,#19351,#19352,#19353,#19354,#19355,
#19356,#19357,#19358,#19359,#19360,#19361,#19362,#19363,#19364,#19365,#19366,
#19367,#19368,#19369,#19370,#19371,#19372,#19373,#19374,#19375,#19376,#19377,
#19378,#19379,#19380,#19381,#19382,#19383,#19384,#19385,#19386,#19387,#19388,
#19389,#19390,#19391,#19392,#19393,#19394,#19395,#19396,#19397,#19398,#19399,
#19400,#19401,#19402,#19403,#19404,#19405,#19406,#19407,#19408,#19409,#19410,
#19411,#19412,#19413,#19414,#19415,#19416,#19417,#19418,#19419,#19420,#19421,
#19422,#19423,#19424,#19425,#19426,#19427,#19428,#19429,#19430,#19431,#19432,
#19433,#19434,#19435,#19436,#19437,#19438)),.UNSPECIFIED.,.F.,.F.,.F.)
B_SPLINE_SURFACE_WITH_KNOTS((4,4),(3,2,2,2,2,2,2,2,2,2,2,2,2,2,2,2,2,2,
2,2,2,2,2,2,2,2,2,2,2,2,2,2,2,2,2,2,2,2,2,2,2,2,2,2,2,2,2,2,2,2,2,2,2,2,
2,2,2,2,2,2,2,2,2,2,2,2,2,2,2,2,2,2,2,2,2,2,2,2,2,2,2,2,2,2,2,2,2,2,2,2,
2,2,2,2,2,2,2,2,2,2,2,2,2,2,2,2,2,2,2,2,2,2,2,2,2,2,2,2,2,2,2,2,2,2,2,2,
2,2,2,2,2,2,2,2,2,2,2,2,2,2,2,2,2,2,2,2,2,2,2,2,2,2,2,2,2,2,2,2,2,2,2,2,
2,2,2,2,2,2,2,2,2,2,2,2,2,2,2,2,2,2,2,2,2,2,2,2,2,2,2,2,2,2,2,2,2,2,2,2,
2,2,2,2,2,2,2,2,2,2,2,2,2,2,2,2,2,2,2,2,2,2,2,2,2,2,2,2,2,2,2,2,2,2,2,2,
2,2,2,2,2,2,2,2,2,2,2,2,2,2,2,2,2,2,2,2,2,2,2,2,2,2,2,2,2,2,2,2,2,2,2,2,
2,2,2,2,2,2,2,2,2,2,2,2,2,2,2,2,2,2,2,2,2,2,2,2,2,2,2,2,2,2,2,2,2,2,2,2,
2,2,2,2,2,2,2,2,2,2,2,2,2,2,2,2,2,2,2,2,2,2,2,2,2,2,2,2,2,2,2,2,2,2,2,2,
2,2,2,2,2,2,2,2,2,2,2,2,2,2,2,2,2,2,2,2,2,2,2,2,2,2,2,2,2,2,2,2,2,2,2,2,
2,2,2,2,2,2,2,2,2,2,2,2,2,2,2,2,2,2,2,2,2,2,2,2,2,2,2,2,2,2,2,2,2,2,2,2,
2,2,2,2,2,2,2,2,2,2,2,2,2,2,2,2,2,2,2,2,2,2,2,2,2,2,2,2,2,2,2,2,2,2,2,2,
2,2,2,2,2,2,2,2,2,2,2,2,2,2,2,2,2,2,2,2,2,2,2,2,2,2,2,2,2,2,2,2,2,2,2,2,
3),(0.,1.),(0.,0.00205761316872428,0.00411522633744856,0.00617283950617284,
0.00823045267489712,0.0102880658436214,0.0123456790123457,0.01440329218107,
0.0164609053497942,0.0185185185185185,0.0205761316872428,0.0226337448559671,
0.0246913580246914,0.0267489711934156,0.0288065843621399,0.0308641975308642,
0.0329218106995885,0.0349794238683128,0.037037037037037,0.0390946502057613,
0.0411522633744856,0.0432098765432099,0.0452674897119342,0.0473251028806584,
0.0493827160493827,0.051440329218107,0.0534979423868313,0.0555555555555556,
0.0576131687242798,0.0596707818930041,0.0617283950617284,0.0637860082304527,
0.065843621399177,0.0679012345679012,0.0699588477366255,0.0720164609053498,
0.0740740740740741,0.0761316872427984,0.0781893004115226,0.0802469135802469,
0.0823045267489712,0.0843621399176955,0.0864197530864197,0.088477366255144,
0.0905349794238683,0.0925925925925926,0.0946502057613169,0.0967078189300412,
0.0987654320987654,0.10082304526749,0.102880658436214,0.104938271604938,
0.106995884773663,0.109053497942387,0.111111111111111,0.113168724279835,
0.11522633744856,0.117283950617284,0.119341563786008,0.121399176954733,
0.123456790123457,0.125514403292181,0.127572016460905,0.12962962962963,
0.131687242798354,0.133744855967078,0.135802469135802,0.137860082304527,
0.139917695473251,0.141975308641975,0.1440329218107,0.146090534979424,0.148148148148148,
0.150205761316872,0.152263374485597,0.154320987654321,0.156378600823045,
0.15843621399177,0.160493827160494,0.162551440329218,0.164609053497942,
0.166666666666667,0.168724279835391,0.170781893004115,0.172839506172839,
0.174897119341564,0.176954732510288,0.179012345679012,0.181069958847737,
0.183127572016461,0.185185185185185,0.187242798353909,0.189300411522634,
0.191358024691358,0.193415637860082,0.195473251028807,0.197530864197531,
0.199588477366255,0.201646090534979,0.203703703703704,0.205761316872428,
0.207818930041152,0.209876543209877,0.211934156378601,0.213991769547325,
0.216049382716049,0.218106995884774,0.220164609053498,0.222222222222222,
0.224279835390947,0.226337448559671,0.228395061728395,0.230452674897119,
0.232510288065844,0.234567901234568,0.236625514403292,0.238683127572016,
0.240740740740741,0.242798353909465,0.244855967078189,0.246913580246914,
0.248971193415638,0.251028806584362,0.253086419753086,0.255144032921811,
0.257201646090535,0.259259259259259,0.261316872427984,0.263374485596708,
0.265432098765432,0.267489711934156,0.269547325102881,0.271604938271605,
0.273662551440329,0.275720164609054,0.277777777777778,0.279835390946502,
0.281893004115226,0.283950617283951,0.286008230452675,0.288065843621399,
0.290123456790123,0.292181069958848,0.294238683127572,0.296296296296296,
0.298353909465021,0.300411522633745,0.302469135802469,0.304526748971193,
0.306584362139918,0.308641975308642,0.310699588477366,0.312757201646091,
0.314814814814815,0.316872427983539,0.318930041152263,0.320987654320988,
0.323045267489712,0.325102880658436,0.327160493827161,0.329218106995885,
0.331275720164609,0.333333333333333,0.335390946502058,0.337448559670782,
0.339506172839506,0.34156378600823,0.343621399176955,0.345679012345679,
0.347736625514403,0.349794238683128,0.351851851851852,0.353909465020576,
0.3559670781893,0.358024691358025,0.360082304526749,0.362139917695473,0.364197530864198,
0.366255144032922,0.368312757201646,0.37037037037037,0.372427983539095,
0.374485596707819,0.376543209876543,0.378600823045267,0.380658436213992,
0.382716049382716,0.38477366255144,0.386831275720165,0.388888888888889,
0.390946502057613,0.393004115226337,0.395061728395062,0.397119341563786,
0.39917695473251,0.401234567901235,0.403292181069959,0.405349794238683,
0.407407407407407,0.409465020576132,0.411522633744856,0.41358024691358,
0.415637860082305,0.417695473251029,0.419753086419753,0.421810699588477,
0.423868312757202,0.425925925925926,0.42798353909465,0.430041152263374,
0.432098765432099,0.434156378600823,0.436213991769547,0.438271604938272,
0.440329218106996,0.44238683127572,0.444444444444444,0.446502057613169,
0.448559670781893,0.450617283950617,0.452674897119342,0.454732510288066,
0.45679012345679,0.458847736625514,0.460905349794239,0.462962962962963,
0.465020576131687,0.467078189300412,0.469135802469136,0.47119341563786,
0.473251028806584,0.475308641975309,0.477366255144033,0.479423868312757,
0.481481481481481,0.483539094650206,0.48559670781893,0.487654320987654,
0.489711934156379,0.491769547325103,0.493827160493827,0.495884773662551,
0.497942386831276,0.5,0.502057613168724,0.504115226337449,0.506172839506173,
0.508230452674897,0.510288065843621,0.512345679012346,0.51440329218107,
0.516460905349794,0.518518518518518,0.520576131687243,0.522633744855967,
0.524691358024691,0.526748971193416,0.52880658436214,0.530864197530864,
0.532921810699588,0.534979423868313,0.537037037037037,0.539094650205761,
0.541152263374486,0.54320987654321,0.545267489711934,0.547325102880658,
0.549382716049383,0.551440329218107,0.553497942386831,0.555555555555556,
0.55761316872428,0.559670781893004,0.561728395061728,0.563786008230453,
0.565843621399177,0.567901234567901,0.569958847736626,0.57201646090535,
0.574074074074074,0.576131687242798,0.578189300411523,0.580246913580247,
0.582304526748971,0.584362139917695,0.58641975308642,0.588477366255144,
0.590534979423868,0.592592592592593,0.594650205761317,0.596707818930041,
0.598765432098765,0.60082304526749,0.602880658436214,0.604938271604938,
0.606995884773663,0.609053497942387,0.611111111111111,0.613168724279835,
0.61522633744856,0.617283950617284,0.619341563786008,0.621399176954732,
0.623456790123457,0.625514403292181,0.627572016460905,0.62962962962963,
0.631687242798354,0.633744855967078,0.635802469135803,0.637860082304527,
0.639917695473251,0.641975308641975,0.6440329218107,0.646090534979424,0.648148148148148,
0.650205761316872,0.652263374485597,0.654320987654321,0.656378600823045,
0.65843621399177,0.660493827160494,0.662551440329218,0.664609053497942,
0.666666666666667,0.668724279835391,0.670781893004115,0.672839506172839,
0.674897119341564,0.676954732510288,0.679012345679012,0.681069958847737,
0.683127572016461,0.685185185185185,0.687242798353909,0.689300411522634,
0.691358024691358,0.693415637860082,0.695473251028807,0.697530864197531,
0.699588477366255,0.701646090534979,0.703703703703704,0.705761316872428,
0.707818930041152,0.709876543209877,0.711934156378601,0.713991769547325,
0.716049382716049,0.718106995884774,0.720164609053498,0.722222222222222,
0.724279835390947,0.726337448559671,0.728395061728395,0.730452674897119,
0.732510288065844,0.734567901234568,0.736625514403292,0.738683127572016,
0.740740740740741,0.742798353909465,0.744855967078189,0.746913580246914,
0.748971193415638,0.751028806584362,0.753086419753086,0.755144032921811,
0.757201646090535,0.759259259259259,0.761316872427984,0.763374485596708,
0.765432098765432,0.767489711934156,0.769547325102881,0.771604938271605,
0.773662551440329,0.775720164609053,0.777777777777778,0.779835390946502,
0.781893004115226,0.783950617283951,0.786008230452675,0.788065843621399,
0.790123456790123,0.792181069958848,0.794238683127572,0.796296296296296,
0.798353909465021,0.800411522633745,0.802469135802469,0.804526748971193,
0.806584362139918,0.808641975308642,0.810699588477366,0.812757201646091,
0.814814814814815,0.816872427983539,0.818930041152263,0.820987654320988,
0.823045267489712,0.825102880658436,0.827160493827161,0.829218106995885,
0.831275720164609,0.833333333333333,0.835390946502058,0.837448559670782,
0.839506172839506,0.84156378600823,0.843621399176955,0.845679012345679,
0.847736625514403,0.849794238683128,0.851851851851852,0.853909465020576,
0.8559670781893,0.858024691358025,0.860082304526749,0.862139917695473,0.864197530864197,
0.866255144032922,0.868312757201646,0.87037037037037,0.872427983539095,
0.874485596707819,0.876543209876543,0.878600823045268,0.880658436213992,
0.882716049382716,0.88477366255144,0.886831275720165,0.888888888888889,
0.890946502057613,0.893004115226337,0.895061728395062,0.897119341563786,
0.89917695473251,0.901234567901235,0.903292181069959,0.905349794238683,
0.907407407407407,0.909465020576132,0.911522633744856,0.91358024691358,
0.915637860082305,0.917695473251029,0.919753086419753,0.921810699588477,
0.923868312757202,0.925925925925926,0.92798353909465,0.930041152263374,
0.932098765432099,0.934156378600823,0.936213991769547,0.938271604938272,
0.940329218106996,0.94238683127572,0.944444444444444,0.946502057613169,
0.948559670781893,0.950617283950617,0.952674897119342,0.954732510288066,
0.95679012345679,0.958847736625514,0.960905349794239,0.962962962962963,
0.965020576131687,0.967078189300412,0.969135802469136,0.97119341563786,
0.973251028806584,0.975308641975309,0.977366255144033,0.979423868312757,
0.981481481481482,0.983539094650206,0.98559670781893,0.987654320987654,
0.989711934156379,0.991769547325103,0.993827160493827,0.995884773662551,
0.997942386831276,1.),.UNSPECIFIED.)
GEOMETRIC_REPRESENTATION_ITEM()
RATIONAL_B_SPLINE_SURFACE(((1.,0.866025403784439,1.,0.866025403784439,1.,
0.866025403784439,1.,0.866025403784439,1.,0.866025403784439,1.,0.866025403784439,
1.,0.866025403784439,1.,0.866025403784439,1.,0.866025403784439,1.,0.866025403784439,
1.,0.866025403784439,1.,0.866025403784439,1.,0.866025403784439,1.,0.866025403784439,
1.,0.866025403784439,1.,0.866025403784439,1.,0.866025403784439,1.,0.866025403784439,
1.,0.866025403784439,1.,0.866025403784439,1.,0.866025403784439,1.,0.866025403784439,
1.,0.866025403784439,1.,0.866025403784439,1.,0.866025403784439,1.,0.866025403784439,
1.,0.866025403784439,1.,0.866025403784439,1.,0.866025403784439,1.,0.866025403784439,
1.,0.866025403784439,1.,0.866025403784439,1.,0.866025403784439,1.,0.866025403784439,
1.,0.866025403784439,1.,0.866025403784439,1.,0.866025403784439,1.,0.866025403784439,
1.,0.866025403784439,1.,0.866025403784439,1.,0.866025403784439,1.,0.866025403784439,
1.,0.866025403784439,1.,0.866025403784439,1.,0.866025403784439,1.,0.866025403784439,
1.,0.866025403784439,1.,0.866025403784439,1.,0.866025403784439,1.,0.866025403784439,
1.,0.866025403784439,1.,0.866025403784439,1.,0.866025403784439,1.,0.866025403784439,
1.,0.866025403784439,1.,0.866025403784439,1.,0.866025403784439,1.,0.866025403784439,
1.,0.866025403784439,1.,0.866025403784439,1.,0.866025403784439,1.,0.866025403784439,
1.,0.866025403784439,1.,0.866025403784439,1.,0.866025403784439,1.,0.866025403784439,
1.,0.866025403784439,1.,0.866025403784439,1.,0.866025403784439,1.,0.866025403784439,
1.,0.866025403784439,1.,0.866025403784439,1.,0.866025403784439,1.,0.866025403784439,
1.,0.866025403784439,1.,0.866025403784439,1.,0.866025403784439,1.,0.866025403784439,
1.,0.866025403784439,1.,0.866025403784439,1.,0.866025403784439,1.,0.866025403784439,
1.,0.866025403784439,1.,0.866025403784439,1.,0.866025403784439,1.,0.866025403784439,
1.,0.866025403784439,1.,0.866025403784439,1.,0.866025403784439,1.,0.866025403784439,
1.,0.866025403784439,1.,0.866025403784439,1.,0.866025403784439,1.,0.866025403784439,
1.,0.866025403784439,1.,0.866025403784439,1.,0.866025403784439,1.,0.866025403784439,
1.,0.866025403784439,1.,0.866025403784439,1.,0.866025403784439,1.,0.866025403784439,
1.,0.866025403784439,1.,0.866025403784439,1.,0.866025403784439,1.,0.866025403784439,
1.,0.866025403784439,1.,0.866025403784439,1.,0.866025403784439,1.,0.866025403784439,
1.,0.866025403784439,1.,0.866025403784439,1.,0.866025403784439,1.,0.866025403784439,
1.,0.866025403784439,1.,0.866025403784439,1.,0.866025403784439,1.,0.866025403784439,
1.,0.866025403784439,1.,0.866025403784439,1.,0.866025403784439,1.,0.866025403784439,
1.,0.866025403784439,1.,0.866025403784439,1.,0.866025403784439,1.,0.866025403784439,
1.,0.866025403784439,1.,0.866025403784439,1.,0.866025403784439,1.,0.866025403784439,
1.,0.866025403784439,1.,0.866025403784439,1.,0.866025403784439,1.,0.866025403784439,
1.,0.866025403784439,1.,0.866025403784439,1.,0.866025403784439,1.,0.866025403784439,
1.,0.866025403784439,1.,0.866025403784439,1.,0.866025403784439,1.,0.866025403784439,
1.,0.866025403784439,1.,0.866025403784439,1.,0.866025403784439,1.,0.866025403784439,
1.,0.866025403784439,1.,0.866025403784439,1.,0.866025403784439,1.,0.866025403784439,
1.,0.866025403784439,1.,0.866025403784439,1.,0.866025403784439,1.,0.866025403784439,
1.,0.866025403784439,1.,0.866025403784439,1.,0.866025403784439,1.,0.866025403784439,
1.,0.866025403784439,1.,0.866025403784439,1.,0.866025403784439,1.,0.866025403784439,
1.,0.866025403784439,1.,0.866025403784439,1.,0.866025403784439,1.,0.866025403784439,
1.,0.866025403784439,1.,0.866025403784439,1.,0.866025403784439,1.,0.866025403784439,
1.,0.866025403784439,1.,0.866025403784439,1.,0.866025403784439,1.,0.866025403784439,
1.,0.866025403784439,1.,0.866025403784439,1.,0.866025403784439,1.,0.866025403784439,
1.,0.866025403784439,1.,0.866025403784439,1.,0.866025403784439,1.,0.866025403784439,
1.,0.866025403784439,1.,0.866025403784439,1.,0.866025403784439,1.,0.866025403784439,
1.,0.866025403784439,1.,0.866025403784439,1.,0.866025403784439,1.,0.866025403784439,
1.,0.866025403784439,1.,0.866025403784439,1.,0.866025403784439,1.,0.866025403784439,
1.,0.866025403784439,1.,0.866025403784439,1.,0.866025403784439,1.,0.866025403784439,
1.,0.866025403784439,1.,0.866025403784439,1.,0.866025403784439,1.,0.866025403784439,
1.,0.866025403784439,1.,0.866025403784439,1.,0.866025403784439,1.,0.866025403784439,
1.,0.866025403784439,1.,0.866025403784439,1.,0.866025403784439,1.,0.866025403784439,
1.,0.866025403784439,1.,0.866025403784439,1.,0.866025403784439,1.,0.866025403784439,
1.,0.866025403784439,1.,0.866025403784439,1.,0.866025403784439,1.,0.866025403784439,
1.,0.866025403784439,1.,0.866025403784439,1.,0.866025403784439,1.,0.866025403784439,
1.,0.866025403784439,1.,0.866025403784439,1.,0.866025403784439,1.,0.866025403784439,
1.,0.866025403784439,1.,0.866025403784439,1.,0.866025403784439,1.,0.866025403784439,
1.,0.866025403784439,1.,0.866025403784439,1.,0.866025403784439,1.,0.866025403784439,
1.,0.866025403784439,1.,0.866025403784439,1.,0.866025403784439,1.,0.866025403784439,
1.,0.866025403784439,1.,0.866025403784439,1.,0.866025403784439,1.,0.866025403784439,
1.,0.866025403784439,1.,0.866025403784439,1.,0.866025403784439,1.,0.866025403784439,
1.,0.866025403784439,1.,0.866025403784439,1.,0.866025403784439,1.,0.866025403784439,
1.,0.866025403784439,1.,0.866025403784439,1.,0.866025403784439,1.,0.866025403784439,
1.,0.866025403784439,1.,0.866025403784439,1.,0.866025403784439,1.,0.866025403784439,
1.,0.866025403784439,1.,0.866025403784439,1.,0.866025403784439,1.,0.866025403784439,
1.,0.866025403784439,1.,0.866025403784439,1.,0.866025403784439,1.,0.866025403784439,
1.,0.866025403784439,1.,0.866025403784439,1.,0.866025403784439,1.,0.866025403784439,
1.,0.866025403784439,1.,0.866025403784439,1.,0.866025403784439,1.,0.866025403784439,
1.,0.866025403784439,1.,0.866025403784439,1.,0.866025403784439,1.,0.866025403784439,
1.,0.866025403784439,1.,0.866025403784439,1.,0.866025403784439,1.,0.866025403784439,
1.,0.866025403784439,1.,0.866025403784439,1.,0.866025403784439,1.,0.866025403784439,
1.,0.866025403784439,1.,0.866025403784439,1.,0.866025403784439,1.,0.866025403784439,
1.,0.866025403784439,1.,0.866025403784439,1.,0.866025403784439,1.,0.866025403784439,
1.,0.866025403784439,1.,0.866025403784439,1.,0.866025403784439,1.,0.866025403784439,
1.,0.866025403784439,1.,0.866025403784439,1.,0.866025403784439,1.,0.866025403784439,
1.,0.866025403784439,1.,0.866025403784439,1.,0.866025403784439,1.,0.866025403784439,
1.,0.866025403784439,1.,0.866025403784439,1.,0.866025403784439,1.,0.866025403784439,
1.,0.866025403784439,1.,0.866025403784439,1.,0.866025403784439,1.,0.866025403784439,
1.,0.866025403784439,1.,0.866025403784439,1.,0.866025403784439,1.,0.866025403784439,
1.,0.866025403784439,1.,0.866025403784439,1.,0.866025403784439,1.,0.866025403784439,
1.,0.866025403784439,1.,0.866025403784439,1.,0.866025403784439,1.,0.866025403784439,
1.,0.866025403784439,1.,0.866025403784439,1.,0.866025403784439,1.,0.866025403784439,
1.,0.866025403784439,1.,0.866025403784439,1.,0.866025403784439,1.,0.866025403784439,
1.,0.866025403784439,1.,0.866025403784439,1.,0.866025403784439,1.,0.866025403784439,
1.,0.866025403784439,1.,0.866025403784439,1.,0.866025403784439,1.,0.866025403784439,
1.,0.866025403784439,1.,0.866025403784439,1.,0.866025403784439,1.,0.866025403784439,
1.,0.866025403784439,1.,0.866025403784439,1.,0.866025403784439,1.,0.866025403784439,
1.,0.866025403784439,1.,0.866025403784439,1.,0.866025403784439,1.,0.866025403784439,
1.,0.866025403784439,1.,0.866025403784439,1.,0.866025403784439,1.,0.866025403784439,
1.,0.866025403784439,1.,0.866025403784439,1.,0.866025403784439,1.,0.866025403784439,
1.,0.866025403784439,1.,0.866025403784439,1.,0.866025403784439,1.,0.866025403784439,
1.,0.866025403784439,1.,0.866025403784439,1.,0.866025403784439,1.,0.866025403784439,
1.,0.866025403784439,1.,0.866025403784439,1.,0.866025403784439,1.,0.866025403784439,
1.,0.866025403784439,1.,0.866025403784439,1.,0.866025403784439,1.,0.866025403784439,
1.,0.866025403784439,1.,0.866025403784439,1.,0.866025403784439,1.,0.866025403784439,
1.,0.866025403784439,1.,0.866025403784439,1.,0.866025403784439,1.,0.866025403784439,
1.,0.866025403784439,1.,0.866025403784439,1.,0.866025403784439,1.,0.866025403784439,
1.,0.866025403784439,1.,0.866025403784439,1.,0.866025403784439,1.,0.866025403784439,
1.,0.866025403784439,1.,0.866025403784439,1.,0.866025403784439,1.,0.866025403784439,
1.,0.866025403784439,1.,0.866025403784439,1.,0.866025403784439,1.,0.866025403784439,
1.,0.866025403784439,1.,0.866025403784439,1.,0.866025403784439,1.,0.866025403784439,
1.,0.866025403784439,1.,0.866025403784439,1.,0.866025403784439,1.,0.866025403784439,
1.,0.866025403784439,1.,0.866025403784439,1.,0.866025403784439,1.,0.866025403784439,
1.,0.866025403784439,1.,0.866025403784439,1.,0.866025403784439,1.,0.866025403784439,
1.,0.866025403784439,1.,0.866025403784439,1.,0.866025403784439,1.,0.866025403784439,
1.,0.866025403784439,1.,0.866025403784439,1.,0.866025403784439,1.,0.866025403784439,
1.,0.866025403784439,1.,0.866025403784439,1.,0.866025403784439,1.,0.866025403784439,
1.,0.866025403784439,1.,0.866025403784439,1.,0.866025403784439,1.,0.866025403784439,
1.,0.866025403784439,1.,0.866025403784439,1.,0.866025403784439,1.,0.866025403784439,
1.,0.866025403784439,1.,0.866025403784439,1.,0.866025403784439,1.,0.866025403784439,
1.,0.866025403784439,1.,0.866025403784439,1.,0.866025403784439,1.,0.866025403784439,
1.,0.866025403784439,1.,0.866025403784439,1.,0.866025403784439,1.,0.866025403784439,
1.,0.866025403784439,1.,0.866025403784439,1.,0.866025403784439,1.,0.866025403784439,
1.,0.866025403784439,1.,0.866025403784439,1.,0.866025403784439,1.,0.866025403784439,
1.,0.866025403784439,1.,0.866025403784439,1.,0.866025403784439,1.,0.866025403784439,
1.,0.866025403784439,1.,0.866025403784439,1.,0.866025403784439,1.,0.866025403784439,
1.,0.866025403784439,1.,0.866025403784439,1.,0.866025403784439,1.,0.866025403784439,
1.,0.866025403784439,1.,0.866025403784439,1.,0.866025403784439,1.,0.866025403784439,
1.,0.866025403784439,1.,0.866025403784439,1.,0.866025403784439,1.,0.866025403784439,
1.,0.866025403784439,1.,0.866025403784439,1.,0.866025403784439,1.,0.866025403784439,
1.,0.866025403784439,1.,0.866025403784439,1.,0.866025403784439,1.,0.866025403784439,
1.),(0.641165742156689,0.555265820743996,0.641165742156689,0.555265820743996,
0.641165742156689,0.555265820743996,0.641165742156689,0.555265820743996,
0.641165742156689,0.555265820743996,0.641165742156689,0.555265820743996,
0.641165742156689,0.555265820743996,0.641165742156689,0.555265820743996,
0.641165742156689,0.555265820743996,0.641165742156689,0.555265820743996,
0.641165742156689,0.555265820743996,0.641165742156689,0.555265820743996,
0.641165742156689,0.555265820743996,0.641165742156689,0.555265820743996,
0.641165742156689,0.555265820743996,0.641165742156689,0.555265820743996,
0.641165742156689,0.555265820743996,0.641165742156689,0.555265820743996,
0.641165742156689,0.555265820743996,0.641165742156689,0.555265820743996,
0.641165742156689,0.555265820743996,0.641165742156689,0.555265820743996,
0.641165742156689,0.555265820743996,0.641165742156689,0.555265820743996,
0.641165742156689,0.555265820743996,0.641165742156689,0.555265820743996,
0.641165742156689,0.555265820743996,0.641165742156689,0.555265820743996,
0.641165742156689,0.555265820743996,0.641165742156689,0.555265820743996,
0.641165742156689,0.555265820743996,0.641165742156689,0.555265820743996,
0.641165742156689,0.555265820743996,0.641165742156689,0.555265820743996,
0.641165742156689,0.555265820743996,0.641165742156689,0.555265820743996,
0.641165742156689,0.555265820743996,0.641165742156689,0.555265820743996,
0.641165742156689,0.555265820743996,0.641165742156689,0.555265820743996,
0.641165742156689,0.555265820743996,0.641165742156689,0.555265820743996,
0.641165742156689,0.555265820743996,0.641165742156689,0.555265820743996,
0.641165742156689,0.555265820743996,0.641165742156689,0.555265820743996,
0.641165742156689,0.555265820743996,0.641165742156689,0.555265820743996,
0.641165742156689,0.555265820743996,0.641165742156689,0.555265820743996,
0.641165742156689,0.555265820743996,0.641165742156689,0.555265820743996,
0.641165742156689,0.555265820743996,0.641165742156689,0.555265820743996,
0.641165742156689,0.555265820743996,0.641165742156689,0.555265820743996,
0.641165742156689,0.555265820743996,0.641165742156689,0.555265820743996,
0.641165742156689,0.555265820743996,0.641165742156689,0.555265820743996,
0.641165742156689,0.555265820743996,0.641165742156689,0.555265820743996,
0.641165742156689,0.555265820743996,0.641165742156689,0.555265820743996,
0.641165742156689,0.555265820743996,0.641165742156689,0.555265820743996,
0.641165742156689,0.555265820743996,0.641165742156689,0.555265820743996,
0.641165742156689,0.555265820743996,0.641165742156689,0.555265820743996,
0.641165742156689,0.555265820743996,0.641165742156689,0.555265820743996,
0.641165742156689,0.555265820743996,0.641165742156689,0.555265820743996,
0.641165742156689,0.555265820743996,0.641165742156689,0.555265820743996,
0.641165742156689,0.555265820743996,0.641165742156689,0.555265820743996,
0.641165742156689,0.555265820743996,0.641165742156689,0.555265820743996,
0.641165742156689,0.555265820743996,0.641165742156689,0.555265820743996,
0.641165742156689,0.555265820743996,0.641165742156689,0.555265820743996,
0.641165742156689,0.555265820743996,0.641165742156689,0.555265820743996,
0.641165742156689,0.555265820743996,0.641165742156689,0.555265820743996,
0.641165742156689,0.555265820743996,0.641165742156689,0.555265820743996,
0.641165742156689,0.555265820743996,0.641165742156689,0.555265820743996,
0.641165742156689,0.555265820743996,0.641165742156689,0.555265820743996,
0.641165742156689,0.555265820743996,0.641165742156689,0.555265820743996,
0.641165742156689,0.555265820743996,0.641165742156689,0.555265820743996,
0.641165742156689,0.555265820743996,0.641165742156689,0.555265820743996,
0.641165742156689,0.555265820743996,0.641165742156689,0.555265820743996,
0.641165742156689,0.555265820743996,0.641165742156689,0.555265820743996,
0.641165742156689,0.555265820743996,0.641165742156689,0.555265820743996,
0.641165742156689,0.555265820743996,0.641165742156689,0.555265820743996,
0.641165742156689,0.555265820743996,0.641165742156689,0.555265820743996,
0.641165742156689,0.555265820743996,0.641165742156689,0.555265820743996,
0.641165742156689,0.555265820743996,0.641165742156689,0.555265820743996,
0.641165742156689,0.555265820743996,0.641165742156689,0.555265820743996,
0.641165742156689,0.555265820743996,0.641165742156689,0.555265820743996,
0.641165742156689,0.555265820743996,0.641165742156689,0.555265820743996,
0.641165742156689,0.555265820743996,0.641165742156689,0.555265820743996,
0.641165742156689,0.555265820743996,0.641165742156689,0.555265820743996,
0.641165742156689,0.555265820743996,0.641165742156689,0.555265820743996,
0.641165742156689,0.555265820743996,0.641165742156689,0.555265820743996,
0.641165742156689,0.555265820743996,0.641165742156689,0.555265820743996,
0.641165742156689,0.555265820743996,0.641165742156689,0.555265820743996,
0.641165742156689,0.555265820743996,0.641165742156689,0.555265820743996,
0.641165742156689,0.555265820743996,0.641165742156689,0.555265820743996,
0.641165742156689,0.555265820743996,0.641165742156689,0.555265820743996,
0.641165742156689,0.555265820743996,0.641165742156689,0.555265820743996,
0.641165742156689,0.555265820743996,0.641165742156689,0.555265820743996,
0.641165742156689,0.555265820743996,0.641165742156689,0.555265820743996,
0.641165742156689,0.555265820743996,0.641165742156689,0.555265820743996,
0.641165742156689,0.555265820743996,0.641165742156689,0.555265820743996,
0.641165742156689,0.555265820743996,0.641165742156689,0.555265820743996,
0.641165742156689,0.555265820743996,0.641165742156689,0.555265820743996,
0.641165742156689,0.555265820743996,0.641165742156689,0.555265820743996,
0.641165742156689,0.555265820743996,0.641165742156689,0.555265820743996,
0.641165742156689,0.555265820743996,0.641165742156689,0.555265820743996,
0.641165742156689,0.555265820743996,0.641165742156689,0.555265820743996,
0.641165742156689,0.555265820743996,0.641165742156689,0.555265820743996,
0.641165742156689,0.555265820743996,0.641165742156689,0.555265820743996,
0.641165742156689,0.555265820743996,0.641165742156689,0.555265820743996,
0.641165742156689,0.555265820743996,0.641165742156689,0.555265820743996,
0.641165742156689,0.555265820743996,0.641165742156689,0.555265820743996,
0.641165742156689,0.555265820743996,0.641165742156689,0.555265820743996,
0.641165742156689,0.555265820743996,0.641165742156689,0.555265820743996,
0.641165742156689,0.555265820743996,0.641165742156689,0.555265820743996,
0.641165742156689,0.555265820743996,0.641165742156689,0.555265820743996,
0.641165742156689,0.555265820743996,0.641165742156689,0.555265820743996,
0.641165742156689,0.555265820743996,0.641165742156689,0.555265820743996,
0.641165742156689,0.555265820743996,0.641165742156689,0.555265820743996,
0.641165742156689,0.555265820743996,0.641165742156689,0.555265820743996,
0.641165742156689,0.555265820743996,0.641165742156689,0.555265820743996,
0.641165742156689,0.555265820743996,0.641165742156689,0.555265820743996,
0.641165742156689,0.555265820743996,0.641165742156689,0.555265820743996,
0.641165742156689,0.555265820743996,0.641165742156689,0.555265820743996,
0.641165742156689,0.555265820743996,0.641165742156689,0.555265820743996,
0.641165742156689,0.555265820743996,0.641165742156689,0.555265820743996,
0.641165742156689,0.555265820743996,0.641165742156689,0.555265820743996,
0.641165742156689,0.555265820743996,0.641165742156689,0.555265820743996,
0.641165742156689,0.555265820743996,0.641165742156689,0.555265820743996,
0.641165742156689,0.555265820743996,0.641165742156689,0.555265820743996,
0.641165742156689,0.555265820743996,0.641165742156689,0.555265820743996,
0.641165742156689,0.555265820743996,0.641165742156689,0.555265820743996,
0.641165742156689,0.555265820743996,0.641165742156689,0.555265820743996,
0.641165742156689,0.555265820743996,0.641165742156689,0.555265820743996,
0.641165742156689,0.555265820743996,0.641165742156689,0.555265820743996,
0.641165742156689,0.555265820743996,0.641165742156689,0.555265820743996,
0.641165742156689,0.555265820743996,0.641165742156689,0.555265820743996,
0.641165742156689,0.555265820743996,0.641165742156689,0.555265820743996,
0.641165742156689,0.555265820743996,0.641165742156689,0.555265820743996,
0.641165742156689,0.555265820743996,0.641165742156689,0.555265820743996,
0.641165742156689,0.555265820743996,0.641165742156689,0.555265820743996,
0.641165742156689,0.555265820743996,0.641165742156689,0.555265820743996,
0.641165742156689,0.555265820743996,0.641165742156689,0.555265820743996,
0.641165742156689,0.555265820743996,0.641165742156689,0.555265820743996,
0.641165742156689,0.555265820743996,0.641165742156689,0.555265820743996,
0.641165742156689,0.555265820743996,0.641165742156689,0.555265820743996,
0.641165742156689,0.555265820743996,0.641165742156689,0.555265820743996,
0.641165742156689,0.555265820743996,0.641165742156689,0.555265820743996,
0.641165742156689,0.555265820743996,0.641165742156689,0.555265820743996,
0.641165742156689,0.555265820743996,0.641165742156689,0.555265820743996,
0.641165742156689,0.555265820743996,0.641165742156689,0.555265820743996,
0.641165742156689,0.555265820743996,0.641165742156689,0.555265820743996,
0.641165742156689,0.555265820743996,0.641165742156689,0.555265820743996,
0.641165742156689,0.555265820743996,0.641165742156689,0.555265820743996,
0.641165742156689,0.555265820743996,0.641165742156689,0.555265820743996,
0.641165742156689,0.555265820743996,0.641165742156689,0.555265820743996,
0.641165742156689,0.555265820743996,0.641165742156689,0.555265820743996,
0.641165742156689,0.555265820743996,0.641165742156689,0.555265820743996,
0.641165742156689,0.555265820743996,0.641165742156689,0.555265820743996,
0.641165742156689,0.555265820743996,0.641165742156689,0.555265820743996,
0.641165742156689,0.555265820743996,0.641165742156689,0.555265820743996,
0.641165742156689,0.555265820743996,0.641165742156689,0.555265820743996,
0.641165742156689,0.555265820743996,0.641165742156689,0.555265820743996,
0.641165742156689,0.555265820743996,0.641165742156689,0.555265820743996,
0.641165742156689,0.555265820743996,0.641165742156689,0.555265820743996,
0.641165742156689,0.555265820743996,0.641165742156689,0.555265820743996,
0.641165742156689,0.555265820743996,0.641165742156689,0.555265820743996,
0.641165742156689,0.555265820743996,0.641165742156689,0.555265820743996,
0.641165742156689,0.555265820743996,0.641165742156689,0.555265820743996,
0.641165742156689,0.555265820743996,0.641165742156689,0.555265820743996,
0.641165742156689,0.555265820743996,0.641165742156689,0.555265820743996,
0.641165742156689,0.555265820743996,0.641165742156689,0.555265820743996,
0.641165742156689,0.555265820743996,0.641165742156689,0.555265820743996,
0.641165742156689,0.555265820743996,0.641165742156689,0.555265820743996,
0.641165742156689,0.555265820743996,0.641165742156689,0.555265820743996,
0.641165742156689,0.555265820743996,0.641165742156689,0.555265820743996,
0.641165742156689,0.555265820743996,0.641165742156689,0.555265820743996,
0.641165742156689,0.555265820743996,0.641165742156689,0.555265820743996,
0.641165742156689,0.555265820743996,0.641165742156689,0.555265820743996,
0.641165742156689,0.555265820743996,0.641165742156689,0.555265820743996,
0.641165742156689,0.555265820743996,0.641165742156689,0.555265820743996,
0.641165742156689,0.555265820743996,0.641165742156689,0.555265820743996,
0.641165742156689,0.555265820743996,0.641165742156689,0.555265820743996,
0.641165742156689,0.555265820743996,0.641165742156689,0.555265820743996,
0.641165742156689,0.555265820743996,0.641165742156689,0.555265820743996,
0.641165742156689,0.555265820743996,0.641165742156689,0.555265820743996,
0.641165742156689,0.555265820743996,0.641165742156689,0.555265820743996,
0.641165742156689,0.555265820743996,0.641165742156689,0.555265820743996,
0.641165742156689,0.555265820743996,0.641165742156689,0.555265820743996,
0.641165742156689,0.555265820743996,0.641165742156689,0.555265820743996,
0.641165742156689,0.555265820743996,0.641165742156689,0.555265820743996,
0.641165742156689,0.555265820743996,0.641165742156689,0.555265820743996,
0.641165742156689,0.555265820743996,0.641165742156689,0.555265820743996,
0.641165742156689,0.555265820743996,0.641165742156689,0.555265820743996,
0.641165742156689,0.555265820743996,0.641165742156689,0.555265820743996,
0.641165742156689,0.555265820743996,0.641165742156689,0.555265820743996,
0.641165742156689,0.555265820743996,0.641165742156689,0.555265820743996,
0.641165742156689,0.555265820743996,0.641165742156689,0.555265820743996,
0.641165742156689,0.555265820743996,0.641165742156689,0.555265820743996,
0.641165742156689,0.555265820743996,0.641165742156689,0.555265820743996,
0.641165742156689,0.555265820743996,0.641165742156689,0.555265820743996,
0.641165742156689,0.555265820743996,0.641165742156689,0.555265820743996,
0.641165742156689,0.555265820743996,0.641165742156689,0.555265820743996,
0.641165742156689,0.555265820743996,0.641165742156689,0.555265820743996,
0.641165742156689,0.555265820743996,0.641165742156689,0.555265820743996,
0.641165742156689,0.555265820743996,0.641165742156689,0.555265820743996,
0.641165742156689,0.555265820743996,0.641165742156689,0.555265820743996,
0.641165742156689,0.555265820743996,0.641165742156689,0.555265820743996,
0.641165742156689,0.555265820743996,0.641165742156689,0.555265820743996,
0.641165742156689,0.555265820743996,0.641165742156689,0.555265820743996,
0.641165742156689,0.555265820743996,0.641165742156689,0.555265820743996,
0.641165742156689,0.555265820743996,0.641165742156689,0.555265820743996,
0.641165742156689,0.555265820743996,0.641165742156689,0.555265820743996,
0.641165742156689,0.555265820743996,0.641165742156689,0.555265820743996,
0.641165742156689,0.555265820743996,0.641165742156689,0.555265820743996,
0.641165742156689,0.555265820743996,0.641165742156689,0.555265820743996,
0.641165742156689,0.555265820743996,0.641165742156689,0.555265820743996,
0.641165742156689,0.555265820743996,0.641165742156689,0.555265820743996,
0.641165742156689,0.555265820743996,0.641165742156689,0.555265820743996,
0.641165742156689,0.555265820743996,0.641165742156689,0.555265820743996,
0.641165742156689,0.555265820743996,0.641165742156689,0.555265820743996,
0.641165742156689,0.555265820743996,0.641165742156689,0.555265820743996,
0.641165742156689,0.555265820743996,0.641165742156689,0.555265820743996,
0.641165742156689,0.555265820743996,0.641165742156689,0.555265820743996,
0.641165742156689,0.555265820743996,0.641165742156689,0.555265820743996,
0.641165742156689,0.555265820743996,0.641165742156689,0.555265820743996,
0.641165742156689,0.555265820743996,0.641165742156689,0.555265820743996,
0.641165742156689,0.555265820743996,0.641165742156689,0.555265820743996,
0.641165742156689,0.555265820743996,0.641165742156689,0.555265820743996,
0.641165742156689,0.555265820743996,0.641165742156689,0.555265820743996,
0.641165742156689,0.555265820743996,0.641165742156689,0.555265820743996,
0.641165742156689,0.555265820743996,0.641165742156689,0.555265820743996,
0.641165742156689,0.555265820743996,0.641165742156689,0.555265820743996,
0.641165742156689,0.555265820743996,0.641165742156689,0.555265820743996,
0.641165742156689,0.555265820743996,0.641165742156689,0.555265820743996,
0.641165742156689,0.555265820743996,0.641165742156689,0.555265820743996,
0.641165742156689,0.555265820743996,0.641165742156689,0.555265820743996,
0.641165742156689,0.555265820743996,0.641165742156689,0.555265820743996,
0.641165742156689,0.555265820743996,0.641165742156689,0.555265820743996,
0.641165742156689,0.555265820743996,0.641165742156689,0.555265820743996,
0.641165742156689,0.555265820743996,0.641165742156689,0.555265820743996,
0.641165742156689,0.555265820743996,0.641165742156689,0.555265820743996,
0.641165742156689,0.555265820743996,0.641165742156689,0.555265820743996,
0.641165742156689,0.555265820743996,0.641165742156689,0.555265820743996,
0.641165742156689,0.555265820743996,0.641165742156689,0.555265820743996,
0.641165742156689,0.555265820743996,0.641165742156689,0.555265820743996,
0.641165742156689,0.555265820743996,0.641165742156689,0.555265820743996,
0.641165742156689,0.555265820743996,0.641165742156689,0.555265820743996,
0.641165742156689,0.555265820743996,0.641165742156689,0.555265820743996,
0.641165742156689,0.555265820743996,0.641165742156689,0.555265820743996,
0.641165742156689,0.555265820743996,0.641165742156689,0.555265820743996,
0.641165742156689,0.555265820743996,0.641165742156689,0.555265820743996,
0.641165742156689,0.555265820743996,0.641165742156689,0.555265820743996,
0.641165742156689,0.555265820743996,0.641165742156689,0.555265820743996,
0.641165742156689,0.555265820743996,0.641165742156689,0.555265820743996,
0.641165742156689,0.555265820743996,0.641165742156689,0.555265820743996,
0.641165742156689,0.555265820743996,0.641165742156689,0.555265820743996,
0.641165742156689,0.555265820743996,0.641165742156689,0.555265820743996,
0.641165742156689,0.555265820743996,0.641165742156689,0.555265820743996,
0.641165742156689,0.555265820743996,0.641165742156689,0.555265820743996,
0.641165742156689,0.555265820743996,0.641165742156689,0.555265820743996,
0.641165742156689,0.555265820743996,0.641165742156689,0.555265820743996,
0.641165742156689,0.555265820743996,0.641165742156689,0.555265820743996,
0.641165742156689,0.555265820743996,0.641165742156689,0.555265820743996,
0.641165742156689,0.555265820743996,0.641165742156689,0.555265820743996,
0.641165742156689,0.555265820743996,0.641165742156689,0.555265820743996,
0.641165742156689,0.555265820743996,0.641165742156689,0.555265820743996,
0.641165742156689,0.555265820743996,0.641165742156689,0.555265820743996,
0.641165742156689,0.555265820743996,0.641165742156689,0.555265820743996,
0.641165742156689,0.555265820743996,0.641165742156689,0.555265820743996,
0.641165742156689),(0.641165742156689,0.555265820743996,0.641165742156689,
0.555265820743996,0.641165742156689,0.555265820743996,0.641165742156689,
0.555265820743996,0.641165742156689,0.555265820743996,0.641165742156689,
0.555265820743996,0.641165742156689,0.555265820743996,0.641165742156689,
0.555265820743996,0.641165742156689,0.555265820743996,0.641165742156689,
0.555265820743996,0.641165742156689,0.555265820743996,0.641165742156689,
0.555265820743996,0.641165742156689,0.555265820743996,0.641165742156689,
0.555265820743996,0.641165742156689,0.555265820743996,0.641165742156689,
0.555265820743996,0.641165742156689,0.555265820743996,0.641165742156689,
0.555265820743996,0.641165742156689,0.555265820743996,0.641165742156689,
0.555265820743996,0.641165742156689,0.555265820743996,0.641165742156689,
0.555265820743996,0.641165742156689,0.555265820743996,0.641165742156689,
0.555265820743996,0.641165742156689,0.555265820743996,0.641165742156689,
0.555265820743996,0.641165742156689,0.555265820743996,0.641165742156689,
0.555265820743996,0.641165742156689,0.555265820743996,0.641165742156689,
0.555265820743996,0.641165742156689,0.555265820743996,0.641165742156689,
0.555265820743996,0.641165742156689,0.555265820743996,0.641165742156689,
0.555265820743996,0.641165742156689,0.555265820743996,0.641165742156689,
0.555265820743996,0.641165742156689,0.555265820743996,0.641165742156689,
0.555265820743996,0.641165742156689,0.555265820743996,0.641165742156689,
0.555265820743996,0.641165742156689,0.555265820743996,0.641165742156689,
0.555265820743996,0.641165742156689,0.555265820743996,0.641165742156689,
0.555265820743996,0.641165742156689,0.555265820743996,0.641165742156689,
0.555265820743996,0.641165742156689,0.555265820743996,0.641165742156689,
0.555265820743996,0.641165742156689,0.555265820743996,0.641165742156689,
0.555265820743996,0.641165742156689,0.555265820743996,0.641165742156689,
0.555265820743996,0.641165742156689,0.555265820743996,0.641165742156689,
0.555265820743996,0.641165742156689,0.555265820743996,0.641165742156689,
0.555265820743996,0.641165742156689,0.555265820743996,0.641165742156689,
0.555265820743996,0.641165742156689,0.555265820743996,0.641165742156689,
0.555265820743996,0.641165742156689,0.555265820743996,0.641165742156689,
0.555265820743996,0.641165742156689,0.555265820743996,0.641165742156689,
0.555265820743996,0.641165742156689,0.555265820743996,0.641165742156689,
0.555265820743996,0.641165742156689,0.555265820743996,0.641165742156689,
0.555265820743996,0.641165742156689,0.555265820743996,0.641165742156689,
0.555265820743996,0.641165742156689,0.555265820743996,0.641165742156689,
0.555265820743996,0.641165742156689,0.555265820743996,0.641165742156689,
0.555265820743996,0.641165742156689,0.555265820743996,0.641165742156689,
0.555265820743996,0.641165742156689,0.555265820743996,0.641165742156689,
0.555265820743996,0.641165742156689,0.555265820743996,0.641165742156689,
0.555265820743996,0.641165742156689,0.555265820743996,0.641165742156689,
0.555265820743996,0.641165742156689,0.555265820743996,0.641165742156689,
0.555265820743996,0.641165742156689,0.555265820743996,0.641165742156689,
0.555265820743996,0.641165742156689,0.555265820743996,0.641165742156689,
0.555265820743996,0.641165742156689,0.555265820743996,0.641165742156689,
0.555265820743996,0.641165742156689,0.555265820743996,0.641165742156689,
0.555265820743996,0.641165742156689,0.555265820743996,0.641165742156689,
0.555265820743996,0.641165742156689,0.555265820743996,0.641165742156689,
0.555265820743996,0.641165742156689,0.555265820743996,0.641165742156689,
0.555265820743996,0.641165742156689,0.555265820743996,0.641165742156689,
0.555265820743996,0.641165742156689,0.555265820743996,0.641165742156689,
0.555265820743996,0.641165742156689,0.555265820743996,0.641165742156689,
0.555265820743996,0.641165742156689,0.555265820743996,0.641165742156689,
0.555265820743996,0.641165742156689,0.555265820743996,0.641165742156689,
0.555265820743996,0.641165742156689,0.555265820743996,0.641165742156689,
0.555265820743996,0.641165742156689,0.555265820743996,0.641165742156689,
0.555265820743996,0.641165742156689,0.555265820743996,0.641165742156689,
0.555265820743996,0.641165742156689,0.555265820743996,0.641165742156689,
0.555265820743996,0.641165742156689,0.555265820743996,0.641165742156689,
0.555265820743996,0.641165742156689,0.555265820743996,0.641165742156689,
0.555265820743996,0.641165742156689,0.555265820743996,0.641165742156689,
0.555265820743996,0.641165742156689,0.555265820743996,0.641165742156689,
0.555265820743996,0.641165742156689,0.555265820743996,0.641165742156689,
0.555265820743996,0.641165742156689,0.555265820743996,0.641165742156689,
0.555265820743996,0.641165742156689,0.555265820743996,0.641165742156689,
0.555265820743996,0.641165742156689,0.555265820743996,0.641165742156689,
0.555265820743996,0.641165742156689,0.555265820743996,0.641165742156689,
0.555265820743996,0.641165742156689,0.555265820743996,0.641165742156689,
0.555265820743996,0.641165742156689,0.555265820743996,0.641165742156689,
0.555265820743996,0.641165742156689,0.555265820743996,0.641165742156689,
0.555265820743996,0.641165742156689,0.555265820743996,0.641165742156689,
0.555265820743996,0.641165742156689,0.555265820743996,0.641165742156689,
0.555265820743996,0.641165742156689,0.555265820743996,0.641165742156689,
0.555265820743996,0.641165742156689,0.555265820743996,0.641165742156689,
0.555265820743996,0.641165742156689,0.555265820743996,0.641165742156689,
0.555265820743996,0.641165742156689,0.555265820743996,0.641165742156689,
0.555265820743996,0.641165742156689,0.555265820743996,0.641165742156689,
0.555265820743996,0.641165742156689,0.555265820743996,0.641165742156689,
0.555265820743996,0.641165742156689,0.555265820743996,0.641165742156689,
0.555265820743996,0.641165742156689,0.555265820743996,0.641165742156689,
0.555265820743996,0.641165742156689,0.555265820743996,0.641165742156689,
0.555265820743996,0.641165742156689,0.555265820743996,0.641165742156689,
0.555265820743996,0.641165742156689,0.555265820743996,0.641165742156689,
0.555265820743996,0.641165742156689,0.555265820743996,0.641165742156689,
0.555265820743996,0.641165742156689,0.555265820743996,0.641165742156689,
0.555265820743996,0.641165742156689,0.555265820743996,0.641165742156689,
0.555265820743996,0.641165742156689,0.555265820743996,0.641165742156689,
0.555265820743996,0.641165742156689,0.555265820743996,0.641165742156689,
0.555265820743996,0.641165742156689,0.555265820743996,0.641165742156689,
0.555265820743996,0.641165742156689,0.555265820743996,0.641165742156689,
0.555265820743996,0.641165742156689,0.555265820743996,0.641165742156689,
0.555265820743996,0.641165742156689,0.555265820743996,0.641165742156689,
0.555265820743996,0.641165742156689,0.555265820743996,0.641165742156689,
0.555265820743996,0.641165742156689,0.555265820743996,0.641165742156689,
0.555265820743996,0.641165742156689,0.555265820743996,0.641165742156689,
0.555265820743996,0.641165742156689,0.555265820743996,0.641165742156689,
0.555265820743996,0.641165742156689,0.555265820743996,0.641165742156689,
0.555265820743996,0.641165742156689,0.555265820743996,0.641165742156689,
0.555265820743996,0.641165742156689,0.555265820743996,0.641165742156689,
0.555265820743996,0.641165742156689,0.555265820743996,0.641165742156689,
0.555265820743996,0.641165742156689,0.555265820743996,0.641165742156689,
0.555265820743996,0.641165742156689,0.555265820743996,0.641165742156689,
0.555265820743996,0.641165742156689,0.555265820743996,0.641165742156689,
0.555265820743996,0.641165742156689,0.555265820743996,0.641165742156689,
0.555265820743996,0.641165742156689,0.555265820743996,0.641165742156689,
0.555265820743996,0.641165742156689,0.555265820743996,0.641165742156689,
0.555265820743996,0.641165742156689,0.555265820743996,0.641165742156689,
0.555265820743996,0.641165742156689,0.555265820743996,0.641165742156689,
0.555265820743996,0.641165742156689,0.555265820743996,0.641165742156689,
0.555265820743996,0.641165742156689,0.555265820743996,0.641165742156689,
0.555265820743996,0.641165742156689,0.555265820743996,0.641165742156689,
0.555265820743996,0.641165742156689,0.555265820743996,0.641165742156689,
0.555265820743996,0.641165742156689,0.555265820743996,0.641165742156689,
0.555265820743996,0.641165742156689,0.555265820743996,0.641165742156689,
0.555265820743996,0.641165742156689,0.555265820743996,0.641165742156689,
0.555265820743996,0.641165742156689,0.555265820743996,0.641165742156689,
0.555265820743996,0.641165742156689,0.555265820743996,0.641165742156689,
0.555265820743996,0.641165742156689,0.555265820743996,0.641165742156689,
0.555265820743996,0.641165742156689,0.555265820743996,0.641165742156689,
0.555265820743996,0.641165742156689,0.555265820743996,0.641165742156689,
0.555265820743996,0.641165742156689,0.555265820743996,0.641165742156689,
0.555265820743996,0.641165742156689,0.555265820743996,0.641165742156689,
0.555265820743996,0.641165742156689,0.555265820743996,0.641165742156689,
0.555265820743996,0.641165742156689,0.555265820743996,0.641165742156689,
0.555265820743996,0.641165742156689,0.555265820743996,0.641165742156689,
0.555265820743996,0.641165742156689,0.555265820743996,0.641165742156689,
0.555265820743996,0.641165742156689,0.555265820743996,0.641165742156689,
0.555265820743996,0.641165742156689,0.555265820743996,0.641165742156689,
0.555265820743996,0.641165742156689,0.555265820743996,0.641165742156689,
0.555265820743996,0.641165742156689,0.555265820743996,0.641165742156689,
0.555265820743996,0.641165742156689,0.555265820743996,0.641165742156689,
0.555265820743996,0.641165742156689,0.555265820743996,0.641165742156689,
0.555265820743996,0.641165742156689,0.555265820743996,0.641165742156689,
0.555265820743996,0.641165742156689,0.555265820743996,0.641165742156689,
0.555265820743996,0.641165742156689,0.555265820743996,0.641165742156689,
0.555265820743996,0.641165742156689,0.555265820743996,0.641165742156689,
0.555265820743996,0.641165742156689,0.555265820743996,0.641165742156689,
0.555265820743996,0.641165742156689,0.555265820743996,0.641165742156689,
0.555265820743996,0.641165742156689,0.555265820743996,0.641165742156689,
0.555265820743996,0.641165742156689,0.555265820743996,0.641165742156689,
0.555265820743996,0.641165742156689,0.555265820743996,0.641165742156689,
0.555265820743996,0.641165742156689,0.555265820743996,0.641165742156689,
0.555265820743996,0.641165742156689,0.555265820743996,0.641165742156689,
0.555265820743996,0.641165742156689,0.555265820743996,0.641165742156689,
0.555265820743996,0.641165742156689,0.555265820743996,0.641165742156689,
0.555265820743996,0.641165742156689,0.555265820743996,0.641165742156689,
0.555265820743996,0.641165742156689,0.555265820743996,0.641165742156689,
0.555265820743996,0.641165742156689,0.555265820743996,0.641165742156689,
0.555265820743996,0.641165742156689,0.555265820743996,0.641165742156689,
0.555265820743996,0.641165742156689,0.555265820743996,0.641165742156689,
0.555265820743996,0.641165742156689,0.555265820743996,0.641165742156689,
0.555265820743996,0.641165742156689,0.555265820743996,0.641165742156689,
0.555265820743996,0.641165742156689,0.555265820743996,0.641165742156689,
0.555265820743996,0.641165742156689,0.555265820743996,0.641165742156689,
0.555265820743996,0.641165742156689,0.555265820743996,0.641165742156689,
0.555265820743996,0.641165742156689,0.555265820743996,0.641165742156689,
0.555265820743996,0.641165742156689,0.555265820743996,0.641165742156689,
0.555265820743996,0.641165742156689,0.555265820743996,0.641165742156689,
0.555265820743996,0.641165742156689,0.555265820743996,0.641165742156689,
0.555265820743996,0.641165742156689,0.555265820743996,0.641165742156689,
0.555265820743996,0.641165742156689,0.555265820743996,0.641165742156689,
0.555265820743996,0.641165742156689,0.555265820743996,0.641165742156689,
0.555265820743996,0.641165742156689,0.555265820743996,0.641165742156689,
0.555265820743996,0.641165742156689,0.555265820743996,0.641165742156689,
0.555265820743996,0.641165742156689,0.555265820743996,0.641165742156689,
0.555265820743996,0.641165742156689,0.555265820743996,0.641165742156689,
0.555265820743996,0.641165742156689,0.555265820743996,0.641165742156689,
0.555265820743996,0.641165742156689,0.555265820743996,0.641165742156689,
0.555265820743996,0.641165742156689,0.555265820743996,0.641165742156689,
0.555265820743996,0.641165742156689,0.555265820743996,0.641165742156689,
0.555265820743996,0.641165742156689,0.555265820743996,0.641165742156689,
0.555265820743996,0.641165742156689,0.555265820743996,0.641165742156689,
0.555265820743996,0.641165742156689,0.555265820743996,0.641165742156689,
0.555265820743996,0.641165742156689,0.555265820743996,0.641165742156689,
0.555265820743996,0.641165742156689,0.555265820743996,0.641165742156689,
0.555265820743996,0.641165742156689,0.555265820743996,0.641165742156689,
0.555265820743996,0.641165742156689,0.555265820743996,0.641165742156689,
0.555265820743996,0.641165742156689,0.555265820743996,0.641165742156689,
0.555265820743996,0.641165742156689,0.555265820743996,0.641165742156689,
0.555265820743996,0.641165742156689,0.555265820743996,0.641165742156689,
0.555265820743996,0.641165742156689,0.555265820743996,0.641165742156689,
0.555265820743996,0.641165742156689,0.555265820743996,0.641165742156689,
0.555265820743996,0.641165742156689,0.555265820743996,0.641165742156689,
0.555265820743996,0.641165742156689,0.555265820743996,0.641165742156689,
0.555265820743996,0.641165742156689,0.555265820743996,0.641165742156689,
0.555265820743996,0.641165742156689,0.555265820743996,0.641165742156689,
0.555265820743996,0.641165742156689,0.555265820743996,0.641165742156689,
0.555265820743996,0.641165742156689,0.555265820743996,0.641165742156689,
0.555265820743996,0.641165742156689,0.555265820743996,0.641165742156689,
0.555265820743996,0.641165742156689,0.555265820743996,0.641165742156689,
0.555265820743996,0.641165742156689,0.555265820743996,0.641165742156689,
0.555265820743996,0.641165742156689,0.555265820743996,0.641165742156689,
0.555265820743996,0.641165742156689,0.555265820743996,0.641165742156689,
0.555265820743996,0.641165742156689,0.555265820743996,0.641165742156689,
0.555265820743996,0.641165742156689,0.555265820743996,0.641165742156689,
0.555265820743996,0.641165742156689,0.555265820743996,0.641165742156689,
0.555265820743996,0.641165742156689,0.555265820743996,0.641165742156689,
0.555265820743996,0.641165742156689,0.555265820743996,0.641165742156689,
0.555265820743996,0.641165742156689,0.555265820743996,0.641165742156689,
0.555265820743996,0.641165742156689,0.555265820743996,0.641165742156689,
0.555265820743996,0.641165742156689,0.555265820743996,0.641165742156689,
0.555265820743996,0.641165742156689,0.555265820743996,0.641165742156689,
0.555265820743996,0.641165742156689,0.555265820743996,0.641165742156689,
0.555265820743996,0.641165742156689,0.555265820743996,0.641165742156689,
0.555265820743996,0.641165742156689,0.555265820743996,0.641165742156689,
0.555265820743996,0.641165742156689,0.555265820743996,0.641165742156689,
0.555265820743996,0.641165742156689,0.555265820743996,0.641165742156689,
0.555265820743996,0.641165742156689,0.555265820743996,0.641165742156689,
0.555265820743996,0.641165742156689,0.555265820743996,0.641165742156689,
0.555265820743996,0.641165742156689,0.555265820743996,0.641165742156689,
0.555265820743996,0.641165742156689,0.555265820743996,0.641165742156689,
0.555265820743996,0.641165742156689,0.555265820743996,0.641165742156689,
0.555265820743996,0.641165742156689,0.555265820743996,0.641165742156689,
0.555265820743996,0.641165742156689,0.555265820743996,0.641165742156689,
0.555265820743996,0.641165742156689,0.555265820743996,0.641165742156689,
0.555265820743996,0.641165742156689,0.555265820743996,0.641165742156689,
0.555265820743996,0.641165742156689,0.555265820743996,0.641165742156689,
0.555265820743996,0.641165742156689,0.555265820743996,0.641165742156689,
0.555265820743996,0.641165742156689,0.555265820743996,0.641165742156689,
0.555265820743996,0.641165742156689,0.555265820743996,0.641165742156689,
0.555265820743996,0.641165742156689,0.555265820743996,0.641165742156689,
0.555265820743996,0.641165742156689,0.555265820743996,0.641165742156689,
0.555265820743996,0.641165742156689,0.555265820743996,0.641165742156689,
0.555265820743996,0.641165742156689,0.555265820743996,0.641165742156689,
0.555265820743996,0.641165742156689,0.555265820743996,0.641165742156689,
0.555265820743996,0.641165742156689,0.555265820743996,0.641165742156689,
0.555265820743996,0.641165742156689,0.555265820743996,0.641165742156689,
0.555265820743996,0.641165742156689,0.555265820743996,0.641165742156689,
0.555265820743996,0.641165742156689,0.555265820743996,0.641165742156689,
0.555265820743996,0.641165742156689,0.555265820743996,0.641165742156689,
0.555265820743996,0.641165742156689,0.555265820743996,0.641165742156689,
0.555265820743996,0.641165742156689,0.555265820743996,0.641165742156689,
0.555265820743996,0.641165742156689,0.555265820743996,0.641165742156689,
0.555265820743996,0.641165742156689,0.555265820743996,0.641165742156689,
0.555265820743996,0.641165742156689,0.555265820743996,0.641165742156689,
0.555265820743996,0.641165742156689,0.555265820743996,0.641165742156689,
0.555265820743996,0.641165742156689,0.555265820743996,0.641165742156689,
0.555265820743996,0.641165742156689,0.555265820743996,0.641165742156689,
0.555265820743996,0.641165742156689,0.555265820743996,0.641165742156689,
0.555265820743996,0.641165742156689,0.555265820743996,0.641165742156689,
0.555265820743996,0.641165742156689,0.555265820743996,0.641165742156689,
0.555265820743996,0.641165742156689,0.555265820743996,0.641165742156689,
0.555265820743996,0.641165742156689,0.555265820743996,0.641165742156689,
0.555265820743996,0.641165742156689),(1.,0.866025403784439,1.,0.866025403784439,
1.,0.866025403784439,1.,0.866025403784439,1.,0.866025403784439,1.,0.866025403784439,
1.,0.866025403784439,1.,0.866025403784439,1.,0.866025403784439,1.,0.866025403784439,
1.,0.866025403784439,1.,0.866025403784439,1.,0.866025403784439,1.,0.866025403784439,
1.,0.866025403784439,1.,0.866025403784439,1.,0.866025403784439,1.,0.866025403784439,
1.,0.866025403784439,1.,0.866025403784439,1.,0.866025403784439,1.,0.866025403784439,
1.,0.866025403784439,1.,0.866025403784439,1.,0.866025403784439,1.,0.866025403784439,
1.,0.866025403784439,1.,0.866025403784439,1.,0.866025403784439,1.,0.866025403784439,
1.,0.866025403784439,1.,0.866025403784439,1.,0.866025403784439,1.,0.866025403784439,
1.,0.866025403784439,1.,0.866025403784439,1.,0.866025403784439,1.,0.866025403784439,
1.,0.866025403784439,1.,0.866025403784439,1.,0.866025403784439,1.,0.866025403784439,
1.,0.866025403784439,1.,0.866025403784439,1.,0.866025403784439,1.,0.866025403784439,
1.,0.866025403784439,1.,0.866025403784439,1.,0.866025403784439,1.,0.866025403784439,
1.,0.866025403784439,1.,0.866025403784439,1.,0.866025403784439,1.,0.866025403784439,
1.,0.866025403784439,1.,0.866025403784439,1.,0.866025403784439,1.,0.866025403784439,
1.,0.866025403784439,1.,0.866025403784439,1.,0.866025403784439,1.,0.866025403784439,
1.,0.866025403784439,1.,0.866025403784439,1.,0.866025403784439,1.,0.866025403784439,
1.,0.866025403784439,1.,0.866025403784439,1.,0.866025403784439,1.,0.866025403784439,
1.,0.866025403784439,1.,0.866025403784439,1.,0.866025403784439,1.,0.866025403784439,
1.,0.866025403784439,1.,0.866025403784439,1.,0.866025403784439,1.,0.866025403784439,
1.,0.866025403784439,1.,0.866025403784439,1.,0.866025403784439,1.,0.866025403784439,
1.,0.866025403784439,1.,0.866025403784439,1.,0.866025403784439,1.,0.866025403784439,
1.,0.866025403784439,1.,0.866025403784439,1.,0.866025403784439,1.,0.866025403784439,
1.,0.866025403784439,1.,0.866025403784439,1.,0.866025403784439,1.,0.866025403784439,
1.,0.866025403784439,1.,0.866025403784439,1.,0.866025403784439,1.,0.866025403784439,
1.,0.866025403784439,1.,0.866025403784439,1.,0.866025403784439,1.,0.866025403784439,
1.,0.866025403784439,1.,0.866025403784439,1.,0.866025403784439,1.,0.866025403784439,
1.,0.866025403784439,1.,0.866025403784439,1.,0.866025403784439,1.,0.866025403784439,
1.,0.866025403784439,1.,0.866025403784439,1.,0.866025403784439,1.,0.866025403784439,
1.,0.866025403784439,1.,0.866025403784439,1.,0.866025403784439,1.,0.866025403784439,
1.,0.866025403784439,1.,0.866025403784439,1.,0.866025403784439,1.,0.866025403784439,
1.,0.866025403784439,1.,0.866025403784439,1.,0.866025403784439,1.,0.866025403784439,
1.,0.866025403784439,1.,0.866025403784439,1.,0.866025403784439,1.,0.866025403784439,
1.,0.866025403784439,1.,0.866025403784439,1.,0.866025403784439,1.,0.866025403784439,
1.,0.866025403784439,1.,0.866025403784439,1.,0.866025403784439,1.,0.866025403784439,
1.,0.866025403784439,1.,0.866025403784439,1.,0.866025403784439,1.,0.866025403784439,
1.,0.866025403784439,1.,0.866025403784439,1.,0.866025403784439,1.,0.866025403784439,
1.,0.866025403784439,1.,0.866025403784439,1.,0.866025403784439,1.,0.866025403784439,
1.,0.866025403784439,1.,0.866025403784439,1.,0.866025403784439,1.,0.866025403784439,
1.,0.866025403784439,1.,0.866025403784439,1.,0.866025403784439,1.,0.866025403784439,
1.,0.866025403784439,1.,0.866025403784439,1.,0.866025403784439,1.,0.866025403784439,
1.,0.866025403784439,1.,0.866025403784439,1.,0.866025403784439,1.,0.866025403784439,
1.,0.866025403784439,1.,0.866025403784439,1.,0.866025403784439,1.,0.866025403784439,
1.,0.866025403784439,1.,0.866025403784439,1.,0.866025403784439,1.,0.866025403784439,
1.,0.866025403784439,1.,0.866025403784439,1.,0.866025403784439,1.,0.866025403784439,
1.,0.866025403784439,1.,0.866025403784439,1.,0.866025403784439,1.,0.866025403784439,
1.,0.866025403784439,1.,0.866025403784439,1.,0.866025403784439,1.,0.866025403784439,
1.,0.866025403784439,1.,0.866025403784439,1.,0.866025403784439,1.,0.866025403784439,
1.,0.866025403784439,1.,0.866025403784439,1.,0.866025403784439,1.,0.866025403784439,
1.,0.866025403784439,1.,0.866025403784439,1.,0.866025403784439,1.,0.866025403784439,
1.,0.866025403784439,1.,0.866025403784439,1.,0.866025403784439,1.,0.866025403784439,
1.,0.866025403784439,1.,0.866025403784439,1.,0.866025403784439,1.,0.866025403784439,
1.,0.866025403784439,1.,0.866025403784439,1.,0.866025403784439,1.,0.866025403784439,
1.,0.866025403784439,1.,0.866025403784439,1.,0.866025403784439,1.,0.866025403784439,
1.,0.866025403784439,1.,0.866025403784439,1.,0.866025403784439,1.,0.866025403784439,
1.,0.866025403784439,1.,0.866025403784439,1.,0.866025403784439,1.,0.866025403784439,
1.,0.866025403784439,1.,0.866025403784439,1.,0.866025403784439,1.,0.866025403784439,
1.,0.866025403784439,1.,0.866025403784439,1.,0.866025403784439,1.,0.866025403784439,
1.,0.866025403784439,1.,0.866025403784439,1.,0.866025403784439,1.,0.866025403784439,
1.,0.866025403784439,1.,0.866025403784439,1.,0.866025403784439,1.,0.866025403784439,
1.,0.866025403784439,1.,0.866025403784439,1.,0.866025403784439,1.,0.866025403784439,
1.,0.866025403784439,1.,0.866025403784439,1.,0.866025403784439,1.,0.866025403784439,
1.,0.866025403784439,1.,0.866025403784439,1.,0.866025403784439,1.,0.866025403784439,
1.,0.866025403784439,1.,0.866025403784439,1.,0.866025403784439,1.,0.866025403784439,
1.,0.866025403784439,1.,0.866025403784439,1.,0.866025403784439,1.,0.866025403784439,
1.,0.866025403784439,1.,0.866025403784439,1.,0.866025403784439,1.,0.866025403784439,
1.,0.866025403784439,1.,0.866025403784439,1.,0.866025403784439,1.,0.866025403784439,
1.,0.866025403784439,1.,0.866025403784439,1.,0.866025403784439,1.,0.866025403784439,
1.,0.866025403784439,1.,0.866025403784439,1.,0.866025403784439,1.,0.866025403784439,
1.,0.866025403784439,1.,0.866025403784439,1.,0.866025403784439,1.,0.866025403784439,
1.,0.866025403784439,1.,0.866025403784439,1.,0.866025403784439,1.,0.866025403784439,
1.,0.866025403784439,1.,0.866025403784439,1.,0.866025403784439,1.,0.866025403784439,
1.,0.866025403784439,1.,0.866025403784439,1.,0.866025403784439,1.,0.866025403784439,
1.,0.866025403784439,1.,0.866025403784439,1.,0.866025403784439,1.,0.866025403784439,
1.,0.866025403784439,1.,0.866025403784439,1.,0.866025403784439,1.,0.866025403784439,
1.,0.866025403784439,1.,0.866025403784439,1.,0.866025403784439,1.,0.866025403784439,
1.,0.866025403784439,1.,0.866025403784439,1.,0.866025403784439,1.,0.866025403784439,
1.,0.866025403784439,1.,0.866025403784439,1.,0.866025403784439,1.,0.866025403784439,
1.,0.866025403784439,1.,0.866025403784439,1.,0.866025403784439,1.,0.866025403784439,
1.,0.866025403784439,1.,0.866025403784439,1.,0.866025403784439,1.,0.866025403784439,
1.,0.866025403784439,1.,0.866025403784439,1.,0.866025403784439,1.,0.866025403784439,
1.,0.866025403784439,1.,0.866025403784439,1.,0.866025403784439,1.,0.866025403784439,
1.,0.866025403784439,1.,0.866025403784439,1.,0.866025403784439,1.,0.866025403784439,
1.,0.866025403784439,1.,0.866025403784439,1.,0.866025403784439,1.,0.866025403784439,
1.,0.866025403784439,1.,0.866025403784439,1.,0.866025403784439,1.,0.866025403784439,
1.,0.866025403784439,1.,0.866025403784439,1.,0.866025403784439,1.,0.866025403784439,
1.,0.866025403784439,1.,0.866025403784439,1.,0.866025403784439,1.,0.866025403784439,
1.,0.866025403784439,1.,0.866025403784439,1.,0.866025403784439,1.,0.866025403784439,
1.,0.866025403784439,1.,0.866025403784439,1.,0.866025403784439,1.,0.866025403784439,
1.,0.866025403784439,1.,0.866025403784439,1.,0.866025403784439,1.,0.866025403784439,
1.,0.866025403784439,1.,0.866025403784439,1.,0.866025403784439,1.,0.866025403784439,
1.,0.866025403784439,1.,0.866025403784439,1.,0.866025403784439,1.,0.866025403784439,
1.,0.866025403784439,1.,0.866025403784439,1.,0.866025403784439,1.,0.866025403784439,
1.,0.866025403784439,1.,0.866025403784439,1.,0.866025403784439,1.,0.866025403784439,
1.,0.866025403784439,1.,0.866025403784439,1.,0.866025403784439,1.,0.866025403784439,
1.,0.866025403784439,1.,0.866025403784439,1.,0.866025403784439,1.,0.866025403784439,
1.,0.866025403784439,1.,0.866025403784439,1.,0.866025403784439,1.,0.866025403784439,
1.,0.866025403784439,1.,0.866025403784439,1.,0.866025403784439,1.,0.866025403784439,
1.,0.866025403784439,1.,0.866025403784439,1.,0.866025403784439,1.,0.866025403784439,
1.,0.866025403784439,1.,0.866025403784439,1.,0.866025403784439,1.,0.866025403784439,
1.,0.866025403784439,1.,0.866025403784439,1.,0.866025403784439,1.,0.866025403784439,
1.,0.866025403784439,1.,0.866025403784439,1.,0.866025403784439,1.,0.866025403784439,
1.,0.866025403784439,1.,0.866025403784439,1.,0.866025403784439,1.,0.866025403784439,
1.,0.866025403784439,1.,0.866025403784439,1.,0.866025403784439,1.,0.866025403784439,
1.,0.866025403784439,1.,0.866025403784439,1.,0.866025403784439,1.,0.866025403784439,
1.,0.866025403784439,1.,0.866025403784439,1.,0.866025403784439,1.,0.866025403784439,
1.,0.866025403784439,1.,0.866025403784439,1.,0.866025403784439,1.,0.866025403784439,
1.,0.866025403784439,1.,0.866025403784439,1.,0.866025403784439,1.,0.866025403784439,
1.,0.866025403784439,1.,0.866025403784439,1.,0.866025403784439,1.,0.866025403784439,
1.,0.866025403784439,1.,0.866025403784439,1.,0.866025403784439,1.,0.866025403784439,
1.,0.866025403784439,1.,0.866025403784439,1.,0.866025403784439,1.,0.866025403784439,
1.,0.866025403784439,1.,0.866025403784439,1.,0.866025403784439,1.,0.866025403784439,
1.,0.866025403784439,1.,0.866025403784439,1.,0.866025403784439,1.,0.866025403784439,
1.,0.866025403784439,1.,0.866025403784439,1.,0.866025403784439,1.,0.866025403784439,
1.,0.866025403784439,1.,0.866025403784439,1.,0.866025403784439,1.,0.866025403784439,
1.,0.866025403784439,1.,0.866025403784439,1.,0.866025403784439,1.,0.866025403784439,
1.,0.866025403784439,1.,0.866025403784439,1.,0.866025403784439,1.,0.866025403784439,
1.,0.866025403784439,1.,0.866025403784439,1.,0.866025403784439,1.,0.866025403784439,
1.,0.866025403784439,1.,0.866025403784439,1.,0.866025403784439,1.,0.866025403784439,
1.,0.866025403784439,1.,0.866025403784439,1.,0.866025403784439,1.,0.866025403784439,
1.,0.866025403784439,1.,0.866025403784439,1.,0.866025403784439,1.,0.866025403784439,
1.,0.866025403784439,1.,0.866025403784439,1.,0.866025403784439,1.,0.866025403784439,
1.)))
REPRESENTATION_ITEM('')
SURFACE()
);
#150=(
BOUNDED_SURFACE()
B_SPLINE_SURFACE(1,2,((#19439,#19440,#19441,#19442,#19443,#19444,#19445,
#19446,#19447,#19448,#19449,#19450,#19451,#19452,#19453,#19454,#19455,#19456,
#19457,#19458,#19459,#19460,#19461,#19462,#19463,#19464,#19465,#19466,#19467,
#19468,#19469,#19470,#19471,#19472,#19473,#19474,#19475,#19476,#19477,#19478,
#19479,#19480,#19481,#19482,#19483,#19484,#19485,#19486,#19487,#19488,#19489,
#19490,#19491,#19492,#19493,#19494,#19495,#19496,#19497,#19498,#19499,#19500,
#19501,#19502,#19503,#19504,#19505,#19506,#19507,#19508,#19509,#19510,#19511,
#19512,#19513,#19514,#19515,#19516,#19517,#19518,#19519,#19520,#19521,#19522,
#19523,#19524,#19525,#19526,#19527,#19528,#19529,#19530,#19531,#19532,#19533,
#19534,#19535,#19536,#19537,#19538,#19539,#19540,#19541,#19542,#19543,#19544,
#19545,#19546,#19547,#19548,#19549,#19550,#19551,#19552,#19553,#19554,#19555,
#19556,#19557,#19558,#19559,#19560,#19561,#19562,#19563,#19564,#19565,#19566,
#19567,#19568,#19569,#19570,#19571,#19572,#19573,#19574,#19575,#19576,#19577,
#19578,#19579,#19580,#19581,#19582,#19583,#19584,#19585,#19586,#19587,#19588,
#19589,#19590,#19591,#19592,#19593,#19594,#19595,#19596,#19597,#19598,#19599,
#19600,#19601,#19602,#19603,#19604,#19605,#19606,#19607,#19608,#19609,#19610,
#19611,#19612,#19613,#19614,#19615,#19616,#19617,#19618,#19619,#19620,#19621,
#19622,#19623,#19624,#19625,#19626,#19627,#19628,#19629,#19630,#19631,#19632,
#19633,#19634,#19635,#19636,#19637,#19638,#19639,#19640,#19641,#19642,#19643,
#19644,#19645,#19646,#19647,#19648,#19649,#19650,#19651,#19652,#19653,#19654,
#19655,#19656,#19657,#19658,#19659,#19660,#19661,#19662,#19663,#19664,#19665,
#19666,#19667,#19668,#19669,#19670,#19671,#19672,#19673,#19674,#19675,#19676,
#19677,#19678,#19679,#19680,#19681,#19682,#19683,#19684,#19685,#19686,#19687,
#19688,#19689,#19690,#19691,#19692,#19693,#19694,#19695,#19696,#19697,#19698,
#19699,#19700,#19701,#19702,#19703,#19704,#19705,#19706,#19707,#19708,#19709,
#19710,#19711,#19712,#19713,#19714,#19715,#19716,#19717,#19718,#19719,#19720,
#19721,#19722,#19723,#19724,#19725,#19726,#19727,#19728,#19729,#19730,#19731,
#19732,#19733,#19734,#19735,#19736,#19737,#19738,#19739,#19740,#19741,#19742,
#19743,#19744,#19745,#19746,#19747,#19748,#19749,#19750,#19751,#19752,#19753,
#19754,#19755,#19756,#19757,#19758,#19759,#19760,#19761,#19762,#19763,#19764,
#19765,#19766,#19767,#19768,#19769,#19770,#19771,#19772,#19773,#19774,#19775,
#19776,#19777,#19778,#19779,#19780,#19781,#19782,#19783,#19784,#19785,#19786,
#19787,#19788,#19789,#19790,#19791,#19792,#19793,#19794,#19795,#19796,#19797,
#19798,#19799,#19800,#19801,#19802,#19803,#19804,#19805,#19806,#19807,#19808,
#19809,#19810,#19811,#19812,#19813,#19814,#19815,#19816,#19817,#19818,#19819,
#19820,#19821,#19822,#19823,#19824,#19825,#19826,#19827,#19828,#19829,#19830,
#19831,#19832,#19833,#19834,#19835,#19836,#19837,#19838,#19839,#19840,#19841,
#19842,#19843,#19844,#19845,#19846,#19847,#19848,#19849,#19850,#19851,#19852,
#19853,#19854,#19855,#19856,#19857,#19858,#19859,#19860,#19861,#19862,#19863,
#19864,#19865,#19866,#19867,#19868,#19869,#19870,#19871,#19872,#19873,#19874,
#19875,#19876,#19877,#19878,#19879,#19880,#19881,#19882,#19883,#19884,#19885,
#19886,#19887,#19888,#19889,#19890,#19891,#19892,#19893,#19894,#19895,#19896,
#19897,#19898,#19899,#19900,#19901,#19902,#19903,#19904,#19905,#19906,#19907,
#19908,#19909,#19910,#19911,#19912,#19913,#19914,#19915,#19916,#19917,#19918,
#19919,#19920,#19921,#19922,#19923,#19924,#19925,#19926,#19927,#19928,#19929,
#19930,#19931,#19932,#19933,#19934,#19935,#19936,#19937,#19938,#19939,#19940,
#19941,#19942,#19943,#19944,#19945,#19946,#19947,#19948,#19949,#19950,#19951,
#19952,#19953,#19954,#19955,#19956,#19957,#19958,#19959,#19960,#19961,#19962,
#19963,#19964,#19965,#19966,#19967,#19968,#19969,#19970,#19971,#19972,#19973,
#19974,#19975,#19976,#19977,#19978,#19979,#19980,#19981,#19982,#19983,#19984,
#19985,#19986,#19987,#19988,#19989,#19990,#19991,#19992,#19993,#19994,#19995,
#19996,#19997,#19998,#19999,#20000,#20001,#20002,#20003,#20004,#20005,#20006,
#20007,#20008,#20009,#20010,#20011,#20012,#20013,#20014,#20015,#20016,#20017,
#20018,#20019,#20020,#20021,#20022,#20023,#20024,#20025,#20026,#20027,#20028,
#20029,#20030,#20031,#20032,#20033,#20034,#20035,#20036,#20037,#20038,#20039,
#20040,#20041,#20042,#20043,#20044,#20045,#20046,#20047,#20048,#20049,#20050,
#20051,#20052,#20053,#20054,#20055,#20056,#20057,#20058,#20059,#20060,#20061,
#20062,#20063,#20064,#20065,#20066,#20067,#20068,#20069,#20070,#20071,#20072,
#20073,#20074,#20075,#20076,#20077,#20078,#20079,#20080,#20081,#20082,#20083,
#20084,#20085,#20086,#20087,#20088,#20089,#20090,#20091,#20092,#20093,#20094,
#20095,#20096,#20097,#20098,#20099,#20100,#20101,#20102,#20103,#20104,#20105,
#20106,#20107,#20108,#20109,#20110,#20111,#20112,#20113,#20114,#20115,#20116,
#20117,#20118,#20119,#20120,#20121,#20122,#20123,#20124,#20125,#20126,#20127,
#20128,#20129,#20130,#20131,#20132,#20133,#20134,#20135,#20136,#20137,#20138,
#20139,#20140,#20141,#20142,#20143,#20144,#20145,#20146,#20147,#20148,#20149,
#20150,#20151,#20152,#20153,#20154,#20155,#20156,#20157,#20158,#20159,#20160,
#20161,#20162,#20163,#20164,#20165,#20166,#20167,#20168,#20169,#20170,#20171,
#20172,#20173,#20174,#20175,#20176,#20177,#20178,#20179,#20180,#20181,#20182,
#20183,#20184,#20185,#20186,#20187,#20188,#20189,#20190,#20191,#20192,#20193,
#20194,#20195,#20196,#20197,#20198,#20199,#20200,#20201,#20202,#20203,#20204,
#20205,#20206,#20207,#20208,#20209,#20210,#20211,#20212,#20213,#20214,#20215,
#20216,#20217,#20218,#20219,#20220,#20221,#20222,#20223,#20224,#20225,#20226,
#20227,#20228,#20229,#20230,#20231,#20232,#20233,#20234,#20235,#20236,#20237,
#20238,#20239,#20240,#20241,#20242,#20243,#20244,#20245,#20246,#20247,#20248,
#20249,#20250,#20251,#20252,#20253,#20254,#20255,#20256,#20257,#20258,#20259,
#20260,#20261,#20262,#20263,#20264,#20265,#20266,#20267,#20268,#20269,#20270,
#20271,#20272,#20273,#20274,#20275,#20276,#20277,#20278,#20279,#20280,#20281,
#20282,#20283,#20284,#20285,#20286,#20287,#20288,#20289,#20290,#20291,#20292,
#20293,#20294,#20295,#20296,#20297,#20298,#20299,#20300,#20301,#20302,#20303,
#20304,#20305,#20306,#20307,#20308,#20309,#20310,#20311,#20312,#20313,#20314,
#20315,#20316,#20317,#20318,#20319,#20320,#20321,#20322,#20323,#20324,#20325,
#20326,#20327,#20328,#20329,#20330,#20331,#20332,#20333,#20334,#20335,#20336,
#20337,#20338,#20339,#20340,#20341,#20342,#20343,#20344,#20345,#20346,#20347,
#20348,#20349,#20350,#20351,#20352,#20353,#20354,#20355,#20356,#20357,#20358,
#20359,#20360,#20361,#20362,#20363,#20364,#20365,#20366,#20367,#20368,#20369,
#20370,#20371,#20372,#20373,#20374,#20375,#20376,#20377,#20378,#20379,#20380,
#20381,#20382,#20383,#20384,#20385,#20386,#20387,#20388,#20389,#20390,#20391,
#20392,#20393,#20394,#20395,#20396,#20397,#20398,#20399,#20400,#20401,#20402,
#20403,#20404,#20405,#20406,#20407,#20408,#20409,#20410,#20411),(#20412,
#20413,#20414,#20415,#20416,#20417,#20418,#20419,#20420,#20421,#20422,#20423,
#20424,#20425,#20426,#20427,#20428,#20429,#20430,#20431,#20432,#20433,#20434,
#20435,#20436,#20437,#20438,#20439,#20440,#20441,#20442,#20443,#20444,#20445,
#20446,#20447,#20448,#20449,#20450,#20451,#20452,#20453,#20454,#20455,#20456,
#20457,#20458,#20459,#20460,#20461,#20462,#20463,#20464,#20465,#20466,#20467,
#20468,#20469,#20470,#20471,#20472,#20473,#20474,#20475,#20476,#20477,#20478,
#20479,#20480,#20481,#20482,#20483,#20484,#20485,#20486,#20487,#20488,#20489,
#20490,#20491,#20492,#20493,#20494,#20495,#20496,#20497,#20498,#20499,#20500,
#20501,#20502,#20503,#20504,#20505,#20506,#20507,#20508,#20509,#20510,#20511,
#20512,#20513,#20514,#20515,#20516,#20517,#20518,#20519,#20520,#20521,#20522,
#20523,#20524,#20525,#20526,#20527,#20528,#20529,#20530,#20531,#20532,#20533,
#20534,#20535,#20536,#20537,#20538,#20539,#20540,#20541,#20542,#20543,#20544,
#20545,#20546,#20547,#20548,#20549,#20550,#20551,#20552,#20553,#20554,#20555,
#20556,#20557,#20558,#20559,#20560,#20561,#20562,#20563,#20564,#20565,#20566,
#20567,#20568,#20569,#20570,#20571,#20572,#20573,#20574,#20575,#20576,#20577,
#20578,#20579,#20580,#20581,#20582,#20583,#20584,#20585,#20586,#20587,#20588,
#20589,#20590,#20591,#20592,#20593,#20594,#20595,#20596,#20597,#20598,#20599,
#20600,#20601,#20602,#20603,#20604,#20605,#20606,#20607,#20608,#20609,#20610,
#20611,#20612,#20613,#20614,#20615,#20616,#20617,#20618,#20619,#20620,#20621,
#20622,#20623,#20624,#20625,#20626,#20627,#20628,#20629,#20630,#20631,#20632,
#20633,#20634,#20635,#20636,#20637,#20638,#20639,#20640,#20641,#20642,#20643,
#20644,#20645,#20646,#20647,#20648,#20649,#20650,#20651,#20652,#20653,#20654,
#20655,#20656,#20657,#20658,#20659,#20660,#20661,#20662,#20663,#20664,#20665,
#20666,#20667,#20668,#20669,#20670,#20671,#20672,#20673,#20674,#20675,#20676,
#20677,#20678,#20679,#20680,#20681,#20682,#20683,#20684,#20685,#20686,#20687,
#20688,#20689,#20690,#20691,#20692,#20693,#20694,#20695,#20696,#20697,#20698,
#20699,#20700,#20701,#20702,#20703,#20704,#20705,#20706,#20707,#20708,#20709,
#20710,#20711,#20712,#20713,#20714,#20715,#20716,#20717,#20718,#20719,#20720,
#20721,#20722,#20723,#20724,#20725,#20726,#20727,#20728,#20729,#20730,#20731,
#20732,#20733,#20734,#20735,#20736,#20737,#20738,#20739,#20740,#20741,#20742,
#20743,#20744,#20745,#20746,#20747,#20748,#20749,#20750,#20751,#20752,#20753,
#20754,#20755,#20756,#20757,#20758,#20759,#20760,#20761,#20762,#20763,#20764,
#20765,#20766,#20767,#20768,#20769,#20770,#20771,#20772,#20773,#20774,#20775,
#20776,#20777,#20778,#20779,#20780,#20781,#20782,#20783,#20784,#20785,#20786,
#20787,#20788,#20789,#20790,#20791,#20792,#20793,#20794,#20795,#20796,#20797,
#20798,#20799,#20800,#20801,#20802,#20803,#20804,#20805,#20806,#20807,#20808,
#20809,#20810,#20811,#20812,#20813,#20814,#20815,#20816,#20817,#20818,#20819,
#20820,#20821,#20822,#20823,#20824,#20825,#20826,#20827,#20828,#20829,#20830,
#20831,#20832,#20833,#20834,#20835,#20836,#20837,#20838,#20839,#20840,#20841,
#20842,#20843,#20844,#20845,#20846,#20847,#20848,#20849,#20850,#20851,#20852,
#20853,#20854,#20855,#20856,#20857,#20858,#20859,#20860,#20861,#20862,#20863,
#20864,#20865,#20866,#20867,#20868,#20869,#20870,#20871,#20872,#20873,#20874,
#20875,#20876,#20877,#20878,#20879,#20880,#20881,#20882,#20883,#20884,#20885,
#20886,#20887,#20888,#20889,#20890,#20891,#20892,#20893,#20894,#20895,#20896,
#20897,#20898,#20899,#20900,#20901,#20902,#20903,#20904,#20905,#20906,#20907,
#20908,#20909,#20910,#20911,#20912,#20913,#20914,#20915,#20916,#20917,#20918,
#20919,#20920,#20921,#20922,#20923,#20924,#20925,#20926,#20927,#20928,#20929,
#20930,#20931,#20932,#20933,#20934,#20935,#20936,#20937,#20938,#20939,#20940,
#20941,#20942,#20943,#20944,#20945,#20946,#20947,#20948,#20949,#20950,#20951,
#20952,#20953,#20954,#20955,#20956,#20957,#20958,#20959,#20960,#20961,#20962,
#20963,#20964,#20965,#20966,#20967,#20968,#20969,#20970,#20971,#20972,#20973,
#20974,#20975,#20976,#20977,#20978,#20979,#20980,#20981,#20982,#20983,#20984,
#20985,#20986,#20987,#20988,#20989,#20990,#20991,#20992,#20993,#20994,#20995,
#20996,#20997,#20998,#20999,#21000,#21001,#21002,#21003,#21004,#21005,#21006,
#21007,#21008,#21009,#21010,#21011,#21012,#21013,#21014,#21015,#21016,#21017,
#21018,#21019,#21020,#21021,#21022,#21023,#21024,#21025,#21026,#21027,#21028,
#21029,#21030,#21031,#21032,#21033,#21034,#21035,#21036,#21037,#21038,#21039,
#21040,#21041,#21042,#21043,#21044,#21045,#21046,#21047,#21048,#21049,#21050,
#21051,#21052,#21053,#21054,#21055,#21056,#21057,#21058,#21059,#21060,#21061,
#21062,#21063,#21064,#21065,#21066,#21067,#21068,#21069,#21070,#21071,#21072,
#21073,#21074,#21075,#21076,#21077,#21078,#21079,#21080,#21081,#21082,#21083,
#21084,#21085,#21086,#21087,#21088,#21089,#21090,#21091,#21092,#21093,#21094,
#21095,#21096,#21097,#21098,#21099,#21100,#21101,#21102,#21103,#21104,#21105,
#21106,#21107,#21108,#21109,#21110,#21111,#21112,#21113,#21114,#21115,#21116,
#21117,#21118,#21119,#21120,#21121,#21122,#21123,#21124,#21125,#21126,#21127,
#21128,#21129,#21130,#21131,#21132,#21133,#21134,#21135,#21136,#21137,#21138,
#21139,#21140,#21141,#21142,#21143,#21144,#21145,#21146,#21147,#21148,#21149,
#21150,#21151,#21152,#21153,#21154,#21155,#21156,#21157,#21158,#21159,#21160,
#21161,#21162,#21163,#21164,#21165,#21166,#21167,#21168,#21169,#21170,#21171,
#21172,#21173,#21174,#21175,#21176,#21177,#21178,#21179,#21180,#21181,#21182,
#21183,#21184,#21185,#21186,#21187,#21188,#21189,#21190,#21191,#21192,#21193,
#21194,#21195,#21196,#21197,#21198,#21199,#21200,#21201,#21202,#21203,#21204,
#21205,#21206,#21207,#21208,#21209,#21210,#21211,#21212,#21213,#21214,#21215,
#21216,#21217,#21218,#21219,#21220,#21221,#21222,#21223,#21224,#21225,#21226,
#21227,#21228,#21229,#21230,#21231,#21232,#21233,#21234,#21235,#21236,#21237,
#21238,#21239,#21240,#21241,#21242,#21243,#21244,#21245,#21246,#21247,#21248,
#21249,#21250,#21251,#21252,#21253,#21254,#21255,#21256,#21257,#21258,#21259,
#21260,#21261,#21262,#21263,#21264,#21265,#21266,#21267,#21268,#21269,#21270,
#21271,#21272,#21273,#21274,#21275,#21276,#21277,#21278,#21279,#21280,#21281,
#21282,#21283,#21284,#21285,#21286,#21287,#21288,#21289,#21290,#21291,#21292,
#21293,#21294,#21295,#21296,#21297,#21298,#21299,#21300,#21301,#21302,#21303,
#21304,#21305,#21306,#21307,#21308,#21309,#21310,#21311,#21312,#21313,#21314,
#21315,#21316,#21317,#21318,#21319,#21320,#21321,#21322,#21323,#21324,#21325,
#21326,#21327,#21328,#21329,#21330,#21331,#21332,#21333,#21334,#21335,#21336,
#21337,#21338,#21339,#21340,#21341,#21342,#21343,#21344,#21345,#21346,#21347,
#21348,#21349,#21350,#21351,#21352,#21353,#21354,#21355,#21356,#21357,#21358,
#21359,#21360,#21361,#21362,#21363,#21364,#21365,#21366,#21367,#21368,#21369,
#21370,#21371,#21372,#21373,#21374,#21375,#21376,#21377,#21378,#21379,#21380,
#21381,#21382,#21383,#21384)),.UNSPECIFIED.,.F.,.F.,.F.)
B_SPLINE_SURFACE_WITH_KNOTS((2,2),(3,2,2,2,2,2,2,2,2,2,2,2,2,2,2,2,2,2,
2,2,2,2,2,2,2,2,2,2,2,2,2,2,2,2,2,2,2,2,2,2,2,2,2,2,2,2,2,2,2,2,2,2,2,2,
2,2,2,2,2,2,2,2,2,2,2,2,2,2,2,2,2,2,2,2,2,2,2,2,2,2,2,2,2,2,2,2,2,2,2,2,
2,2,2,2,2,2,2,2,2,2,2,2,2,2,2,2,2,2,2,2,2,2,2,2,2,2,2,2,2,2,2,2,2,2,2,2,
2,2,2,2,2,2,2,2,2,2,2,2,2,2,2,2,2,2,2,2,2,2,2,2,2,2,2,2,2,2,2,2,2,2,2,2,
2,2,2,2,2,2,2,2,2,2,2,2,2,2,2,2,2,2,2,2,2,2,2,2,2,2,2,2,2,2,2,2,2,2,2,2,
2,2,2,2,2,2,2,2,2,2,2,2,2,2,2,2,2,2,2,2,2,2,2,2,2,2,2,2,2,2,2,2,2,2,2,2,
2,2,2,2,2,2,2,2,2,2,2,2,2,2,2,2,2,2,2,2,2,2,2,2,2,2,2,2,2,2,2,2,2,2,2,2,
2,2,2,2,2,2,2,2,2,2,2,2,2,2,2,2,2,2,2,2,2,2,2,2,2,2,2,2,2,2,2,2,2,2,2,2,
2,2,2,2,2,2,2,2,2,2,2,2,2,2,2,2,2,2,2,2,2,2,2,2,2,2,2,2,2,2,2,2,2,2,2,2,
2,2,2,2,2,2,2,2,2,2,2,2,2,2,2,2,2,2,2,2,2,2,2,2,2,2,2,2,2,2,2,2,2,2,2,2,
2,2,2,2,2,2,2,2,2,2,2,2,2,2,2,2,2,2,2,2,2,2,2,2,2,2,2,2,2,2,2,2,2,2,2,2,
2,2,2,2,2,2,2,2,2,2,2,2,2,2,2,2,2,2,2,2,2,2,2,2,2,2,2,2,2,2,2,2,2,2,2,2,
2,2,2,2,2,2,2,2,2,2,2,2,2,2,2,2,2,2,2,2,2,2,2,2,2,2,2,2,2,2,2,2,2,2,2,2,
3),(-1.70634721592824E-6,1.),(0.,0.00205761316872428,0.00411522633744856,
0.00617283950617284,0.00823045267489712,0.0102880658436214,0.0123456790123457,
0.01440329218107,0.0164609053497942,0.0185185185185185,0.0205761316872428,
0.0226337448559671,0.0246913580246914,0.0267489711934156,0.0288065843621399,
0.0308641975308642,0.0329218106995885,0.0349794238683128,0.037037037037037,
0.0390946502057613,0.0411522633744856,0.0432098765432099,0.0452674897119342,
0.0473251028806584,0.0493827160493827,0.051440329218107,0.0534979423868313,
0.0555555555555556,0.0576131687242798,0.0596707818930041,0.0617283950617284,
0.0637860082304527,0.065843621399177,0.0679012345679012,0.0699588477366255,
0.0720164609053498,0.0740740740740741,0.0761316872427984,0.0781893004115226,
0.0802469135802469,0.0823045267489712,0.0843621399176955,0.0864197530864197,
0.088477366255144,0.0905349794238683,0.0925925925925926,0.0946502057613169,
0.0967078189300412,0.0987654320987654,0.10082304526749,0.102880658436214,
0.104938271604938,0.106995884773663,0.109053497942387,0.111111111111111,
0.113168724279835,0.11522633744856,0.117283950617284,0.119341563786008,
0.121399176954733,0.123456790123457,0.125514403292181,0.127572016460905,
0.12962962962963,0.131687242798354,0.133744855967078,0.135802469135802,
0.137860082304527,0.139917695473251,0.141975308641975,0.1440329218107,0.146090534979424,
0.148148148148148,0.150205761316872,0.152263374485597,0.154320987654321,
0.156378600823045,0.15843621399177,0.160493827160494,0.162551440329218,
0.164609053497942,0.166666666666667,0.168724279835391,0.170781893004115,
0.172839506172839,0.174897119341564,0.176954732510288,0.179012345679012,
0.181069958847737,0.183127572016461,0.185185185185185,0.187242798353909,
0.189300411522634,0.191358024691358,0.193415637860082,0.195473251028807,
0.197530864197531,0.199588477366255,0.201646090534979,0.203703703703704,
0.205761316872428,0.207818930041152,0.209876543209877,0.211934156378601,
0.213991769547325,0.216049382716049,0.218106995884774,0.220164609053498,
0.222222222222222,0.224279835390947,0.226337448559671,0.228395061728395,
0.230452674897119,0.232510288065844,0.234567901234568,0.236625514403292,
0.238683127572016,0.240740740740741,0.242798353909465,0.244855967078189,
0.246913580246914,0.248971193415638,0.251028806584362,0.253086419753086,
0.255144032921811,0.257201646090535,0.259259259259259,0.261316872427984,
0.263374485596708,0.265432098765432,0.267489711934156,0.269547325102881,
0.271604938271605,0.273662551440329,0.275720164609054,0.277777777777778,
0.279835390946502,0.281893004115226,0.283950617283951,0.286008230452675,
0.288065843621399,0.290123456790123,0.292181069958848,0.294238683127572,
0.296296296296296,0.298353909465021,0.300411522633745,0.302469135802469,
0.304526748971193,0.306584362139918,0.308641975308642,0.310699588477366,
0.312757201646091,0.314814814814815,0.316872427983539,0.318930041152263,
0.320987654320988,0.323045267489712,0.325102880658436,0.327160493827161,
0.329218106995885,0.331275720164609,0.333333333333333,0.335390946502058,
0.337448559670782,0.339506172839506,0.34156378600823,0.343621399176955,
0.345679012345679,0.347736625514403,0.349794238683128,0.351851851851852,
0.353909465020576,0.3559670781893,0.358024691358025,0.360082304526749,0.362139917695473,
0.364197530864198,0.366255144032922,0.368312757201646,0.37037037037037,
0.372427983539095,0.374485596707819,0.376543209876543,0.378600823045267,
0.380658436213992,0.382716049382716,0.38477366255144,0.386831275720165,
0.388888888888889,0.390946502057613,0.393004115226337,0.395061728395062,
0.397119341563786,0.39917695473251,0.401234567901235,0.403292181069959,
0.405349794238683,0.407407407407407,0.409465020576132,0.411522633744856,
0.41358024691358,0.415637860082305,0.417695473251029,0.419753086419753,
0.421810699588477,0.423868312757202,0.425925925925926,0.42798353909465,
0.430041152263374,0.432098765432099,0.434156378600823,0.436213991769547,
0.438271604938272,0.440329218106996,0.44238683127572,0.444444444444444,
0.446502057613169,0.448559670781893,0.450617283950617,0.452674897119342,
0.454732510288066,0.45679012345679,0.458847736625514,0.460905349794239,
0.462962962962963,0.465020576131687,0.467078189300412,0.469135802469136,
0.47119341563786,0.473251028806584,0.475308641975309,0.477366255144033,
0.479423868312757,0.481481481481481,0.483539094650206,0.48559670781893,
0.487654320987654,0.489711934156379,0.491769547325103,0.493827160493827,
0.495884773662551,0.497942386831276,0.5,0.502057613168724,0.504115226337449,
0.506172839506173,0.508230452674897,0.510288065843621,0.512345679012346,
0.51440329218107,0.516460905349794,0.518518518518518,0.520576131687243,
0.522633744855967,0.524691358024691,0.526748971193416,0.52880658436214,
0.530864197530864,0.532921810699588,0.534979423868313,0.537037037037037,
0.539094650205761,0.541152263374486,0.54320987654321,0.545267489711934,
0.547325102880658,0.549382716049383,0.551440329218107,0.553497942386831,
0.555555555555556,0.55761316872428,0.559670781893004,0.561728395061728,
0.563786008230453,0.565843621399177,0.567901234567901,0.569958847736626,
0.57201646090535,0.574074074074074,0.576131687242798,0.578189300411523,
0.580246913580247,0.582304526748971,0.584362139917695,0.58641975308642,
0.588477366255144,0.590534979423868,0.592592592592593,0.594650205761317,
0.596707818930041,0.598765432098765,0.60082304526749,0.602880658436214,
0.604938271604938,0.606995884773663,0.609053497942387,0.611111111111111,
0.613168724279835,0.61522633744856,0.617283950617284,0.619341563786008,
0.621399176954732,0.623456790123457,0.625514403292181,0.627572016460905,
0.62962962962963,0.631687242798354,0.633744855967078,0.635802469135803,
0.637860082304527,0.639917695473251,0.641975308641975,0.6440329218107,0.646090534979424,
0.648148148148148,0.650205761316872,0.652263374485597,0.654320987654321,
0.656378600823045,0.65843621399177,0.660493827160494,0.662551440329218,
0.664609053497942,0.666666666666667,0.668724279835391,0.670781893004115,
0.672839506172839,0.674897119341564,0.676954732510288,0.679012345679012,
0.681069958847737,0.683127572016461,0.685185185185185,0.687242798353909,
0.689300411522634,0.691358024691358,0.693415637860082,0.695473251028807,
0.697530864197531,0.699588477366255,0.701646090534979,0.703703703703704,
0.705761316872428,0.707818930041152,0.709876543209877,0.711934156378601,
0.713991769547325,0.716049382716049,0.718106995884774,0.720164609053498,
0.722222222222222,0.724279835390947,0.726337448559671,0.728395061728395,
0.730452674897119,0.732510288065844,0.734567901234568,0.736625514403292,
0.738683127572016,0.740740740740741,0.742798353909465,0.744855967078189,
0.746913580246914,0.748971193415638,0.751028806584362,0.753086419753086,
0.755144032921811,0.757201646090535,0.759259259259259,0.761316872427984,
0.763374485596708,0.765432098765432,0.767489711934156,0.769547325102881,
0.771604938271605,0.773662551440329,0.775720164609053,0.777777777777778,
0.779835390946502,0.781893004115226,0.783950617283951,0.786008230452675,
0.788065843621399,0.790123456790123,0.792181069958848,0.794238683127572,
0.796296296296296,0.798353909465021,0.800411522633745,0.802469135802469,
0.804526748971193,0.806584362139918,0.808641975308642,0.810699588477366,
0.812757201646091,0.814814814814815,0.816872427983539,0.818930041152263,
0.820987654320988,0.823045267489712,0.825102880658436,0.827160493827161,
0.829218106995885,0.831275720164609,0.833333333333333,0.835390946502058,
0.837448559670782,0.839506172839506,0.84156378600823,0.843621399176955,
0.845679012345679,0.847736625514403,0.849794238683128,0.851851851851852,
0.853909465020576,0.8559670781893,0.858024691358025,0.860082304526749,0.862139917695473,
0.864197530864197,0.866255144032922,0.868312757201646,0.87037037037037,
0.872427983539095,0.874485596707819,0.876543209876543,0.878600823045268,
0.880658436213992,0.882716049382716,0.88477366255144,0.886831275720165,
0.888888888888889,0.890946502057613,0.893004115226337,0.895061728395062,
0.897119341563786,0.89917695473251,0.901234567901235,0.903292181069959,
0.905349794238683,0.907407407407407,0.909465020576132,0.911522633744856,
0.91358024691358,0.915637860082305,0.917695473251029,0.919753086419753,
0.921810699588477,0.923868312757202,0.925925925925926,0.92798353909465,
0.930041152263374,0.932098765432099,0.934156378600823,0.936213991769547,
0.938271604938272,0.940329218106996,0.94238683127572,0.944444444444444,
0.946502057613169,0.948559670781893,0.950617283950617,0.952674897119342,
0.954732510288066,0.95679012345679,0.958847736625514,0.960905349794239,
0.962962962962963,0.965020576131687,0.967078189300412,0.969135802469136,
0.97119341563786,0.973251028806584,0.975308641975309,0.977366255144033,
0.979423868312757,0.981481481481482,0.983539094650206,0.98559670781893,
0.987654320987654,0.989711934156379,0.991769547325103,0.993827160493827,
0.995884773662551,0.997942386831276,1.),.UNSPECIFIED.)
GEOMETRIC_REPRESENTATION_ITEM()
RATIONAL_B_SPLINE_SURFACE(((1.,0.866025403784439,1.,0.866025403784439,1.,
0.866025403784439,1.,0.866025403784439,1.,0.866025403784439,1.,0.866025403784439,
1.,0.866025403784439,1.,0.866025403784439,1.,0.866025403784439,1.,0.866025403784439,
1.,0.866025403784439,1.,0.866025403784439,1.,0.866025403784439,1.,0.866025403784439,
1.,0.866025403784439,1.,0.866025403784439,1.,0.866025403784439,1.,0.866025403784439,
1.,0.866025403784439,1.,0.866025403784439,1.,0.866025403784439,1.,0.866025403784439,
1.,0.866025403784439,1.,0.866025403784439,1.,0.866025403784439,1.,0.866025403784439,
1.,0.866025403784439,1.,0.866025403784439,1.,0.866025403784439,1.,0.866025403784439,
1.,0.866025403784439,1.,0.866025403784439,1.,0.866025403784439,1.,0.866025403784439,
1.,0.866025403784439,1.,0.866025403784439,1.,0.866025403784439,1.,0.866025403784439,
1.,0.866025403784439,1.,0.866025403784439,1.,0.866025403784439,1.,0.866025403784439,
1.,0.866025403784439,1.,0.866025403784439,1.,0.866025403784439,1.,0.866025403784439,
1.,0.866025403784439,1.,0.866025403784439,1.,0.866025403784439,1.,0.866025403784439,
1.,0.866025403784439,1.,0.866025403784439,1.,0.866025403784439,1.,0.866025403784439,
1.,0.866025403784439,1.,0.866025403784439,1.,0.866025403784439,1.,0.866025403784439,
1.,0.866025403784439,1.,0.866025403784439,1.,0.866025403784439,1.,0.866025403784439,
1.,0.866025403784439,1.,0.866025403784439,1.,0.866025403784439,1.,0.866025403784439,
1.,0.866025403784439,1.,0.866025403784439,1.,0.866025403784439,1.,0.866025403784439,
1.,0.866025403784439,1.,0.866025403784439,1.,0.866025403784439,1.,0.866025403784439,
1.,0.866025403784439,1.,0.866025403784439,1.,0.866025403784439,1.,0.866025403784439,
1.,0.866025403784439,1.,0.866025403784439,1.,0.866025403784439,1.,0.866025403784439,
1.,0.866025403784439,1.,0.866025403784439,1.,0.866025403784439,1.,0.866025403784439,
1.,0.866025403784439,1.,0.866025403784439,1.,0.866025403784439,1.,0.866025403784439,
1.,0.866025403784439,1.,0.866025403784439,1.,0.866025403784439,1.,0.866025403784439,
1.,0.866025403784439,1.,0.866025403784439,1.,0.866025403784439,1.,0.866025403784439,
1.,0.866025403784439,1.,0.866025403784439,1.,0.866025403784439,1.,0.866025403784439,
1.,0.866025403784439,1.,0.866025403784439,1.,0.866025403784439,1.,0.866025403784439,
1.,0.866025403784439,1.,0.866025403784439,1.,0.866025403784439,1.,0.866025403784439,
1.,0.866025403784439,1.,0.866025403784439,1.,0.866025403784439,1.,0.866025403784439,
1.,0.866025403784439,1.,0.866025403784439,1.,0.866025403784439,1.,0.866025403784439,
1.,0.866025403784439,1.,0.866025403784439,1.,0.866025403784439,1.,0.866025403784439,
1.,0.866025403784439,1.,0.866025403784439,1.,0.866025403784439,1.,0.866025403784439,
1.,0.866025403784439,1.,0.866025403784439,1.,0.866025403784439,1.,0.866025403784439,
1.,0.866025403784439,1.,0.866025403784439,1.,0.866025403784439,1.,0.866025403784439,
1.,0.866025403784439,1.,0.866025403784439,1.,0.866025403784439,1.,0.866025403784439,
1.,0.866025403784439,1.,0.866025403784439,1.,0.866025403784439,1.,0.866025403784439,
1.,0.866025403784439,1.,0.866025403784439,1.,0.866025403784439,1.,0.866025403784439,
1.,0.866025403784439,1.,0.866025403784439,1.,0.866025403784439,1.,0.866025403784439,
1.,0.866025403784439,1.,0.866025403784439,1.,0.866025403784439,1.,0.866025403784439,
1.,0.866025403784439,1.,0.866025403784439,1.,0.866025403784439,1.,0.866025403784439,
1.,0.866025403784439,1.,0.866025403784439,1.,0.866025403784439,1.,0.866025403784439,
1.,0.866025403784439,1.,0.866025403784439,1.,0.866025403784439,1.,0.866025403784439,
1.,0.866025403784439,1.,0.866025403784439,1.,0.866025403784439,1.,0.866025403784439,
1.,0.866025403784439,1.,0.866025403784439,1.,0.866025403784439,1.,0.866025403784439,
1.,0.866025403784439,1.,0.866025403784439,1.,0.866025403784439,1.,0.866025403784439,
1.,0.866025403784439,1.,0.866025403784439,1.,0.866025403784439,1.,0.866025403784439,
1.,0.866025403784439,1.,0.866025403784439,1.,0.866025403784439,1.,0.866025403784439,
1.,0.866025403784439,1.,0.866025403784439,1.,0.866025403784439,1.,0.866025403784439,
1.,0.866025403784439,1.,0.866025403784439,1.,0.866025403784439,1.,0.866025403784439,
1.,0.866025403784439,1.,0.866025403784439,1.,0.866025403784439,1.,0.866025403784439,
1.,0.866025403784439,1.,0.866025403784439,1.,0.866025403784439,1.,0.866025403784439,
1.,0.866025403784439,1.,0.866025403784439,1.,0.866025403784439,1.,0.866025403784439,
1.,0.866025403784439,1.,0.866025403784439,1.,0.866025403784439,1.,0.866025403784439,
1.,0.866025403784439,1.,0.866025403784439,1.,0.866025403784439,1.,0.866025403784439,
1.,0.866025403784439,1.,0.866025403784439,1.,0.866025403784439,1.,0.866025403784439,
1.,0.866025403784439,1.,0.866025403784439,1.,0.866025403784439,1.,0.866025403784439,
1.,0.866025403784439,1.,0.866025403784439,1.,0.866025403784439,1.,0.866025403784439,
1.,0.866025403784439,1.,0.866025403784439,1.,0.866025403784439,1.,0.866025403784439,
1.,0.866025403784439,1.,0.866025403784439,1.,0.866025403784439,1.,0.866025403784439,
1.,0.866025403784439,1.,0.866025403784439,1.,0.866025403784439,1.,0.866025403784439,
1.,0.866025403784439,1.,0.866025403784439,1.,0.866025403784439,1.,0.866025403784439,
1.,0.866025403784439,1.,0.866025403784439,1.,0.866025403784439,1.,0.866025403784439,
1.,0.866025403784439,1.,0.866025403784439,1.,0.866025403784439,1.,0.866025403784439,
1.,0.866025403784439,1.,0.866025403784439,1.,0.866025403784439,1.,0.866025403784439,
1.,0.866025403784439,1.,0.866025403784439,1.,0.866025403784439,1.,0.866025403784439,
1.,0.866025403784439,1.,0.866025403784439,1.,0.866025403784439,1.,0.866025403784439,
1.,0.866025403784439,1.,0.866025403784439,1.,0.866025403784439,1.,0.866025403784439,
1.,0.866025403784439,1.,0.866025403784439,1.,0.866025403784439,1.,0.866025403784439,
1.,0.866025403784439,1.,0.866025403784439,1.,0.866025403784439,1.,0.866025403784439,
1.,0.866025403784439,1.,0.866025403784439,1.,0.866025403784439,1.,0.866025403784439,
1.,0.866025403784439,1.,0.866025403784439,1.,0.866025403784439,1.,0.866025403784439,
1.,0.866025403784439,1.,0.866025403784439,1.,0.866025403784439,1.,0.866025403784439,
1.,0.866025403784439,1.,0.866025403784439,1.,0.866025403784439,1.,0.866025403784439,
1.,0.866025403784439,1.,0.866025403784439,1.,0.866025403784439,1.,0.866025403784439,
1.,0.866025403784439,1.,0.866025403784439,1.,0.866025403784439,1.,0.866025403784439,
1.,0.866025403784439,1.,0.866025403784439,1.,0.866025403784439,1.,0.866025403784439,
1.,0.866025403784439,1.,0.866025403784439,1.,0.866025403784439,1.,0.866025403784439,
1.,0.866025403784439,1.,0.866025403784439,1.,0.866025403784439,1.,0.866025403784439,
1.,0.866025403784439,1.,0.866025403784439,1.,0.866025403784439,1.,0.866025403784439,
1.,0.866025403784439,1.,0.866025403784439,1.,0.866025403784439,1.,0.866025403784439,
1.,0.866025403784439,1.,0.866025403784439,1.,0.866025403784439,1.,0.866025403784439,
1.,0.866025403784439,1.,0.866025403784439,1.,0.866025403784439,1.,0.866025403784439,
1.,0.866025403784439,1.,0.866025403784439,1.,0.866025403784439,1.,0.866025403784439,
1.,0.866025403784439,1.,0.866025403784439,1.,0.866025403784439,1.,0.866025403784439,
1.,0.866025403784439,1.,0.866025403784439,1.,0.866025403784439,1.,0.866025403784439,
1.,0.866025403784439,1.,0.866025403784439,1.,0.866025403784439,1.,0.866025403784439,
1.,0.866025403784439,1.,0.866025403784439,1.,0.866025403784439,1.,0.866025403784439,
1.,0.866025403784439,1.,0.866025403784439,1.,0.866025403784439,1.,0.866025403784439,
1.,0.866025403784439,1.,0.866025403784439,1.,0.866025403784439,1.,0.866025403784439,
1.,0.866025403784439,1.,0.866025403784439,1.,0.866025403784439,1.,0.866025403784439,
1.,0.866025403784439,1.,0.866025403784439,1.,0.866025403784439,1.,0.866025403784439,
1.,0.866025403784439,1.,0.866025403784439,1.,0.866025403784439,1.,0.866025403784439,
1.,0.866025403784439,1.,0.866025403784439,1.,0.866025403784439,1.,0.866025403784439,
1.,0.866025403784439,1.,0.866025403784439,1.,0.866025403784439,1.,0.866025403784439,
1.,0.866025403784439,1.,0.866025403784439,1.,0.866025403784439,1.,0.866025403784439,
1.,0.866025403784439,1.,0.866025403784439,1.,0.866025403784439,1.,0.866025403784439,
1.,0.866025403784439,1.,0.866025403784439,1.,0.866025403784439,1.,0.866025403784439,
1.,0.866025403784439,1.,0.866025403784439,1.,0.866025403784439,1.,0.866025403784439,
1.,0.866025403784439,1.,0.866025403784439,1.,0.866025403784439,1.,0.866025403784439,
1.,0.866025403784439,1.,0.866025403784439,1.,0.866025403784439,1.,0.866025403784439,
1.,0.866025403784439,1.,0.866025403784439,1.,0.866025403784439,1.,0.866025403784439,
1.,0.866025403784439,1.,0.866025403784439,1.,0.866025403784439,1.,0.866025403784439,
1.,0.866025403784439,1.,0.866025403784439,1.,0.866025403784439,1.,0.866025403784439,
1.,0.866025403784439,1.,0.866025403784439,1.,0.866025403784439,1.,0.866025403784439,
1.,0.866025403784439,1.,0.866025403784439,1.,0.866025403784439,1.,0.866025403784439,
1.,0.866025403784439,1.,0.866025403784439,1.,0.866025403784439,1.,0.866025403784439,
1.,0.866025403784439,1.,0.866025403784439,1.,0.866025403784439,1.,0.866025403784439,
1.,0.866025403784439,1.,0.866025403784439,1.,0.866025403784439,1.,0.866025403784439,
1.,0.866025403784439,1.,0.866025403784439,1.,0.866025403784439,1.,0.866025403784439,
1.,0.866025403784439,1.,0.866025403784439,1.,0.866025403784439,1.,0.866025403784439,
1.,0.866025403784439,1.,0.866025403784439,1.,0.866025403784439,1.,0.866025403784439,
1.,0.866025403784439,1.,0.866025403784439,1.,0.866025403784439,1.,0.866025403784439,
1.,0.866025403784439,1.,0.866025403784439,1.,0.866025403784439,1.,0.866025403784439,
1.,0.866025403784439,1.,0.866025403784439,1.,0.866025403784439,1.,0.866025403784439,
1.,0.866025403784439,1.,0.866025403784439,1.,0.866025403784439,1.,0.866025403784439,
1.,0.866025403784439,1.,0.866025403784439,1.,0.866025403784439,1.,0.866025403784439,
1.,0.866025403784439,1.,0.866025403784439,1.,0.866025403784439,1.,0.866025403784439,
1.,0.866025403784439,1.,0.866025403784439,1.,0.866025403784439,1.,0.866025403784439,
1.,0.866025403784439,1.,0.866025403784439,1.,0.866025403784439,1.,0.866025403784439,
1.,0.866025403784439,1.,0.866025403784439,1.,0.866025403784439,1.,0.866025403784439,
1.,0.866025403784439,1.,0.866025403784439,1.,0.866025403784439,1.,0.866025403784439,
1.,0.866025403784439,1.,0.866025403784439,1.,0.866025403784439,1.,0.866025403784439,
1.),(1.,0.866025403784439,1.,0.866025403784439,1.,0.866025403784439,1.,
0.866025403784439,1.,0.866025403784439,1.,0.866025403784439,1.,0.866025403784439,
1.,0.866025403784439,1.,0.866025403784439,1.,0.866025403784439,1.,0.866025403784439,
1.,0.866025403784439,1.,0.866025403784439,1.,0.866025403784439,1.,0.866025403784439,
1.,0.866025403784439,1.,0.866025403784439,1.,0.866025403784439,1.,0.866025403784439,
1.,0.866025403784439,1.,0.866025403784439,1.,0.866025403784439,1.,0.866025403784439,
1.,0.866025403784439,1.,0.866025403784439,1.,0.866025403784439,1.,0.866025403784439,
1.,0.866025403784439,1.,0.866025403784439,1.,0.866025403784439,1.,0.866025403784439,
1.,0.866025403784439,1.,0.866025403784439,1.,0.866025403784439,1.,0.866025403784439,
1.,0.866025403784439,1.,0.866025403784439,1.,0.866025403784439,1.,0.866025403784439,
1.,0.866025403784439,1.,0.866025403784439,1.,0.866025403784439,1.,0.866025403784439,
1.,0.866025403784439,1.,0.866025403784439,1.,0.866025403784439,1.,0.866025403784439,
1.,0.866025403784439,1.,0.866025403784439,1.,0.866025403784439,1.,0.866025403784439,
1.,0.866025403784439,1.,0.866025403784439,1.,0.866025403784439,1.,0.866025403784439,
1.,0.866025403784439,1.,0.866025403784439,1.,0.866025403784439,1.,0.866025403784439,
1.,0.866025403784439,1.,0.866025403784439,1.,0.866025403784439,1.,0.866025403784439,
1.,0.866025403784439,1.,0.866025403784439,1.,0.866025403784439,1.,0.866025403784439,
1.,0.866025403784439,1.,0.866025403784439,1.,0.866025403784439,1.,0.866025403784439,
1.,0.866025403784439,1.,0.866025403784439,1.,0.866025403784439,1.,0.866025403784439,
1.,0.866025403784439,1.,0.866025403784439,1.,0.866025403784439,1.,0.866025403784439,
1.,0.866025403784439,1.,0.866025403784439,1.,0.866025403784439,1.,0.866025403784439,
1.,0.866025403784439,1.,0.866025403784439,1.,0.866025403784439,1.,0.866025403784439,
1.,0.866025403784439,1.,0.866025403784439,1.,0.866025403784439,1.,0.866025403784439,
1.,0.866025403784439,1.,0.866025403784439,1.,0.866025403784439,1.,0.866025403784439,
1.,0.866025403784439,1.,0.866025403784439,1.,0.866025403784439,1.,0.866025403784439,
1.,0.866025403784439,1.,0.866025403784439,1.,0.866025403784439,1.,0.866025403784439,
1.,0.866025403784439,1.,0.866025403784439,1.,0.866025403784439,1.,0.866025403784439,
1.,0.866025403784439,1.,0.866025403784439,1.,0.866025403784439,1.,0.866025403784439,
1.,0.866025403784439,1.,0.866025403784439,1.,0.866025403784439,1.,0.866025403784439,
1.,0.866025403784439,1.,0.866025403784439,1.,0.866025403784439,1.,0.866025403784439,
1.,0.866025403784439,1.,0.866025403784439,1.,0.866025403784439,1.,0.866025403784439,
1.,0.866025403784439,1.,0.866025403784439,1.,0.866025403784439,1.,0.866025403784439,
1.,0.866025403784439,1.,0.866025403784439,1.,0.866025403784439,1.,0.866025403784439,
1.,0.866025403784439,1.,0.866025403784439,1.,0.866025403784439,1.,0.866025403784439,
1.,0.866025403784439,1.,0.866025403784439,1.,0.866025403784439,1.,0.866025403784439,
1.,0.866025403784439,1.,0.866025403784439,1.,0.866025403784439,1.,0.866025403784439,
1.,0.866025403784439,1.,0.866025403784439,1.,0.866025403784439,1.,0.866025403784439,
1.,0.866025403784439,1.,0.866025403784439,1.,0.866025403784439,1.,0.866025403784439,
1.,0.866025403784439,1.,0.866025403784439,1.,0.866025403784439,1.,0.866025403784439,
1.,0.866025403784439,1.,0.866025403784439,1.,0.866025403784439,1.,0.866025403784439,
1.,0.866025403784439,1.,0.866025403784439,1.,0.866025403784439,1.,0.866025403784439,
1.,0.866025403784439,1.,0.866025403784439,1.,0.866025403784439,1.,0.866025403784439,
1.,0.866025403784439,1.,0.866025403784439,1.,0.866025403784439,1.,0.866025403784439,
1.,0.866025403784439,1.,0.866025403784439,1.,0.866025403784439,1.,0.866025403784439,
1.,0.866025403784439,1.,0.866025403784439,1.,0.866025403784439,1.,0.866025403784439,
1.,0.866025403784439,1.,0.866025403784439,1.,0.866025403784439,1.,0.866025403784439,
1.,0.866025403784439,1.,0.866025403784439,1.,0.866025403784439,1.,0.866025403784439,
1.,0.866025403784439,1.,0.866025403784439,1.,0.866025403784439,1.,0.866025403784439,
1.,0.866025403784439,1.,0.866025403784439,1.,0.866025403784439,1.,0.866025403784439,
1.,0.866025403784439,1.,0.866025403784439,1.,0.866025403784439,1.,0.866025403784439,
1.,0.866025403784439,1.,0.866025403784439,1.,0.866025403784439,1.,0.866025403784439,
1.,0.866025403784439,1.,0.866025403784439,1.,0.866025403784439,1.,0.866025403784439,
1.,0.866025403784439,1.,0.866025403784439,1.,0.866025403784439,1.,0.866025403784439,
1.,0.866025403784439,1.,0.866025403784439,1.,0.866025403784439,1.,0.866025403784439,
1.,0.866025403784439,1.,0.866025403784439,1.,0.866025403784439,1.,0.866025403784439,
1.,0.866025403784439,1.,0.866025403784439,1.,0.866025403784439,1.,0.866025403784439,
1.,0.866025403784439,1.,0.866025403784439,1.,0.866025403784439,1.,0.866025403784439,
1.,0.866025403784439,1.,0.866025403784439,1.,0.866025403784439,1.,0.866025403784439,
1.,0.866025403784439,1.,0.866025403784439,1.,0.866025403784439,1.,0.866025403784439,
1.,0.866025403784439,1.,0.866025403784439,1.,0.866025403784439,1.,0.866025403784439,
1.,0.866025403784439,1.,0.866025403784439,1.,0.866025403784439,1.,0.866025403784439,
1.,0.866025403784439,1.,0.866025403784439,1.,0.866025403784439,1.,0.866025403784439,
1.,0.866025403784439,1.,0.866025403784439,1.,0.866025403784439,1.,0.866025403784439,
1.,0.866025403784439,1.,0.866025403784439,1.,0.866025403784439,1.,0.866025403784439,
1.,0.866025403784439,1.,0.866025403784439,1.,0.866025403784439,1.,0.866025403784439,
1.,0.866025403784439,1.,0.866025403784439,1.,0.866025403784439,1.,0.866025403784439,
1.,0.866025403784439,1.,0.866025403784439,1.,0.866025403784439,1.,0.866025403784439,
1.,0.866025403784439,1.,0.866025403784439,1.,0.866025403784439,1.,0.866025403784439,
1.,0.866025403784439,1.,0.866025403784439,1.,0.866025403784439,1.,0.866025403784439,
1.,0.866025403784439,1.,0.866025403784439,1.,0.866025403784439,1.,0.866025403784439,
1.,0.866025403784439,1.,0.866025403784439,1.,0.866025403784439,1.,0.866025403784439,
1.,0.866025403784439,1.,0.866025403784439,1.,0.866025403784439,1.,0.866025403784439,
1.,0.866025403784439,1.,0.866025403784439,1.,0.866025403784439,1.,0.866025403784439,
1.,0.866025403784439,1.,0.866025403784439,1.,0.866025403784439,1.,0.866025403784439,
1.,0.866025403784439,1.,0.866025403784439,1.,0.866025403784439,1.,0.866025403784439,
1.,0.866025403784439,1.,0.866025403784439,1.,0.866025403784439,1.,0.866025403784439,
1.,0.866025403784439,1.,0.866025403784439,1.,0.866025403784439,1.,0.866025403784439,
1.,0.866025403784439,1.,0.866025403784439,1.,0.866025403784439,1.,0.866025403784439,
1.,0.866025403784439,1.,0.866025403784439,1.,0.866025403784439,1.,0.866025403784439,
1.,0.866025403784439,1.,0.866025403784439,1.,0.866025403784439,1.,0.866025403784439,
1.,0.866025403784439,1.,0.866025403784439,1.,0.866025403784439,1.,0.866025403784439,
1.,0.866025403784439,1.,0.866025403784439,1.,0.866025403784439,1.,0.866025403784439,
1.,0.866025403784439,1.,0.866025403784439,1.,0.866025403784439,1.,0.866025403784439,
1.,0.866025403784439,1.,0.866025403784439,1.,0.866025403784439,1.,0.866025403784439,
1.,0.866025403784439,1.,0.866025403784439,1.,0.866025403784439,1.,0.866025403784439,
1.,0.866025403784439,1.,0.866025403784439,1.,0.866025403784439,1.,0.866025403784439,
1.,0.866025403784439,1.,0.866025403784439,1.,0.866025403784439,1.,0.866025403784439,
1.,0.866025403784439,1.,0.866025403784439,1.,0.866025403784439,1.,0.866025403784439,
1.,0.866025403784439,1.,0.866025403784439,1.,0.866025403784439,1.,0.866025403784439,
1.,0.866025403784439,1.,0.866025403784439,1.,0.866025403784439,1.,0.866025403784439,
1.,0.866025403784439,1.,0.866025403784439,1.,0.866025403784439,1.,0.866025403784439,
1.,0.866025403784439,1.,0.866025403784439,1.,0.866025403784439,1.,0.866025403784439,
1.,0.866025403784439,1.,0.866025403784439,1.,0.866025403784439,1.,0.866025403784439,
1.,0.866025403784439,1.,0.866025403784439,1.,0.866025403784439,1.,0.866025403784439,
1.,0.866025403784439,1.,0.866025403784439,1.,0.866025403784439,1.,0.866025403784439,
1.,0.866025403784439,1.,0.866025403784439,1.,0.866025403784439,1.,0.866025403784439,
1.,0.866025403784439,1.,0.866025403784439,1.,0.866025403784439,1.,0.866025403784439,
1.,0.866025403784439,1.,0.866025403784439,1.,0.866025403784439,1.,0.866025403784439,
1.,0.866025403784439,1.,0.866025403784439,1.,0.866025403784439,1.,0.866025403784439,
1.,0.866025403784439,1.,0.866025403784439,1.,0.866025403784439,1.,0.866025403784439,
1.,0.866025403784439,1.,0.866025403784439,1.,0.866025403784439,1.,0.866025403784439,
1.,0.866025403784439,1.,0.866025403784439,1.,0.866025403784439,1.,0.866025403784439,
1.,0.866025403784439,1.,0.866025403784439,1.,0.866025403784439,1.,0.866025403784439,
1.,0.866025403784439,1.,0.866025403784439,1.,0.866025403784439,1.,0.866025403784439,
1.,0.866025403784439,1.,0.866025403784439,1.,0.866025403784439,1.,0.866025403784439,
1.,0.866025403784439,1.,0.866025403784439,1.,0.866025403784439,1.,0.866025403784439,
1.,0.866025403784439,1.,0.866025403784439,1.,0.866025403784439,1.,0.866025403784439,
1.,0.866025403784439,1.,0.866025403784439,1.,0.866025403784439,1.,0.866025403784439,
1.,0.866025403784439,1.,0.866025403784439,1.,0.866025403784439,1.,0.866025403784439,
1.,0.866025403784439,1.,0.866025403784439,1.,0.866025403784439,1.,0.866025403784439,
1.,0.866025403784439,1.,0.866025403784439,1.,0.866025403784439,1.,0.866025403784439,
1.,0.866025403784439,1.,0.866025403784439,1.,0.866025403784439,1.,0.866025403784439,
1.,0.866025403784439,1.,0.866025403784439,1.,0.866025403784439,1.,0.866025403784439,
1.,0.866025403784439,1.,0.866025403784439,1.,0.866025403784439,1.,0.866025403784439,
1.,0.866025403784439,1.,0.866025403784439,1.,0.866025403784439,1.,0.866025403784439,
1.,0.866025403784439,1.,0.866025403784439,1.,0.866025403784439,1.,0.866025403784439,
1.,0.866025403784439,1.,0.866025403784439,1.,0.866025403784439,1.,0.866025403784439,
1.,0.866025403784439,1.,0.866025403784439,1.,0.866025403784439,1.,0.866025403784439,
1.,0.866025403784439,1.,0.866025403784439,1.,0.866025403784439,1.,0.866025403784439,
1.,0.866025403784439,1.,0.866025403784439,1.,0.866025403784439,1.,0.866025403784439,
1.,0.866025403784439,1.,0.866025403784439,1.,0.866025403784439,1.,0.866025403784439,
1.,0.866025403784439,1.,0.866025403784439,1.,0.866025403784439,1.)))
REPRESENTATION_ITEM('')
SURFACE()
);
#151=(
BOUNDED_SURFACE()
B_SPLINE_SURFACE(3,2,((#21658,#21659,#21660,#21661,#21662,#21663,#21664,
#21665,#21666,#21667,#21668,#21669,#21670,#21671,#21672,#21673,#21674,#21675,
#21676,#21677,#21678,#21679,#21680,#21681,#21682,#21683,#21684,#21685,#21686,
#21687,#21688,#21689,#21690,#21691,#21692,#21693,#21694,#21695,#21696,#21697,
#21698,#21699,#21700,#21701,#21702,#21703,#21704,#21705,#21706,#21707,#21708,
#21709,#21710,#21711,#21712,#21713,#21714,#21715,#21716,#21717,#21718,#21719,
#21720,#21721,#21722,#21723,#21724,#21725,#21726,#21727,#21728,#21729,#21730,
#21731,#21732,#21733,#21734,#21735,#21736,#21737,#21738,#21739,#21740,#21741,
#21742,#21743,#21744,#21745,#21746,#21747,#21748,#21749,#21750,#21751,#21752,
#21753,#21754,#21755,#21756,#21757,#21758,#21759,#21760,#21761,#21762,#21763,
#21764,#21765,#21766,#21767,#21768,#21769,#21770,#21771,#21772,#21773,#21774,
#21775,#21776,#21777,#21778,#21779,#21780,#21781,#21782,#21783,#21784,#21785,
#21786,#21787,#21788,#21789,#21790,#21791,#21792,#21793,#21794,#21795,#21796,
#21797,#21798,#21799,#21800,#21801,#21802,#21803,#21804,#21805,#21806,#21807,
#21808,#21809,#21810,#21811,#21812,#21813,#21814,#21815,#21816,#21817,#21818,
#21819,#21820,#21821,#21822,#21823,#21824,#21825,#21826,#21827,#21828,#21829,
#21830,#21831,#21832,#21833,#21834,#21835,#21836,#21837,#21838,#21839,#21840,
#21841,#21842,#21843,#21844,#21845,#21846,#21847,#21848,#21849,#21850,#21851,
#21852,#21853,#21854,#21855,#21856,#21857,#21858,#21859,#21860,#21861,#21862,
#21863,#21864,#21865,#21866,#21867,#21868,#21869,#21870,#21871,#21872,#21873,
#21874,#21875,#21876,#21877,#21878,#21879,#21880,#21881,#21882,#21883,#21884,
#21885,#21886,#21887,#21888,#21889,#21890,#21891,#21892,#21893,#21894,#21895,
#21896,#21897,#21898,#21899,#21900,#21901,#21902,#21903,#21904,#21905,#21906,
#21907,#21908,#21909,#21910,#21911,#21912,#21913,#21914,#21915,#21916,#21917,
#21918,#21919,#21920,#21921,#21922,#21923,#21924,#21925,#21926,#21927,#21928,
#21929,#21930,#21931,#21932,#21933,#21934,#21935,#21936,#21937,#21938,#21939,
#21940,#21941,#21942,#21943,#21944,#21945,#21946,#21947,#21948,#21949,#21950,
#21951,#21952,#21953,#21954,#21955,#21956,#21957,#21958,#21959,#21960,#21961,
#21962,#21963,#21964,#21965,#21966,#21967,#21968,#21969,#21970,#21971,#21972,
#21973,#21974,#21975,#21976,#21977,#21978,#21979,#21980,#21981,#21982,#21983,
#21984,#21985,#21986,#21987,#21988,#21989,#21990,#21991,#21992,#21993,#21994,
#21995,#21996,#21997,#21998,#21999,#22000,#22001,#22002,#22003,#22004,#22005,
#22006,#22007,#22008,#22009,#22010,#22011,#22012,#22013,#22014,#22015,#22016,
#22017,#22018,#22019,#22020,#22021,#22022,#22023,#22024,#22025,#22026,#22027,
#22028,#22029,#22030,#22031,#22032,#22033,#22034,#22035,#22036,#22037,#22038,
#22039,#22040,#22041,#22042,#22043,#22044,#22045,#22046,#22047,#22048,#22049,
#22050,#22051,#22052,#22053,#22054,#22055,#22056,#22057,#22058,#22059,#22060,
#22061,#22062,#22063,#22064,#22065,#22066,#22067,#22068,#22069,#22070,#22071,
#22072,#22073,#22074,#22075,#22076,#22077,#22078,#22079,#22080,#22081,#22082,
#22083,#22084,#22085,#22086,#22087,#22088,#22089,#22090,#22091,#22092,#22093,
#22094,#22095,#22096,#22097,#22098,#22099,#22100,#22101,#22102,#22103,#22104,
#22105,#22106,#22107,#22108,#22109,#22110,#22111,#22112,#22113,#22114,#22115,
#22116,#22117,#22118,#22119,#22120,#22121,#22122,#22123,#22124,#22125,#22126,
#22127,#22128,#22129,#22130,#22131,#22132,#22133,#22134,#22135,#22136,#22137,
#22138,#22139,#22140,#22141,#22142,#22143,#22144,#22145,#22146,#22147,#22148,
#22149,#22150,#22151,#22152,#22153,#22154,#22155,#22156,#22157,#22158,#22159,
#22160,#22161,#22162,#22163,#22164,#22165,#22166,#22167,#22168,#22169,#22170,
#22171,#22172,#22173,#22174,#22175,#22176,#22177,#22178,#22179,#22180,#22181,
#22182,#22183,#22184,#22185,#22186,#22187,#22188,#22189,#22190,#22191,#22192,
#22193,#22194,#22195,#22196,#22197,#22198,#22199,#22200,#22201,#22202,#22203,
#22204,#22205,#22206,#22207,#22208,#22209,#22210,#22211,#22212,#22213,#22214,
#22215,#22216,#22217,#22218,#22219,#22220,#22221,#22222,#22223,#22224,#22225,
#22226,#22227,#22228,#22229,#22230,#22231,#22232,#22233,#22234,#22235,#22236,
#22237,#22238,#22239,#22240,#22241,#22242,#22243,#22244,#22245,#22246,#22247,
#22248,#22249,#22250,#22251,#22252,#22253,#22254,#22255,#22256,#22257,#22258,
#22259,#22260,#22261,#22262,#22263,#22264,#22265,#22266,#22267,#22268,#22269,
#22270,#22271,#22272,#22273,#22274,#22275,#22276,#22277,#22278,#22279,#22280,
#22281,#22282,#22283,#22284,#22285,#22286,#22287,#22288,#22289,#22290,#22291,
#22292,#22293,#22294,#22295,#22296,#22297,#22298,#22299,#22300,#22301,#22302,
#22303,#22304,#22305,#22306,#22307,#22308,#22309,#22310,#22311,#22312,#22313,
#22314,#22315,#22316,#22317,#22318,#22319,#22320,#22321,#22322,#22323,#22324,
#22325,#22326,#22327,#22328,#22329,#22330,#22331,#22332,#22333,#22334,#22335,
#22336,#22337,#22338,#22339,#22340,#22341,#22342,#22343,#22344,#22345,#22346,
#22347,#22348,#22349,#22350,#22351,#22352,#22353,#22354,#22355,#22356,#22357,
#22358,#22359,#22360,#22361,#22362,#22363,#22364,#22365,#22366,#22367,#22368,
#22369,#22370,#22371,#22372,#22373,#22374,#22375,#22376,#22377,#22378,#22379,
#22380,#22381,#22382,#22383,#22384,#22385,#22386,#22387,#22388,#22389,#22390,
#22391,#22392,#22393,#22394,#22395,#22396,#22397,#22398,#22399,#22400,#22401,
#22402,#22403,#22404,#22405,#22406,#22407,#22408,#22409,#22410,#22411,#22412,
#22413,#22414,#22415,#22416,#22417,#22418,#22419,#22420,#22421,#22422,#22423,
#22424,#22425,#22426,#22427,#22428,#22429,#22430,#22431,#22432,#22433,#22434,
#22435,#22436,#22437,#22438,#22439,#22440,#22441,#22442,#22443,#22444,#22445,
#22446,#22447,#22448,#22449,#22450,#22451,#22452,#22453,#22454,#22455,#22456,
#22457,#22458,#22459,#22460,#22461,#22462,#22463,#22464,#22465,#22466,#22467,
#22468,#22469,#22470,#22471,#22472,#22473,#22474,#22475,#22476,#22477,#22478,
#22479,#22480,#22481,#22482,#22483,#22484,#22485,#22486,#22487,#22488,#22489,
#22490,#22491,#22492,#22493,#22494,#22495,#22496,#22497,#22498,#22499,#22500,
#22501,#22502,#22503,#22504,#22505,#22506,#22507,#22508,#22509,#22510,#22511,
#22512,#22513,#22514,#22515,#22516,#22517,#22518,#22519,#22520,#22521,#22522,
#22523,#22524,#22525,#22526,#22527,#22528,#22529,#22530,#22531,#22532,#22533,
#22534,#22535,#22536,#22537,#22538,#22539,#22540,#22541,#22542,#22543,#22544,
#22545,#22546,#22547,#22548,#22549,#22550,#22551,#22552,#22553,#22554,#22555,
#22556,#22557,#22558,#22559,#22560,#22561,#22562,#22563,#22564,#22565,#22566,
#22567,#22568,#22569,#22570,#22571,#22572,#22573,#22574,#22575,#22576,#22577,
#22578,#22579,#22580,#22581,#22582,#22583,#22584,#22585,#22586,#22587,#22588,
#22589,#22590,#22591,#22592,#22593,#22594,#22595,#22596,#22597,#22598,#22599,
#22600,#22601,#22602,#22603,#22604,#22605,#22606,#22607,#22608,#22609,#22610,
#22611,#22612,#22613,#22614,#22615,#22616,#22617,#22618,#22619,#22620,#22621,
#22622,#22623,#22624,#22625,#22626,#22627,#22628,#22629,#22630),(#22631,
#22632,#22633,#22634,#22635,#22636,#22637,#22638,#22639,#22640,#22641,#22642,
#22643,#22644,#22645,#22646,#22647,#22648,#22649,#22650,#22651,#22652,#22653,
#22654,#22655,#22656,#22657,#22658,#22659,#22660,#22661,#22662,#22663,#22664,
#22665,#22666,#22667,#22668,#22669,#22670,#22671,#22672,#22673,#22674,#22675,
#22676,#22677,#22678,#22679,#22680,#22681,#22682,#22683,#22684,#22685,#22686,
#22687,#22688,#22689,#22690,#22691,#22692,#22693,#22694,#22695,#22696,#22697,
#22698,#22699,#22700,#22701,#22702,#22703,#22704,#22705,#22706,#22707,#22708,
#22709,#22710,#22711,#22712,#22713,#22714,#22715,#22716,#22717,#22718,#22719,
#22720,#22721,#22722,#22723,#22724,#22725,#22726,#22727,#22728,#22729,#22730,
#22731,#22732,#22733,#22734,#22735,#22736,#22737,#22738,#22739,#22740,#22741,
#22742,#22743,#22744,#22745,#22746,#22747,#22748,#22749,#22750,#22751,#22752,
#22753,#22754,#22755,#22756,#22757,#22758,#22759,#22760,#22761,#22762,#22763,
#22764,#22765,#22766,#22767,#22768,#22769,#22770,#22771,#22772,#22773,#22774,
#22775,#22776,#22777,#22778,#22779,#22780,#22781,#22782,#22783,#22784,#22785,
#22786,#22787,#22788,#22789,#22790,#22791,#22792,#22793,#22794,#22795,#22796,
#22797,#22798,#22799,#22800,#22801,#22802,#22803,#22804,#22805,#22806,#22807,
#22808,#22809,#22810,#22811,#22812,#22813,#22814,#22815,#22816,#22817,#22818,
#22819,#22820,#22821,#22822,#22823,#22824,#22825,#22826,#22827,#22828,#22829,
#22830,#22831,#22832,#22833,#22834,#22835,#22836,#22837,#22838,#22839,#22840,
#22841,#22842,#22843,#22844,#22845,#22846,#22847,#22848,#22849,#22850,#22851,
#22852,#22853,#22854,#22855,#22856,#22857,#22858,#22859,#22860,#22861,#22862,
#22863,#22864,#22865,#22866,#22867,#22868,#22869,#22870,#22871,#22872,#22873,
#22874,#22875,#22876,#22877,#22878,#22879,#22880,#22881,#22882,#22883,#22884,
#22885,#22886,#22887,#22888,#22889,#22890,#22891,#22892,#22893,#22894,#22895,
#22896,#22897,#22898,#22899,#22900,#22901,#22902,#22903,#22904,#22905,#22906,
#22907,#22908,#22909,#22910,#22911,#22912,#22913,#22914,#22915,#22916,#22917,
#22918,#22919,#22920,#22921,#22922,#22923,#22924,#22925,#22926,#22927,#22928,
#22929,#22930,#22931,#22932,#22933,#22934,#22935,#22936,#22937,#22938,#22939,
#22940,#22941,#22942,#22943,#22944,#22945,#22946,#22947,#22948,#22949,#22950,
#22951,#22952,#22953,#22954,#22955,#22956,#22957,#22958,#22959,#22960,#22961,
#22962,#22963,#22964,#22965,#22966,#22967,#22968,#22969,#22970,#22971,#22972,
#22973,#22974,#22975,#22976,#22977,#22978,#22979,#22980,#22981,#22982,#22983,
#22984,#22985,#22986,#22987,#22988,#22989,#22990,#22991,#22992,#22993,#22994,
#22995,#22996,#22997,#22998,#22999,#23000,#23001,#23002,#23003,#23004,#23005,
#23006,#23007,#23008,#23009,#23010,#23011,#23012,#23013,#23014,#23015,#23016,
#23017,#23018,#23019,#23020,#23021,#23022,#23023,#23024,#23025,#23026,#23027,
#23028,#23029,#23030,#23031,#23032,#23033,#23034,#23035,#23036,#23037,#23038,
#23039,#23040,#23041,#23042,#23043,#23044,#23045,#23046,#23047,#23048,#23049,
#23050,#23051,#23052,#23053,#23054,#23055,#23056,#23057,#23058,#23059,#23060,
#23061,#23062,#23063,#23064,#23065,#23066,#23067,#23068,#23069,#23070,#23071,
#23072,#23073,#23074,#23075,#23076,#23077,#23078,#23079,#23080,#23081,#23082,
#23083,#23084,#23085,#23086,#23087,#23088,#23089,#23090,#23091,#23092,#23093,
#23094,#23095,#23096,#23097,#23098,#23099,#23100,#23101,#23102,#23103,#23104,
#23105,#23106,#23107,#23108,#23109,#23110,#23111,#23112,#23113,#23114,#23115,
#23116,#23117,#23118,#23119,#23120,#23121,#23122,#23123,#23124,#23125,#23126,
#23127,#23128,#23129,#23130,#23131,#23132,#23133,#23134,#23135,#23136,#23137,
#23138,#23139,#23140,#23141,#23142,#23143,#23144,#23145,#23146,#23147,#23148,
#23149,#23150,#23151,#23152,#23153,#23154,#23155,#23156,#23157,#23158,#23159,
#23160,#23161,#23162,#23163,#23164,#23165,#23166,#23167,#23168,#23169,#23170,
#23171,#23172,#23173,#23174,#23175,#23176,#23177,#23178,#23179,#23180,#23181,
#23182,#23183,#23184,#23185,#23186,#23187,#23188,#23189,#23190,#23191,#23192,
#23193,#23194,#23195,#23196,#23197,#23198,#23199,#23200,#23201,#23202,#23203,
#23204,#23205,#23206,#23207,#23208,#23209,#23210,#23211,#23212,#23213,#23214,
#23215,#23216,#23217,#23218,#23219,#23220,#23221,#23222,#23223,#23224,#23225,
#23226,#23227,#23228,#23229,#23230,#23231,#23232,#23233,#23234,#23235,#23236,
#23237,#23238,#23239,#23240,#23241,#23242,#23243,#23244,#23245,#23246,#23247,
#23248,#23249,#23250,#23251,#23252,#23253,#23254,#23255,#23256,#23257,#23258,
#23259,#23260,#23261,#23262,#23263,#23264,#23265,#23266,#23267,#23268,#23269,
#23270,#23271,#23272,#23273,#23274,#23275,#23276,#23277,#23278,#23279,#23280,
#23281,#23282,#23283,#23284,#23285,#23286,#23287,#23288,#23289,#23290,#23291,
#23292,#23293,#23294,#23295,#23296,#23297,#23298,#23299,#23300,#23301,#23302,
#23303,#23304,#23305,#23306,#23307,#23308,#23309,#23310,#23311,#23312,#23313,
#23314,#23315,#23316,#23317,#23318,#23319,#23320,#23321,#23322,#23323,#23324,
#23325,#23326,#23327,#23328,#23329,#23330,#23331,#23332,#23333,#23334,#23335,
#23336,#23337,#23338,#23339,#23340,#23341,#23342,#23343,#23344,#23345,#23346,
#23347,#23348,#23349,#23350,#23351,#23352,#23353,#23354,#23355,#23356,#23357,
#23358,#23359,#23360,#23361,#23362,#23363,#23364,#23365,#23366,#23367,#23368,
#23369,#23370,#23371,#23372,#23373,#23374,#23375,#23376,#23377,#23378,#23379,
#23380,#23381,#23382,#23383,#23384,#23385,#23386,#23387,#23388,#23389,#23390,
#23391,#23392,#23393,#23394,#23395,#23396,#23397,#23398,#23399,#23400,#23401,
#23402,#23403,#23404,#23405,#23406,#23407,#23408,#23409,#23410,#23411,#23412,
#23413,#23414,#23415,#23416,#23417,#23418,#23419,#23420,#23421,#23422,#23423,
#23424,#23425,#23426,#23427,#23428,#23429,#23430,#23431,#23432,#23433,#23434,
#23435,#23436,#23437,#23438,#23439,#23440,#23441,#23442,#23443,#23444,#23445,
#23446,#23447,#23448,#23449,#23450,#23451,#23452,#23453,#23454,#23455,#23456,
#23457,#23458,#23459,#23460,#23461,#23462,#23463,#23464,#23465,#23466,#23467,
#23468,#23469,#23470,#23471,#23472,#23473,#23474,#23475,#23476,#23477,#23478,
#23479,#23480,#23481,#23482,#23483,#23484,#23485,#23486,#23487,#23488,#23489,
#23490,#23491,#23492,#23493,#23494,#23495,#23496,#23497,#23498,#23499,#23500,
#23501,#23502,#23503,#23504,#23505,#23506,#23507,#23508,#23509,#23510,#23511,
#23512,#23513,#23514,#23515,#23516,#23517,#23518,#23519,#23520,#23521,#23522,
#23523,#23524,#23525,#23526,#23527,#23528,#23529,#23530,#23531,#23532,#23533,
#23534,#23535,#23536,#23537,#23538,#23539,#23540,#23541,#23542,#23543,#23544,
#23545,#23546,#23547,#23548,#23549,#23550,#23551,#23552,#23553,#23554,#23555,
#23556,#23557,#23558,#23559,#23560,#23561,#23562,#23563,#23564,#23565,#23566,
#23567,#23568,#23569,#23570,#23571,#23572,#23573,#23574,#23575,#23576,#23577,
#23578,#23579,#23580,#23581,#23582,#23583,#23584,#23585,#23586,#23587,#23588,
#23589,#23590,#23591,#23592,#23593,#23594,#23595,#23596,#23597,#23598,#23599,
#23600,#23601,#23602,#23603),(#23604,#23605,#23606,#23607,#23608,#23609,
#23610,#23611,#23612,#23613,#23614,#23615,#23616,#23617,#23618,#23619,#23620,
#23621,#23622,#23623,#23624,#23625,#23626,#23627,#23628,#23629,#23630,#23631,
#23632,#23633,#23634,#23635,#23636,#23637,#23638,#23639,#23640,#23641,#23642,
#23643,#23644,#23645,#23646,#23647,#23648,#23649,#23650,#23651,#23652,#23653,
#23654,#23655,#23656,#23657,#23658,#23659,#23660,#23661,#23662,#23663,#23664,
#23665,#23666,#23667,#23668,#23669,#23670,#23671,#23672,#23673,#23674,#23675,
#23676,#23677,#23678,#23679,#23680,#23681,#23682,#23683,#23684,#23685,#23686,
#23687,#23688,#23689,#23690,#23691,#23692,#23693,#23694,#23695,#23696,#23697,
#23698,#23699,#23700,#23701,#23702,#23703,#23704,#23705,#23706,#23707,#23708,
#23709,#23710,#23711,#23712,#23713,#23714,#23715,#23716,#23717,#23718,#23719,
#23720,#23721,#23722,#23723,#23724,#23725,#23726,#23727,#23728,#23729,#23730,
#23731,#23732,#23733,#23734,#23735,#23736,#23737,#23738,#23739,#23740,#23741,
#23742,#23743,#23744,#23745,#23746,#23747,#23748,#23749,#23750,#23751,#23752,
#23753,#23754,#23755,#23756,#23757,#23758,#23759,#23760,#23761,#23762,#23763,
#23764,#23765,#23766,#23767,#23768,#23769,#23770,#23771,#23772,#23773,#23774,
#23775,#23776,#23777,#23778,#23779,#23780,#23781,#23782,#23783,#23784,#23785,
#23786,#23787,#23788,#23789,#23790,#23791,#23792,#23793,#23794,#23795,#23796,
#23797,#23798,#23799,#23800,#23801,#23802,#23803,#23804,#23805,#23806,#23807,
#23808,#23809,#23810,#23811,#23812,#23813,#23814,#23815,#23816,#23817,#23818,
#23819,#23820,#23821,#23822,#23823,#23824,#23825,#23826,#23827,#23828,#23829,
#23830,#23831,#23832,#23833,#23834,#23835,#23836,#23837,#23838,#23839,#23840,
#23841,#23842,#23843,#23844,#23845,#23846,#23847,#23848,#23849,#23850,#23851,
#23852,#23853,#23854,#23855,#23856,#23857,#23858,#23859,#23860,#23861,#23862,
#23863,#23864,#23865,#23866,#23867,#23868,#23869,#23870,#23871,#23872,#23873,
#23874,#23875,#23876,#23877,#23878,#23879,#23880,#23881,#23882,#23883,#23884,
#23885,#23886,#23887,#23888,#23889,#23890,#23891,#23892,#23893,#23894,#23895,
#23896,#23897,#23898,#23899,#23900,#23901,#23902,#23903,#23904,#23905,#23906,
#23907,#23908,#23909,#23910,#23911,#23912,#23913,#23914,#23915,#23916,#23917,
#23918,#23919,#23920,#23921,#23922,#23923,#23924,#23925,#23926,#23927,#23928,
#23929,#23930,#23931,#23932,#23933,#23934,#23935,#23936,#23937,#23938,#23939,
#23940,#23941,#23942,#23943,#23944,#23945,#23946,#23947,#23948,#23949,#23950,
#23951,#23952,#23953,#23954,#23955,#23956,#23957,#23958,#23959,#23960,#23961,
#23962,#23963,#23964,#23965,#23966,#23967,#23968,#23969,#23970,#23971,#23972,
#23973,#23974,#23975,#23976,#23977,#23978,#23979,#23980,#23981,#23982,#23983,
#23984,#23985,#23986,#23987,#23988,#23989,#23990,#23991,#23992,#23993,#23994,
#23995,#23996,#23997,#23998,#23999,#24000,#24001,#24002,#24003,#24004,#24005,
#24006,#24007,#24008,#24009,#24010,#24011,#24012,#24013,#24014,#24015,#24016,
#24017,#24018,#24019,#24020,#24021,#24022,#24023,#24024,#24025,#24026,#24027,
#24028,#24029,#24030,#24031,#24032,#24033,#24034,#24035,#24036,#24037,#24038,
#24039,#24040,#24041,#24042,#24043,#24044,#24045,#24046,#24047,#24048,#24049,
#24050,#24051,#24052,#24053,#24054,#24055,#24056,#24057,#24058,#24059,#24060,
#24061,#24062,#24063,#24064,#24065,#24066,#24067,#24068,#24069,#24070,#24071,
#24072,#24073,#24074,#24075,#24076,#24077,#24078,#24079,#24080,#24081,#24082,
#24083,#24084,#24085,#24086,#24087,#24088,#24089,#24090,#24091,#24092,#24093,
#24094,#24095,#24096,#24097,#24098,#24099,#24100,#24101,#24102,#24103,#24104,
#24105,#24106,#24107,#24108,#24109,#24110,#24111,#24112,#24113,#24114,#24115,
#24116,#24117,#24118,#24119,#24120,#24121,#24122,#24123,#24124,#24125,#24126,
#24127,#24128,#24129,#24130,#24131,#24132,#24133,#24134,#24135,#24136,#24137,
#24138,#24139,#24140,#24141,#24142,#24143,#24144,#24145,#24146,#24147,#24148,
#24149,#24150,#24151,#24152,#24153,#24154,#24155,#24156,#24157,#24158,#24159,
#24160,#24161,#24162,#24163,#24164,#24165,#24166,#24167,#24168,#24169,#24170,
#24171,#24172,#24173,#24174,#24175,#24176,#24177,#24178,#24179,#24180,#24181,
#24182,#24183,#24184,#24185,#24186,#24187,#24188,#24189,#24190,#24191,#24192,
#24193,#24194,#24195,#24196,#24197,#24198,#24199,#24200,#24201,#24202,#24203,
#24204,#24205,#24206,#24207,#24208,#24209,#24210,#24211,#24212,#24213,#24214,
#24215,#24216,#24217,#24218,#24219,#24220,#24221,#24222,#24223,#24224,#24225,
#24226,#24227,#24228,#24229,#24230,#24231,#24232,#24233,#24234,#24235,#24236,
#24237,#24238,#24239,#24240,#24241,#24242,#24243,#24244,#24245,#24246,#24247,
#24248,#24249,#24250,#24251,#24252,#24253,#24254,#24255,#24256,#24257,#24258,
#24259,#24260,#24261,#24262,#24263,#24264,#24265,#24266,#24267,#24268,#24269,
#24270,#24271,#24272,#24273,#24274,#24275,#24276,#24277,#24278,#24279,#24280,
#24281,#24282,#24283,#24284,#24285,#24286,#24287,#24288,#24289,#24290,#24291,
#24292,#24293,#24294,#24295,#24296,#24297,#24298,#24299,#24300,#24301,#24302,
#24303,#24304,#24305,#24306,#24307,#24308,#24309,#24310,#24311,#24312,#24313,
#24314,#24315,#24316,#24317,#24318,#24319,#24320,#24321,#24322,#24323,#24324,
#24325,#24326,#24327,#24328,#24329,#24330,#24331,#24332,#24333,#24334,#24335,
#24336,#24337,#24338,#24339,#24340,#24341,#24342,#24343,#24344,#24345,#24346,
#24347,#24348,#24349,#24350,#24351,#24352,#24353,#24354,#24355,#24356,#24357,
#24358,#24359,#24360,#24361,#24362,#24363,#24364,#24365,#24366,#24367,#24368,
#24369,#24370,#24371,#24372,#24373,#24374,#24375,#24376,#24377,#24378,#24379,
#24380,#24381,#24382,#24383,#24384,#24385,#24386,#24387,#24388,#24389,#24390,
#24391,#24392,#24393,#24394,#24395,#24396,#24397,#24398,#24399,#24400,#24401,
#24402,#24403,#24404,#24405,#24406,#24407,#24408,#24409,#24410,#24411,#24412,
#24413,#24414,#24415,#24416,#24417,#24418,#24419,#24420,#24421,#24422,#24423,
#24424,#24425,#24426,#24427,#24428,#24429,#24430,#24431,#24432,#24433,#24434,
#24435,#24436,#24437,#24438,#24439,#24440,#24441,#24442,#24443,#24444,#24445,
#24446,#24447,#24448,#24449,#24450,#24451,#24452,#24453,#24454,#24455,#24456,
#24457,#24458,#24459,#24460,#24461,#24462,#24463,#24464,#24465,#24466,#24467,
#24468,#24469,#24470,#24471,#24472,#24473,#24474,#24475,#24476,#24477,#24478,
#24479,#24480,#24481,#24482,#24483,#24484,#24485,#24486,#24487,#24488,#24489,
#24490,#24491,#24492,#24493,#24494,#24495,#24496,#24497,#24498,#24499,#24500,
#24501,#24502,#24503,#24504,#24505,#24506,#24507,#24508,#24509,#24510,#24511,
#24512,#24513,#24514,#24515,#24516,#24517,#24518,#24519,#24520,#24521,#24522,
#24523,#24524,#24525,#24526,#24527,#24528,#24529,#24530,#24531,#24532,#24533,
#24534,#24535,#24536,#24537,#24538,#24539,#24540,#24541,#24542,#24543,#24544,
#24545,#24546,#24547,#24548,#24549,#24550,#24551,#24552,#24553,#24554,#24555,
#24556,#24557,#24558,#24559,#24560,#24561,#24562,#24563,#24564,#24565,#24566,
#24567,#24568,#24569,#24570,#24571,#24572,#24573,#24574,#24575,#24576),
(#24577,#24578,#24579,#24580,#24581,#24582,#24583,#24584,#24585,#24586,
#24587,#24588,#24589,#24590,#24591,#24592,#24593,#24594,#24595,#24596,#24597,
#24598,#24599,#24600,#24601,#24602,#24603,#24604,#24605,#24606,#24607,#24608,
#24609,#24610,#24611,#24612,#24613,#24614,#24615,#24616,#24617,#24618,#24619,
#24620,#24621,#24622,#24623,#24624,#24625,#24626,#24627,#24628,#24629,#24630,
#24631,#24632,#24633,#24634,#24635,#24636,#24637,#24638,#24639,#24640,#24641,
#24642,#24643,#24644,#24645,#24646,#24647,#24648,#24649,#24650,#24651,#24652,
#24653,#24654,#24655,#24656,#24657,#24658,#24659,#24660,#24661,#24662,#24663,
#24664,#24665,#24666,#24667,#24668,#24669,#24670,#24671,#24672,#24673,#24674,
#24675,#24676,#24677,#24678,#24679,#24680,#24681,#24682,#24683,#24684,#24685,
#24686,#24687,#24688,#24689,#24690,#24691,#24692,#24693,#24694,#24695,#24696,
#24697,#24698,#24699,#24700,#24701,#24702,#24703,#24704,#24705,#24706,#24707,
#24708,#24709,#24710,#24711,#24712,#24713,#24714,#24715,#24716,#24717,#24718,
#24719,#24720,#24721,#24722,#24723,#24724,#24725,#24726,#24727,#24728,#24729,
#24730,#24731,#24732,#24733,#24734,#24735,#24736,#24737,#24738,#24739,#24740,
#24741,#24742,#24743,#24744,#24745,#24746,#24747,#24748,#24749,#24750,#24751,
#24752,#24753,#24754,#24755,#24756,#24757,#24758,#24759,#24760,#24761,#24762,
#24763,#24764,#24765,#24766,#24767,#24768,#24769,#24770,#24771,#24772,#24773,
#24774,#24775,#24776,#24777,#24778,#24779,#24780,#24781,#24782,#24783,#24784,
#24785,#24786,#24787,#24788,#24789,#24790,#24791,#24792,#24793,#24794,#24795,
#24796,#24797,#24798,#24799,#24800,#24801,#24802,#24803,#24804,#24805,#24806,
#24807,#24808,#24809,#24810,#24811,#24812,#24813,#24814,#24815,#24816,#24817,
#24818,#24819,#24820,#24821,#24822,#24823,#24824,#24825,#24826,#24827,#24828,
#24829,#24830,#24831,#24832,#24833,#24834,#24835,#24836,#24837,#24838,#24839,
#24840,#24841,#24842,#24843,#24844,#24845,#24846,#24847,#24848,#24849,#24850,
#24851,#24852,#24853,#24854,#24855,#24856,#24857,#24858,#24859,#24860,#24861,
#24862,#24863,#24864,#24865,#24866,#24867,#24868,#24869,#24870,#24871,#24872,
#24873,#24874,#24875,#24876,#24877,#24878,#24879,#24880,#24881,#24882,#24883,
#24884,#24885,#24886,#24887,#24888,#24889,#24890,#24891,#24892,#24893,#24894,
#24895,#24896,#24897,#24898,#24899,#24900,#24901,#24902,#24903,#24904,#24905,
#24906,#24907,#24908,#24909,#24910,#24911,#24912,#24913,#24914,#24915,#24916,
#24917,#24918,#24919,#24920,#24921,#24922,#24923,#24924,#24925,#24926,#24927,
#24928,#24929,#24930,#24931,#24932,#24933,#24934,#24935,#24936,#24937,#24938,
#24939,#24940,#24941,#24942,#24943,#24944,#24945,#24946,#24947,#24948,#24949,
#24950,#24951,#24952,#24953,#24954,#24955,#24956,#24957,#24958,#24959,#24960,
#24961,#24962,#24963,#24964,#24965,#24966,#24967,#24968,#24969,#24970,#24971,
#24972,#24973,#24974,#24975,#24976,#24977,#24978,#24979,#24980,#24981,#24982,
#24983,#24984,#24985,#24986,#24987,#24988,#24989,#24990,#24991,#24992,#24993,
#24994,#24995,#24996,#24997,#24998,#24999,#25000,#25001,#25002,#25003,#25004,
#25005,#25006,#25007,#25008,#25009,#25010,#25011,#25012,#25013,#25014,#25015,
#25016,#25017,#25018,#25019,#25020,#25021,#25022,#25023,#25024,#25025,#25026,
#25027,#25028,#25029,#25030,#25031,#25032,#25033,#25034,#25035,#25036,#25037,
#25038,#25039,#25040,#25041,#25042,#25043,#25044,#25045,#25046,#25047,#25048,
#25049,#25050,#25051,#25052,#25053,#25054,#25055,#25056,#25057,#25058,#25059,
#25060,#25061,#25062,#25063,#25064,#25065,#25066,#25067,#25068,#25069,#25070,
#25071,#25072,#25073,#25074,#25075,#25076,#25077,#25078,#25079,#25080,#25081,
#25082,#25083,#25084,#25085,#25086,#25087,#25088,#25089,#25090,#25091,#25092,
#25093,#25094,#25095,#25096,#25097,#25098,#25099,#25100,#25101,#25102,#25103,
#25104,#25105,#25106,#25107,#25108,#25109,#25110,#25111,#25112,#25113,#25114,
#25115,#25116,#25117,#25118,#25119,#25120,#25121,#25122,#25123,#25124,#25125,
#25126,#25127,#25128,#25129,#25130,#25131,#25132,#25133,#25134,#25135,#25136,
#25137,#25138,#25139,#25140,#25141,#25142,#25143,#25144,#25145,#25146,#25147,
#25148,#25149,#25150,#25151,#25152,#25153,#25154,#25155,#25156,#25157,#25158,
#25159,#25160,#25161,#25162,#25163,#25164,#25165,#25166,#25167,#25168,#25169,
#25170,#25171,#25172,#25173,#25174,#25175,#25176,#25177,#25178,#25179,#25180,
#25181,#25182,#25183,#25184,#25185,#25186,#25187,#25188,#25189,#25190,#25191,
#25192,#25193,#25194,#25195,#25196,#25197,#25198,#25199,#25200,#25201,#25202,
#25203,#25204,#25205,#25206,#25207,#25208,#25209,#25210,#25211,#25212,#25213,
#25214,#25215,#25216,#25217,#25218,#25219,#25220,#25221,#25222,#25223,#25224,
#25225,#25226,#25227,#25228,#25229,#25230,#25231,#25232,#25233,#25234,#25235,
#25236,#25237,#25238,#25239,#25240,#25241,#25242,#25243,#25244,#25245,#25246,
#25247,#25248,#25249,#25250,#25251,#25252,#25253,#25254,#25255,#25256,#25257,
#25258,#25259,#25260,#25261,#25262,#25263,#25264,#25265,#25266,#25267,#25268,
#25269,#25270,#25271,#25272,#25273,#25274,#25275,#25276,#25277,#25278,#25279,
#25280,#25281,#25282,#25283,#25284,#25285,#25286,#25287,#25288,#25289,#25290,
#25291,#25292,#25293,#25294,#25295,#25296,#25297,#25298,#25299,#25300,#25301,
#25302,#25303,#25304,#25305,#25306,#25307,#25308,#25309,#25310,#25311,#25312,
#25313,#25314,#25315,#25316,#25317,#25318,#25319,#25320,#25321,#25322,#25323,
#25324,#25325,#25326,#25327,#25328,#25329,#25330,#25331,#25332,#25333,#25334,
#25335,#25336,#25337,#25338,#25339,#25340,#25341,#25342,#25343,#25344,#25345,
#25346,#25347,#25348,#25349,#25350,#25351,#25352,#25353,#25354,#25355,#25356,
#25357,#25358,#25359,#25360,#25361,#25362,#25363,#25364,#25365,#25366,#25367,
#25368,#25369,#25370,#25371,#25372,#25373,#25374,#25375,#25376,#25377,#25378,
#25379,#25380,#25381,#25382,#25383,#25384,#25385,#25386,#25387,#25388,#25389,
#25390,#25391,#25392,#25393,#25394,#25395,#25396,#25397,#25398,#25399,#25400,
#25401,#25402,#25403,#25404,#25405,#25406,#25407,#25408,#25409,#25410,#25411,
#25412,#25413,#25414,#25415,#25416,#25417,#25418,#25419,#25420,#25421,#25422,
#25423,#25424,#25425,#25426,#25427,#25428,#25429,#25430,#25431,#25432,#25433,
#25434,#25435,#25436,#25437,#25438,#25439,#25440,#25441,#25442,#25443,#25444,
#25445,#25446,#25447,#25448,#25449,#25450,#25451,#25452,#25453,#25454,#25455,
#25456,#25457,#25458,#25459,#25460,#25461,#25462,#25463,#25464,#25465,#25466,
#25467,#25468,#25469,#25470,#25471,#25472,#25473,#25474,#25475,#25476,#25477,
#25478,#25479,#25480,#25481,#25482,#25483,#25484,#25485,#25486,#25487,#25488,
#25489,#25490,#25491,#25492,#25493,#25494,#25495,#25496,#25497,#25498,#25499,
#25500,#25501,#25502,#25503,#25504,#25505,#25506,#25507,#25508,#25509,#25510,
#25511,#25512,#25513,#25514,#25515,#25516,#25517,#25518,#25519,#25520,#25521,
#25522,#25523,#25524,#25525,#25526,#25527,#25528,#25529,#25530,#25531,#25532,
#25533,#25534,#25535,#25536,#25537,#25538,#25539,#25540,#25541,#25542,#25543,
#25544,#25545,#25546,#25547,#25548,#25549)),.UNSPECIFIED.,.F.,.F.,.F.)
B_SPLINE_SURFACE_WITH_KNOTS((4,4),(3,2,2,2,2,2,2,2,2,2,2,2,2,2,2,2,2,2,
2,2,2,2,2,2,2,2,2,2,2,2,2,2,2,2,2,2,2,2,2,2,2,2,2,2,2,2,2,2,2,2,2,2,2,2,
2,2,2,2,2,2,2,2,2,2,2,2,2,2,2,2,2,2,2,2,2,2,2,2,2,2,2,2,2,2,2,2,2,2,2,2,
2,2,2,2,2,2,2,2,2,2,2,2,2,2,2,2,2,2,2,2,2,2,2,2,2,2,2,2,2,2,2,2,2,2,2,2,
2,2,2,2,2,2,2,2,2,2,2,2,2,2,2,2,2,2,2,2,2,2,2,2,2,2,2,2,2,2,2,2,2,2,2,2,
2,2,2,2,2,2,2,2,2,2,2,2,2,2,2,2,2,2,2,2,2,2,2,2,2,2,2,2,2,2,2,2,2,2,2,2,
2,2,2,2,2,2,2,2,2,2,2,2,2,2,2,2,2,2,2,2,2,2,2,2,2,2,2,2,2,2,2,2,2,2,2,2,
2,2,2,2,2,2,2,2,2,2,2,2,2,2,2,2,2,2,2,2,2,2,2,2,2,2,2,2,2,2,2,2,2,2,2,2,
2,2,2,2,2,2,2,2,2,2,2,2,2,2,2,2,2,2,2,2,2,2,2,2,2,2,2,2,2,2,2,2,2,2,2,2,
2,2,2,2,2,2,2,2,2,2,2,2,2,2,2,2,2,2,2,2,2,2,2,2,2,2,2,2,2,2,2,2,2,2,2,2,
2,2,2,2,2,2,2,2,2,2,2,2,2,2,2,2,2,2,2,2,2,2,2,2,2,2,2,2,2,2,2,2,2,2,2,2,
2,2,2,2,2,2,2,2,2,2,2,2,2,2,2,2,2,2,2,2,2,2,2,2,2,2,2,2,2,2,2,2,2,2,2,2,
2,2,2,2,2,2,2,2,2,2,2,2,2,2,2,2,2,2,2,2,2,2,2,2,2,2,2,2,2,2,2,2,2,2,2,2,
2,2,2,2,2,2,2,2,2,2,2,2,2,2,2,2,2,2,2,2,2,2,2,2,2,2,2,2,2,2,2,2,2,2,2,2,
3),(0.,1.),(0.,0.00205761316872428,0.00411522633744856,0.00617283950617284,
0.00823045267489712,0.0102880658436214,0.0123456790123457,0.01440329218107,
0.0164609053497942,0.0185185185185185,0.0205761316872428,0.0226337448559671,
0.0246913580246914,0.0267489711934156,0.0288065843621399,0.0308641975308642,
0.0329218106995885,0.0349794238683128,0.037037037037037,0.0390946502057613,
0.0411522633744856,0.0432098765432099,0.0452674897119342,0.0473251028806584,
0.0493827160493827,0.051440329218107,0.0534979423868313,0.0555555555555556,
0.0576131687242798,0.0596707818930041,0.0617283950617284,0.0637860082304527,
0.065843621399177,0.0679012345679012,0.0699588477366255,0.0720164609053498,
0.0740740740740741,0.0761316872427984,0.0781893004115226,0.0802469135802469,
0.0823045267489712,0.0843621399176955,0.0864197530864197,0.088477366255144,
0.0905349794238683,0.0925925925925926,0.0946502057613169,0.0967078189300412,
0.0987654320987654,0.10082304526749,0.102880658436214,0.104938271604938,
0.106995884773663,0.109053497942387,0.111111111111111,0.113168724279835,
0.11522633744856,0.117283950617284,0.119341563786008,0.121399176954733,
0.123456790123457,0.125514403292181,0.127572016460905,0.12962962962963,
0.131687242798354,0.133744855967078,0.135802469135802,0.137860082304527,
0.139917695473251,0.141975308641975,0.1440329218107,0.146090534979424,0.148148148148148,
0.150205761316872,0.152263374485597,0.154320987654321,0.156378600823045,
0.15843621399177,0.160493827160494,0.162551440329218,0.164609053497942,
0.166666666666667,0.168724279835391,0.170781893004115,0.172839506172839,
0.174897119341564,0.176954732510288,0.179012345679012,0.181069958847737,
0.183127572016461,0.185185185185185,0.187242798353909,0.189300411522634,
0.191358024691358,0.193415637860082,0.195473251028807,0.197530864197531,
0.199588477366255,0.201646090534979,0.203703703703704,0.205761316872428,
0.207818930041152,0.209876543209877,0.211934156378601,0.213991769547325,
0.216049382716049,0.218106995884774,0.220164609053498,0.222222222222222,
0.224279835390947,0.226337448559671,0.228395061728395,0.230452674897119,
0.232510288065844,0.234567901234568,0.236625514403292,0.238683127572016,
0.240740740740741,0.242798353909465,0.244855967078189,0.246913580246914,
0.248971193415638,0.251028806584362,0.253086419753086,0.255144032921811,
0.257201646090535,0.259259259259259,0.261316872427984,0.263374485596708,
0.265432098765432,0.267489711934156,0.269547325102881,0.271604938271605,
0.273662551440329,0.275720164609054,0.277777777777778,0.279835390946502,
0.281893004115226,0.283950617283951,0.286008230452675,0.288065843621399,
0.290123456790123,0.292181069958848,0.294238683127572,0.296296296296296,
0.298353909465021,0.300411522633745,0.302469135802469,0.304526748971193,
0.306584362139918,0.308641975308642,0.310699588477366,0.312757201646091,
0.314814814814815,0.316872427983539,0.318930041152263,0.320987654320988,
0.323045267489712,0.325102880658436,0.327160493827161,0.329218106995885,
0.331275720164609,0.333333333333333,0.335390946502058,0.337448559670782,
0.339506172839506,0.34156378600823,0.343621399176955,0.345679012345679,
0.347736625514403,0.349794238683128,0.351851851851852,0.353909465020576,
0.3559670781893,0.358024691358025,0.360082304526749,0.362139917695473,0.364197530864198,
0.366255144032922,0.368312757201646,0.37037037037037,0.372427983539095,
0.374485596707819,0.376543209876543,0.378600823045267,0.380658436213992,
0.382716049382716,0.38477366255144,0.386831275720165,0.388888888888889,
0.390946502057613,0.393004115226337,0.395061728395062,0.397119341563786,
0.39917695473251,0.401234567901235,0.403292181069959,0.405349794238683,
0.407407407407407,0.409465020576132,0.411522633744856,0.41358024691358,
0.415637860082305,0.417695473251029,0.419753086419753,0.421810699588477,
0.423868312757202,0.425925925925926,0.42798353909465,0.430041152263374,
0.432098765432099,0.434156378600823,0.436213991769547,0.438271604938272,
0.440329218106996,0.44238683127572,0.444444444444444,0.446502057613169,
0.448559670781893,0.450617283950617,0.452674897119342,0.454732510288066,
0.45679012345679,0.458847736625514,0.460905349794239,0.462962962962963,
0.465020576131687,0.467078189300412,0.469135802469136,0.47119341563786,
0.473251028806584,0.475308641975309,0.477366255144033,0.479423868312757,
0.481481481481481,0.483539094650206,0.48559670781893,0.487654320987654,
0.489711934156379,0.491769547325103,0.493827160493827,0.495884773662551,
0.497942386831276,0.5,0.502057613168724,0.504115226337449,0.506172839506173,
0.508230452674897,0.510288065843621,0.512345679012346,0.51440329218107,
0.516460905349794,0.518518518518518,0.520576131687243,0.522633744855967,
0.524691358024691,0.526748971193416,0.52880658436214,0.530864197530864,
0.532921810699588,0.534979423868313,0.537037037037037,0.539094650205761,
0.541152263374486,0.54320987654321,0.545267489711934,0.547325102880658,
0.549382716049383,0.551440329218107,0.553497942386831,0.555555555555556,
0.55761316872428,0.559670781893004,0.561728395061728,0.563786008230453,
0.565843621399177,0.567901234567901,0.569958847736626,0.57201646090535,
0.574074074074074,0.576131687242798,0.578189300411523,0.580246913580247,
0.582304526748971,0.584362139917695,0.58641975308642,0.588477366255144,
0.590534979423868,0.592592592592593,0.594650205761317,0.596707818930041,
0.598765432098765,0.60082304526749,0.602880658436214,0.604938271604938,
0.606995884773663,0.609053497942387,0.611111111111111,0.613168724279835,
0.61522633744856,0.617283950617284,0.619341563786008,0.621399176954732,
0.623456790123457,0.625514403292181,0.627572016460905,0.62962962962963,
0.631687242798354,0.633744855967078,0.635802469135803,0.637860082304527,
0.639917695473251,0.641975308641975,0.6440329218107,0.646090534979424,0.648148148148148,
0.650205761316872,0.652263374485597,0.654320987654321,0.656378600823045,
0.65843621399177,0.660493827160494,0.662551440329218,0.664609053497942,
0.666666666666667,0.668724279835391,0.670781893004115,0.672839506172839,
0.674897119341564,0.676954732510288,0.679012345679012,0.681069958847737,
0.683127572016461,0.685185185185185,0.687242798353909,0.689300411522634,
0.691358024691358,0.693415637860082,0.695473251028807,0.697530864197531,
0.699588477366255,0.701646090534979,0.703703703703704,0.705761316872428,
0.707818930041152,0.709876543209877,0.711934156378601,0.713991769547325,
0.716049382716049,0.718106995884774,0.720164609053498,0.722222222222222,
0.724279835390947,0.726337448559671,0.728395061728395,0.730452674897119,
0.732510288065844,0.734567901234568,0.736625514403292,0.738683127572016,
0.740740740740741,0.742798353909465,0.744855967078189,0.746913580246914,
0.748971193415638,0.751028806584362,0.753086419753086,0.755144032921811,
0.757201646090535,0.759259259259259,0.761316872427984,0.763374485596708,
0.765432098765432,0.767489711934156,0.769547325102881,0.771604938271605,
0.773662551440329,0.775720164609053,0.777777777777778,0.779835390946502,
0.781893004115226,0.783950617283951,0.786008230452675,0.788065843621399,
0.790123456790123,0.792181069958848,0.794238683127572,0.796296296296296,
0.798353909465021,0.800411522633745,0.802469135802469,0.804526748971193,
0.806584362139918,0.808641975308642,0.810699588477366,0.812757201646091,
0.814814814814815,0.816872427983539,0.818930041152263,0.820987654320988,
0.823045267489712,0.825102880658436,0.827160493827161,0.829218106995885,
0.831275720164609,0.833333333333333,0.835390946502058,0.837448559670782,
0.839506172839506,0.84156378600823,0.843621399176955,0.845679012345679,
0.847736625514403,0.849794238683128,0.851851851851852,0.853909465020576,
0.8559670781893,0.858024691358025,0.860082304526749,0.862139917695473,0.864197530864197,
0.866255144032922,0.868312757201646,0.87037037037037,0.872427983539095,
0.874485596707819,0.876543209876543,0.878600823045268,0.880658436213992,
0.882716049382716,0.88477366255144,0.886831275720165,0.888888888888889,
0.890946502057613,0.893004115226337,0.895061728395062,0.897119341563786,
0.89917695473251,0.901234567901235,0.903292181069959,0.905349794238683,
0.907407407407407,0.909465020576132,0.911522633744856,0.91358024691358,
0.915637860082305,0.917695473251029,0.919753086419753,0.921810699588477,
0.923868312757202,0.925925925925926,0.92798353909465,0.930041152263374,
0.932098765432099,0.934156378600823,0.936213991769547,0.938271604938272,
0.940329218106996,0.94238683127572,0.944444444444444,0.946502057613169,
0.948559670781893,0.950617283950617,0.952674897119342,0.954732510288066,
0.95679012345679,0.958847736625514,0.960905349794239,0.962962962962963,
0.965020576131687,0.967078189300412,0.969135802469136,0.97119341563786,
0.973251028806584,0.975308641975309,0.977366255144033,0.979423868312757,
0.981481481481482,0.983539094650206,0.98559670781893,0.987654320987654,
0.989711934156379,0.991769547325103,0.993827160493827,0.995884773662551,
0.997942386831276,1.),.UNSPECIFIED.)
GEOMETRIC_REPRESENTATION_ITEM()
RATIONAL_B_SPLINE_SURFACE(((1.,0.866025403784439,1.,0.866025403784439,1.,
0.866025403784439,1.,0.866025403784439,1.,0.866025403784439,1.,0.866025403784439,
1.,0.866025403784439,1.,0.866025403784439,1.,0.866025403784439,1.,0.866025403784439,
1.,0.866025403784439,1.,0.866025403784439,1.,0.866025403784439,1.,0.866025403784439,
1.,0.866025403784439,1.,0.866025403784439,1.,0.866025403784439,1.,0.866025403784439,
1.,0.866025403784439,1.,0.866025403784439,1.,0.866025403784439,1.,0.866025403784439,
1.,0.866025403784439,1.,0.866025403784439,1.,0.866025403784439,1.,0.866025403784439,
1.,0.866025403784439,1.,0.866025403784439,1.,0.866025403784439,1.,0.866025403784439,
1.,0.866025403784439,1.,0.866025403784439,1.,0.866025403784439,1.,0.866025403784439,
1.,0.866025403784439,1.,0.866025403784439,1.,0.866025403784439,1.,0.866025403784439,
1.,0.866025403784439,1.,0.866025403784439,1.,0.866025403784439,1.,0.866025403784439,
1.,0.866025403784439,1.,0.866025403784439,1.,0.866025403784439,1.,0.866025403784439,
1.,0.866025403784439,1.,0.866025403784439,1.,0.866025403784439,1.,0.866025403784439,
1.,0.866025403784439,1.,0.866025403784439,1.,0.866025403784439,1.,0.866025403784439,
1.,0.866025403784439,1.,0.866025403784439,1.,0.866025403784439,1.,0.866025403784439,
1.,0.866025403784439,1.,0.866025403784439,1.,0.866025403784439,1.,0.866025403784439,
1.,0.866025403784439,1.,0.866025403784439,1.,0.866025403784439,1.,0.866025403784439,
1.,0.866025403784439,1.,0.866025403784439,1.,0.866025403784439,1.,0.866025403784439,
1.,0.866025403784439,1.,0.866025403784439,1.,0.866025403784439,1.,0.866025403784439,
1.,0.866025403784439,1.,0.866025403784439,1.,0.866025403784439,1.,0.866025403784439,
1.,0.866025403784439,1.,0.866025403784439,1.,0.866025403784439,1.,0.866025403784439,
1.,0.866025403784439,1.,0.866025403784439,1.,0.866025403784439,1.,0.866025403784439,
1.,0.866025403784439,1.,0.866025403784439,1.,0.866025403784439,1.,0.866025403784439,
1.,0.866025403784439,1.,0.866025403784439,1.,0.866025403784439,1.,0.866025403784439,
1.,0.866025403784439,1.,0.866025403784439,1.,0.866025403784439,1.,0.866025403784439,
1.,0.866025403784439,1.,0.866025403784439,1.,0.866025403784439,1.,0.866025403784439,
1.,0.866025403784439,1.,0.866025403784439,1.,0.866025403784439,1.,0.866025403784439,
1.,0.866025403784439,1.,0.866025403784439,1.,0.866025403784439,1.,0.866025403784439,
1.,0.866025403784439,1.,0.866025403784439,1.,0.866025403784439,1.,0.866025403784439,
1.,0.866025403784439,1.,0.866025403784439,1.,0.866025403784439,1.,0.866025403784439,
1.,0.866025403784439,1.,0.866025403784439,1.,0.866025403784439,1.,0.866025403784439,
1.,0.866025403784439,1.,0.866025403784439,1.,0.866025403784439,1.,0.866025403784439,
1.,0.866025403784439,1.,0.866025403784439,1.,0.866025403784439,1.,0.866025403784439,
1.,0.866025403784439,1.,0.866025403784439,1.,0.866025403784439,1.,0.866025403784439,
1.,0.866025403784439,1.,0.866025403784439,1.,0.866025403784439,1.,0.866025403784439,
1.,0.866025403784439,1.,0.866025403784439,1.,0.866025403784439,1.,0.866025403784439,
1.,0.866025403784439,1.,0.866025403784439,1.,0.866025403784439,1.,0.866025403784439,
1.,0.866025403784439,1.,0.866025403784439,1.,0.866025403784439,1.,0.866025403784439,
1.,0.866025403784439,1.,0.866025403784439,1.,0.866025403784439,1.,0.866025403784439,
1.,0.866025403784439,1.,0.866025403784439,1.,0.866025403784439,1.,0.866025403784439,
1.,0.866025403784439,1.,0.866025403784439,1.,0.866025403784439,1.,0.866025403784439,
1.,0.866025403784439,1.,0.866025403784439,1.,0.866025403784439,1.,0.866025403784439,
1.,0.866025403784439,1.,0.866025403784439,1.,0.866025403784439,1.,0.866025403784439,
1.,0.866025403784439,1.,0.866025403784439,1.,0.866025403784439,1.,0.866025403784439,
1.,0.866025403784439,1.,0.866025403784439,1.,0.866025403784439,1.,0.866025403784439,
1.,0.866025403784439,1.,0.866025403784439,1.,0.866025403784439,1.,0.866025403784439,
1.,0.866025403784439,1.,0.866025403784439,1.,0.866025403784439,1.,0.866025403784439,
1.,0.866025403784439,1.,0.866025403784439,1.,0.866025403784439,1.,0.866025403784439,
1.,0.866025403784439,1.,0.866025403784439,1.,0.866025403784439,1.,0.866025403784439,
1.,0.866025403784439,1.,0.866025403784439,1.,0.866025403784439,1.,0.866025403784439,
1.,0.866025403784439,1.,0.866025403784439,1.,0.866025403784439,1.,0.866025403784439,
1.,0.866025403784439,1.,0.866025403784439,1.,0.866025403784439,1.,0.866025403784439,
1.,0.866025403784439,1.,0.866025403784439,1.,0.866025403784439,1.,0.866025403784439,
1.,0.866025403784439,1.,0.866025403784439,1.,0.866025403784439,1.,0.866025403784439,
1.,0.866025403784439,1.,0.866025403784439,1.,0.866025403784439,1.,0.866025403784439,
1.,0.866025403784439,1.,0.866025403784439,1.,0.866025403784439,1.,0.866025403784439,
1.,0.866025403784439,1.,0.866025403784439,1.,0.866025403784439,1.,0.866025403784439,
1.,0.866025403784439,1.,0.866025403784439,1.,0.866025403784439,1.,0.866025403784439,
1.,0.866025403784439,1.,0.866025403784439,1.,0.866025403784439,1.,0.866025403784439,
1.,0.866025403784439,1.,0.866025403784439,1.,0.866025403784439,1.,0.866025403784439,
1.,0.866025403784439,1.,0.866025403784439,1.,0.866025403784439,1.,0.866025403784439,
1.,0.866025403784439,1.,0.866025403784439,1.,0.866025403784439,1.,0.866025403784439,
1.,0.866025403784439,1.,0.866025403784439,1.,0.866025403784439,1.,0.866025403784439,
1.,0.866025403784439,1.,0.866025403784439,1.,0.866025403784439,1.,0.866025403784439,
1.,0.866025403784439,1.,0.866025403784439,1.,0.866025403784439,1.,0.866025403784439,
1.,0.866025403784439,1.,0.866025403784439,1.,0.866025403784439,1.,0.866025403784439,
1.,0.866025403784439,1.,0.866025403784439,1.,0.866025403784439,1.,0.866025403784439,
1.,0.866025403784439,1.,0.866025403784439,1.,0.866025403784439,1.,0.866025403784439,
1.,0.866025403784439,1.,0.866025403784439,1.,0.866025403784439,1.,0.866025403784439,
1.,0.866025403784439,1.,0.866025403784439,1.,0.866025403784439,1.,0.866025403784439,
1.,0.866025403784439,1.,0.866025403784439,1.,0.866025403784439,1.,0.866025403784439,
1.,0.866025403784439,1.,0.866025403784439,1.,0.866025403784439,1.,0.866025403784439,
1.,0.866025403784439,1.,0.866025403784439,1.,0.866025403784439,1.,0.866025403784439,
1.,0.866025403784439,1.,0.866025403784439,1.,0.866025403784439,1.,0.866025403784439,
1.,0.866025403784439,1.,0.866025403784439,1.,0.866025403784439,1.,0.866025403784439,
1.,0.866025403784439,1.,0.866025403784439,1.,0.866025403784439,1.,0.866025403784439,
1.,0.866025403784439,1.,0.866025403784439,1.,0.866025403784439,1.,0.866025403784439,
1.,0.866025403784439,1.,0.866025403784439,1.,0.866025403784439,1.,0.866025403784439,
1.,0.866025403784439,1.,0.866025403784439,1.,0.866025403784439,1.,0.866025403784439,
1.,0.866025403784439,1.,0.866025403784439,1.,0.866025403784439,1.,0.866025403784439,
1.,0.866025403784439,1.,0.866025403784439,1.,0.866025403784439,1.,0.866025403784439,
1.,0.866025403784439,1.,0.866025403784439,1.,0.866025403784439,1.,0.866025403784439,
1.,0.866025403784439,1.,0.866025403784439,1.,0.866025403784439,1.,0.866025403784439,
1.,0.866025403784439,1.,0.866025403784439,1.,0.866025403784439,1.,0.866025403784439,
1.,0.866025403784439,1.,0.866025403784439,1.,0.866025403784439,1.,0.866025403784439,
1.,0.866025403784439,1.,0.866025403784439,1.,0.866025403784439,1.,0.866025403784439,
1.,0.866025403784439,1.,0.866025403784439,1.,0.866025403784439,1.,0.866025403784439,
1.,0.866025403784439,1.,0.866025403784439,1.,0.866025403784439,1.,0.866025403784439,
1.,0.866025403784439,1.,0.866025403784439,1.,0.866025403784439,1.,0.866025403784439,
1.,0.866025403784439,1.,0.866025403784439,1.,0.866025403784439,1.,0.866025403784439,
1.,0.866025403784439,1.,0.866025403784439,1.,0.866025403784439,1.,0.866025403784439,
1.,0.866025403784439,1.,0.866025403784439,1.,0.866025403784439,1.,0.866025403784439,
1.,0.866025403784439,1.,0.866025403784439,1.,0.866025403784439,1.,0.866025403784439,
1.,0.866025403784439,1.,0.866025403784439,1.,0.866025403784439,1.,0.866025403784439,
1.,0.866025403784439,1.,0.866025403784439,1.,0.866025403784439,1.,0.866025403784439,
1.,0.866025403784439,1.,0.866025403784439,1.,0.866025403784439,1.,0.866025403784439,
1.,0.866025403784439,1.,0.866025403784439,1.,0.866025403784439,1.,0.866025403784439,
1.,0.866025403784439,1.,0.866025403784439,1.,0.866025403784439,1.,0.866025403784439,
1.,0.866025403784439,1.,0.866025403784439,1.,0.866025403784439,1.,0.866025403784439,
1.,0.866025403784439,1.,0.866025403784439,1.,0.866025403784439,1.,0.866025403784439,
1.,0.866025403784439,1.,0.866025403784439,1.,0.866025403784439,1.,0.866025403784439,
1.,0.866025403784439,1.,0.866025403784439,1.,0.866025403784439,1.,0.866025403784439,
1.,0.866025403784439,1.,0.866025403784439,1.,0.866025403784439,1.,0.866025403784439,
1.,0.866025403784439,1.,0.866025403784439,1.,0.866025403784439,1.,0.866025403784439,
1.,0.866025403784439,1.,0.866025403784439,1.,0.866025403784439,1.,0.866025403784439,
1.,0.866025403784439,1.,0.866025403784439,1.,0.866025403784439,1.,0.866025403784439,
1.,0.866025403784439,1.,0.866025403784439,1.,0.866025403784439,1.,0.866025403784439,
1.,0.866025403784439,1.,0.866025403784439,1.,0.866025403784439,1.,0.866025403784439,
1.,0.866025403784439,1.,0.866025403784439,1.,0.866025403784439,1.,0.866025403784439,
1.,0.866025403784439,1.,0.866025403784439,1.,0.866025403784439,1.,0.866025403784439,
1.,0.866025403784439,1.,0.866025403784439,1.,0.866025403784439,1.,0.866025403784439,
1.,0.866025403784439,1.,0.866025403784439,1.,0.866025403784439,1.,0.866025403784439,
1.,0.866025403784439,1.,0.866025403784439,1.,0.866025403784439,1.,0.866025403784439,
1.,0.866025403784439,1.,0.866025403784439,1.,0.866025403784439,1.,0.866025403784439,
1.,0.866025403784439,1.,0.866025403784439,1.,0.866025403784439,1.,0.866025403784439,
1.,0.866025403784439,1.,0.866025403784439,1.,0.866025403784439,1.,0.866025403784439,
1.,0.866025403784439,1.,0.866025403784439,1.,0.866025403784439,1.,0.866025403784439,
1.,0.866025403784439,1.,0.866025403784439,1.,0.866025403784439,1.,0.866025403784439,
1.,0.866025403784439,1.,0.866025403784439,1.,0.866025403784439,1.,0.866025403784439,
1.,0.866025403784439,1.,0.866025403784439,1.,0.866025403784439,1.,0.866025403784439,
1.,0.866025403784439,1.,0.866025403784439,1.,0.866025403784439,1.,0.866025403784439,
1.,0.866025403784439,1.,0.866025403784439,1.,0.866025403784439,1.,0.866025403784439,
1.),(0.641165742156689,0.555265820743996,0.641165742156689,0.555265820743996,
0.641165742156689,0.555265820743996,0.641165742156689,0.555265820743996,
0.641165742156689,0.555265820743996,0.641165742156689,0.555265820743996,
0.641165742156689,0.555265820743996,0.641165742156689,0.555265820743996,
0.641165742156689,0.555265820743996,0.641165742156689,0.555265820743996,
0.641165742156689,0.555265820743996,0.641165742156689,0.555265820743996,
0.641165742156689,0.555265820743996,0.641165742156689,0.555265820743996,
0.641165742156689,0.555265820743996,0.641165742156689,0.555265820743996,
0.641165742156689,0.555265820743996,0.641165742156689,0.555265820743996,
0.641165742156689,0.555265820743996,0.641165742156689,0.555265820743996,
0.641165742156689,0.555265820743996,0.641165742156689,0.555265820743996,
0.641165742156689,0.555265820743996,0.641165742156689,0.555265820743996,
0.641165742156689,0.555265820743996,0.641165742156689,0.555265820743996,
0.641165742156689,0.555265820743996,0.641165742156689,0.555265820743996,
0.641165742156689,0.555265820743996,0.641165742156689,0.555265820743996,
0.641165742156689,0.555265820743996,0.641165742156689,0.555265820743996,
0.641165742156689,0.555265820743996,0.641165742156689,0.555265820743996,
0.641165742156689,0.555265820743996,0.641165742156689,0.555265820743996,
0.641165742156689,0.555265820743996,0.641165742156689,0.555265820743996,
0.641165742156689,0.555265820743996,0.641165742156689,0.555265820743996,
0.641165742156689,0.555265820743996,0.641165742156689,0.555265820743996,
0.641165742156689,0.555265820743996,0.641165742156689,0.555265820743996,
0.641165742156689,0.555265820743996,0.641165742156689,0.555265820743996,
0.641165742156689,0.555265820743996,0.641165742156689,0.555265820743996,
0.641165742156689,0.555265820743996,0.641165742156689,0.555265820743996,
0.641165742156689,0.555265820743996,0.641165742156689,0.555265820743996,
0.641165742156689,0.555265820743996,0.641165742156689,0.555265820743996,
0.641165742156689,0.555265820743996,0.641165742156689,0.555265820743996,
0.641165742156689,0.555265820743996,0.641165742156689,0.555265820743996,
0.641165742156689,0.555265820743996,0.641165742156689,0.555265820743996,
0.641165742156689,0.555265820743996,0.641165742156689,0.555265820743996,
0.641165742156689,0.555265820743996,0.641165742156689,0.555265820743996,
0.641165742156689,0.555265820743996,0.641165742156689,0.555265820743996,
0.641165742156689,0.555265820743996,0.641165742156689,0.555265820743996,
0.641165742156689,0.555265820743996,0.641165742156689,0.555265820743996,
0.641165742156689,0.555265820743996,0.641165742156689,0.555265820743996,
0.641165742156689,0.555265820743996,0.641165742156689,0.555265820743996,
0.641165742156689,0.555265820743996,0.641165742156689,0.555265820743996,
0.641165742156689,0.555265820743996,0.641165742156689,0.555265820743996,
0.641165742156689,0.555265820743996,0.641165742156689,0.555265820743996,
0.641165742156689,0.555265820743996,0.641165742156689,0.555265820743996,
0.641165742156689,0.555265820743996,0.641165742156689,0.555265820743996,
0.641165742156689,0.555265820743996,0.641165742156689,0.555265820743996,
0.641165742156689,0.555265820743996,0.641165742156689,0.555265820743996,
0.641165742156689,0.555265820743996,0.641165742156689,0.555265820743996,
0.641165742156689,0.555265820743996,0.641165742156689,0.555265820743996,
0.641165742156689,0.555265820743996,0.641165742156689,0.555265820743996,
0.641165742156689,0.555265820743996,0.641165742156689,0.555265820743996,
0.641165742156689,0.555265820743996,0.641165742156689,0.555265820743996,
0.641165742156689,0.555265820743996,0.641165742156689,0.555265820743996,
0.641165742156689,0.555265820743996,0.641165742156689,0.555265820743996,
0.641165742156689,0.555265820743996,0.641165742156689,0.555265820743996,
0.641165742156689,0.555265820743996,0.641165742156689,0.555265820743996,
0.641165742156689,0.555265820743996,0.641165742156689,0.555265820743996,
0.641165742156689,0.555265820743996,0.641165742156689,0.555265820743996,
0.641165742156689,0.555265820743996,0.641165742156689,0.555265820743996,
0.641165742156689,0.555265820743996,0.641165742156689,0.555265820743996,
0.641165742156689,0.555265820743996,0.641165742156689,0.555265820743996,
0.641165742156689,0.555265820743996,0.641165742156689,0.555265820743996,
0.641165742156689,0.555265820743996,0.641165742156689,0.555265820743996,
0.641165742156689,0.555265820743996,0.641165742156689,0.555265820743996,
0.641165742156689,0.555265820743996,0.641165742156689,0.555265820743996,
0.641165742156689,0.555265820743996,0.641165742156689,0.555265820743996,
0.641165742156689,0.555265820743996,0.641165742156689,0.555265820743996,
0.641165742156689,0.555265820743996,0.641165742156689,0.555265820743996,
0.641165742156689,0.555265820743996,0.641165742156689,0.555265820743996,
0.641165742156689,0.555265820743996,0.641165742156689,0.555265820743996,
0.641165742156689,0.555265820743996,0.641165742156689,0.555265820743996,
0.641165742156689,0.555265820743996,0.641165742156689,0.555265820743996,
0.641165742156689,0.555265820743996,0.641165742156689,0.555265820743996,
0.641165742156689,0.555265820743996,0.641165742156689,0.555265820743996,
0.641165742156689,0.555265820743996,0.641165742156689,0.555265820743996,
0.641165742156689,0.555265820743996,0.641165742156689,0.555265820743996,
0.641165742156689,0.555265820743996,0.641165742156689,0.555265820743996,
0.641165742156689,0.555265820743996,0.641165742156689,0.555265820743996,
0.641165742156689,0.555265820743996,0.641165742156689,0.555265820743996,
0.641165742156689,0.555265820743996,0.641165742156689,0.555265820743996,
0.641165742156689,0.555265820743996,0.641165742156689,0.555265820743996,
0.641165742156689,0.555265820743996,0.641165742156689,0.555265820743996,
0.641165742156689,0.555265820743996,0.641165742156689,0.555265820743996,
0.641165742156689,0.555265820743996,0.641165742156689,0.555265820743996,
0.641165742156689,0.555265820743996,0.641165742156689,0.555265820743996,
0.641165742156689,0.555265820743996,0.641165742156689,0.555265820743996,
0.641165742156689,0.555265820743996,0.641165742156689,0.555265820743996,
0.641165742156689,0.555265820743996,0.641165742156689,0.555265820743996,
0.641165742156689,0.555265820743996,0.641165742156689,0.555265820743996,
0.641165742156689,0.555265820743996,0.641165742156689,0.555265820743996,
0.641165742156689,0.555265820743996,0.641165742156689,0.555265820743996,
0.641165742156689,0.555265820743996,0.641165742156689,0.555265820743996,
0.641165742156689,0.555265820743996,0.641165742156689,0.555265820743996,
0.641165742156689,0.555265820743996,0.641165742156689,0.555265820743996,
0.641165742156689,0.555265820743996,0.641165742156689,0.555265820743996,
0.641165742156689,0.555265820743996,0.641165742156689,0.555265820743996,
0.641165742156689,0.555265820743996,0.641165742156689,0.555265820743996,
0.641165742156689,0.555265820743996,0.641165742156689,0.555265820743996,
0.641165742156689,0.555265820743996,0.641165742156689,0.555265820743996,
0.641165742156689,0.555265820743996,0.641165742156689,0.555265820743996,
0.641165742156689,0.555265820743996,0.641165742156689,0.555265820743996,
0.641165742156689,0.555265820743996,0.641165742156689,0.555265820743996,
0.641165742156689,0.555265820743996,0.641165742156689,0.555265820743996,
0.641165742156689,0.555265820743996,0.641165742156689,0.555265820743996,
0.641165742156689,0.555265820743996,0.641165742156689,0.555265820743996,
0.641165742156689,0.555265820743996,0.641165742156689,0.555265820743996,
0.641165742156689,0.555265820743996,0.641165742156689,0.555265820743996,
0.641165742156689,0.555265820743996,0.641165742156689,0.555265820743996,
0.641165742156689,0.555265820743996,0.641165742156689,0.555265820743996,
0.641165742156689,0.555265820743996,0.641165742156689,0.555265820743996,
0.641165742156689,0.555265820743996,0.641165742156689,0.555265820743996,
0.641165742156689,0.555265820743996,0.641165742156689,0.555265820743996,
0.641165742156689,0.555265820743996,0.641165742156689,0.555265820743996,
0.641165742156689,0.555265820743996,0.641165742156689,0.555265820743996,
0.641165742156689,0.555265820743996,0.641165742156689,0.555265820743996,
0.641165742156689,0.555265820743996,0.641165742156689,0.555265820743996,
0.641165742156689,0.555265820743996,0.641165742156689,0.555265820743996,
0.641165742156689,0.555265820743996,0.641165742156689,0.555265820743996,
0.641165742156689,0.555265820743996,0.641165742156689,0.555265820743996,
0.641165742156689,0.555265820743996,0.641165742156689,0.555265820743996,
0.641165742156689,0.555265820743996,0.641165742156689,0.555265820743996,
0.641165742156689,0.555265820743996,0.641165742156689,0.555265820743996,
0.641165742156689,0.555265820743996,0.641165742156689,0.555265820743996,
0.641165742156689,0.555265820743996,0.641165742156689,0.555265820743996,
0.641165742156689,0.555265820743996,0.641165742156689,0.555265820743996,
0.641165742156689,0.555265820743996,0.641165742156689,0.555265820743996,
0.641165742156689,0.555265820743996,0.641165742156689,0.555265820743996,
0.641165742156689,0.555265820743996,0.641165742156689,0.555265820743996,
0.641165742156689,0.555265820743996,0.641165742156689,0.555265820743996,
0.641165742156689,0.555265820743996,0.641165742156689,0.555265820743996,
0.641165742156689,0.555265820743996,0.641165742156689,0.555265820743996,
0.641165742156689,0.555265820743996,0.641165742156689,0.555265820743996,
0.641165742156689,0.555265820743996,0.641165742156689,0.555265820743996,
0.641165742156689,0.555265820743996,0.641165742156689,0.555265820743996,
0.641165742156689,0.555265820743996,0.641165742156689,0.555265820743996,
0.641165742156689,0.555265820743996,0.641165742156689,0.555265820743996,
0.641165742156689,0.555265820743996,0.641165742156689,0.555265820743996,
0.641165742156689,0.555265820743996,0.641165742156689,0.555265820743996,
0.641165742156689,0.555265820743996,0.641165742156689,0.555265820743996,
0.641165742156689,0.555265820743996,0.641165742156689,0.555265820743996,
0.641165742156689,0.555265820743996,0.641165742156689,0.555265820743996,
0.641165742156689,0.555265820743996,0.641165742156689,0.555265820743996,
0.641165742156689,0.555265820743996,0.641165742156689,0.555265820743996,
0.641165742156689,0.555265820743996,0.641165742156689,0.555265820743996,
0.641165742156689,0.555265820743996,0.641165742156689,0.555265820743996,
0.641165742156689,0.555265820743996,0.641165742156689,0.555265820743996,
0.641165742156689,0.555265820743996,0.641165742156689,0.555265820743996,
0.641165742156689,0.555265820743996,0.641165742156689,0.555265820743996,
0.641165742156689,0.555265820743996,0.641165742156689,0.555265820743996,
0.641165742156689,0.555265820743996,0.641165742156689,0.555265820743996,
0.641165742156689,0.555265820743996,0.641165742156689,0.555265820743996,
0.641165742156689,0.555265820743996,0.641165742156689,0.555265820743996,
0.641165742156689,0.555265820743996,0.641165742156689,0.555265820743996,
0.641165742156689,0.555265820743996,0.641165742156689,0.555265820743996,
0.641165742156689,0.555265820743996,0.641165742156689,0.555265820743996,
0.641165742156689,0.555265820743996,0.641165742156689,0.555265820743996,
0.641165742156689,0.555265820743996,0.641165742156689,0.555265820743996,
0.641165742156689,0.555265820743996,0.641165742156689,0.555265820743996,
0.641165742156689,0.555265820743996,0.641165742156689,0.555265820743996,
0.641165742156689,0.555265820743996,0.641165742156689,0.555265820743996,
0.641165742156689,0.555265820743996,0.641165742156689,0.555265820743996,
0.641165742156689,0.555265820743996,0.641165742156689,0.555265820743996,
0.641165742156689,0.555265820743996,0.641165742156689,0.555265820743996,
0.641165742156689,0.555265820743996,0.641165742156689,0.555265820743996,
0.641165742156689,0.555265820743996,0.641165742156689,0.555265820743996,
0.641165742156689,0.555265820743996,0.641165742156689,0.555265820743996,
0.641165742156689,0.555265820743996,0.641165742156689,0.555265820743996,
0.641165742156689,0.555265820743996,0.641165742156689,0.555265820743996,
0.641165742156689,0.555265820743996,0.641165742156689,0.555265820743996,
0.641165742156689,0.555265820743996,0.641165742156689,0.555265820743996,
0.641165742156689,0.555265820743996,0.641165742156689,0.555265820743996,
0.641165742156689,0.555265820743996,0.641165742156689,0.555265820743996,
0.641165742156689,0.555265820743996,0.641165742156689,0.555265820743996,
0.641165742156689,0.555265820743996,0.641165742156689,0.555265820743996,
0.641165742156689,0.555265820743996,0.641165742156689,0.555265820743996,
0.641165742156689,0.555265820743996,0.641165742156689,0.555265820743996,
0.641165742156689,0.555265820743996,0.641165742156689,0.555265820743996,
0.641165742156689,0.555265820743996,0.641165742156689,0.555265820743996,
0.641165742156689,0.555265820743996,0.641165742156689,0.555265820743996,
0.641165742156689,0.555265820743996,0.641165742156689,0.555265820743996,
0.641165742156689,0.555265820743996,0.641165742156689,0.555265820743996,
0.641165742156689,0.555265820743996,0.641165742156689,0.555265820743996,
0.641165742156689,0.555265820743996,0.641165742156689,0.555265820743996,
0.641165742156689,0.555265820743996,0.641165742156689,0.555265820743996,
0.641165742156689,0.555265820743996,0.641165742156689,0.555265820743996,
0.641165742156689,0.555265820743996,0.641165742156689,0.555265820743996,
0.641165742156689,0.555265820743996,0.641165742156689,0.555265820743996,
0.641165742156689,0.555265820743996,0.641165742156689,0.555265820743996,
0.641165742156689,0.555265820743996,0.641165742156689,0.555265820743996,
0.641165742156689,0.555265820743996,0.641165742156689,0.555265820743996,
0.641165742156689,0.555265820743996,0.641165742156689,0.555265820743996,
0.641165742156689,0.555265820743996,0.641165742156689,0.555265820743996,
0.641165742156689,0.555265820743996,0.641165742156689,0.555265820743996,
0.641165742156689,0.555265820743996,0.641165742156689,0.555265820743996,
0.641165742156689,0.555265820743996,0.641165742156689,0.555265820743996,
0.641165742156689,0.555265820743996,0.641165742156689,0.555265820743996,
0.641165742156689,0.555265820743996,0.641165742156689,0.555265820743996,
0.641165742156689,0.555265820743996,0.641165742156689,0.555265820743996,
0.641165742156689,0.555265820743996,0.641165742156689,0.555265820743996,
0.641165742156689,0.555265820743996,0.641165742156689,0.555265820743996,
0.641165742156689,0.555265820743996,0.641165742156689,0.555265820743996,
0.641165742156689,0.555265820743996,0.641165742156689,0.555265820743996,
0.641165742156689,0.555265820743996,0.641165742156689,0.555265820743996,
0.641165742156689,0.555265820743996,0.641165742156689,0.555265820743996,
0.641165742156689,0.555265820743996,0.641165742156689,0.555265820743996,
0.641165742156689,0.555265820743996,0.641165742156689,0.555265820743996,
0.641165742156689,0.555265820743996,0.641165742156689,0.555265820743996,
0.641165742156689,0.555265820743996,0.641165742156689,0.555265820743996,
0.641165742156689,0.555265820743996,0.641165742156689,0.555265820743996,
0.641165742156689,0.555265820743996,0.641165742156689,0.555265820743996,
0.641165742156689,0.555265820743996,0.641165742156689,0.555265820743996,
0.641165742156689,0.555265820743996,0.641165742156689,0.555265820743996,
0.641165742156689,0.555265820743996,0.641165742156689,0.555265820743996,
0.641165742156689,0.555265820743996,0.641165742156689,0.555265820743996,
0.641165742156689,0.555265820743996,0.641165742156689,0.555265820743996,
0.641165742156689,0.555265820743996,0.641165742156689,0.555265820743996,
0.641165742156689,0.555265820743996,0.641165742156689,0.555265820743996,
0.641165742156689,0.555265820743996,0.641165742156689,0.555265820743996,
0.641165742156689,0.555265820743996,0.641165742156689,0.555265820743996,
0.641165742156689,0.555265820743996,0.641165742156689,0.555265820743996,
0.641165742156689,0.555265820743996,0.641165742156689,0.555265820743996,
0.641165742156689,0.555265820743996,0.641165742156689,0.555265820743996,
0.641165742156689,0.555265820743996,0.641165742156689,0.555265820743996,
0.641165742156689,0.555265820743996,0.641165742156689,0.555265820743996,
0.641165742156689,0.555265820743996,0.641165742156689,0.555265820743996,
0.641165742156689,0.555265820743996,0.641165742156689,0.555265820743996,
0.641165742156689,0.555265820743996,0.641165742156689,0.555265820743996,
0.641165742156689,0.555265820743996,0.641165742156689,0.555265820743996,
0.641165742156689,0.555265820743996,0.641165742156689,0.555265820743996,
0.641165742156689,0.555265820743996,0.641165742156689,0.555265820743996,
0.641165742156689,0.555265820743996,0.641165742156689,0.555265820743996,
0.641165742156689,0.555265820743996,0.641165742156689,0.555265820743996,
0.641165742156689,0.555265820743996,0.641165742156689,0.555265820743996,
0.641165742156689,0.555265820743996,0.641165742156689,0.555265820743996,
0.641165742156689,0.555265820743996,0.641165742156689,0.555265820743996,
0.641165742156689,0.555265820743996,0.641165742156689,0.555265820743996,
0.641165742156689,0.555265820743996,0.641165742156689,0.555265820743996,
0.641165742156689,0.555265820743996,0.641165742156689,0.555265820743996,
0.641165742156689,0.555265820743996,0.641165742156689,0.555265820743996,
0.641165742156689,0.555265820743996,0.641165742156689,0.555265820743996,
0.641165742156689,0.555265820743996,0.641165742156689,0.555265820743996,
0.641165742156689,0.555265820743996,0.641165742156689,0.555265820743996,
0.641165742156689,0.555265820743996,0.641165742156689,0.555265820743996,
0.641165742156689,0.555265820743996,0.641165742156689,0.555265820743996,
0.641165742156689,0.555265820743996,0.641165742156689,0.555265820743996,
0.641165742156689,0.555265820743996,0.641165742156689,0.555265820743996,
0.641165742156689),(0.641165742156689,0.555265820743996,0.641165742156689,
0.555265820743996,0.641165742156689,0.555265820743996,0.641165742156689,
0.555265820743996,0.641165742156689,0.555265820743996,0.641165742156689,
0.555265820743996,0.641165742156689,0.555265820743996,0.641165742156689,
0.555265820743996,0.641165742156689,0.555265820743996,0.641165742156689,
0.555265820743996,0.641165742156689,0.555265820743996,0.641165742156689,
0.555265820743996,0.641165742156689,0.555265820743996,0.641165742156689,
0.555265820743996,0.641165742156689,0.555265820743996,0.641165742156689,
0.555265820743996,0.641165742156689,0.555265820743996,0.641165742156689,
0.555265820743996,0.641165742156689,0.555265820743996,0.641165742156689,
0.555265820743996,0.641165742156689,0.555265820743996,0.641165742156689,
0.555265820743996,0.641165742156689,0.555265820743996,0.641165742156689,
0.555265820743996,0.641165742156689,0.555265820743996,0.641165742156689,
0.555265820743996,0.641165742156689,0.555265820743996,0.641165742156689,
0.555265820743996,0.641165742156689,0.555265820743996,0.641165742156689,
0.555265820743996,0.641165742156689,0.555265820743996,0.641165742156689,
0.555265820743996,0.641165742156689,0.555265820743996,0.641165742156689,
0.555265820743996,0.641165742156689,0.555265820743996,0.641165742156689,
0.555265820743996,0.641165742156689,0.555265820743996,0.641165742156689,
0.555265820743996,0.641165742156689,0.555265820743996,0.641165742156689,
0.555265820743996,0.641165742156689,0.555265820743996,0.641165742156689,
0.555265820743996,0.641165742156689,0.555265820743996,0.641165742156689,
0.555265820743996,0.641165742156689,0.555265820743996,0.641165742156689,
0.555265820743996,0.641165742156689,0.555265820743996,0.641165742156689,
0.555265820743996,0.641165742156689,0.555265820743996,0.641165742156689,
0.555265820743996,0.641165742156689,0.555265820743996,0.641165742156689,
0.555265820743996,0.641165742156689,0.555265820743996,0.641165742156689,
0.555265820743996,0.641165742156689,0.555265820743996,0.641165742156689,
0.555265820743996,0.641165742156689,0.555265820743996,0.641165742156689,
0.555265820743996,0.641165742156689,0.555265820743996,0.641165742156689,
0.555265820743996,0.641165742156689,0.555265820743996,0.641165742156689,
0.555265820743996,0.641165742156689,0.555265820743996,0.641165742156689,
0.555265820743996,0.641165742156689,0.555265820743996,0.641165742156689,
0.555265820743996,0.641165742156689,0.555265820743996,0.641165742156689,
0.555265820743996,0.641165742156689,0.555265820743996,0.641165742156689,
0.555265820743996,0.641165742156689,0.555265820743996,0.641165742156689,
0.555265820743996,0.641165742156689,0.555265820743996,0.641165742156689,
0.555265820743996,0.641165742156689,0.555265820743996,0.641165742156689,
0.555265820743996,0.641165742156689,0.555265820743996,0.641165742156689,
0.555265820743996,0.641165742156689,0.555265820743996,0.641165742156689,
0.555265820743996,0.641165742156689,0.555265820743996,0.641165742156689,
0.555265820743996,0.641165742156689,0.555265820743996,0.641165742156689,
0.555265820743996,0.641165742156689,0.555265820743996,0.641165742156689,
0.555265820743996,0.641165742156689,0.555265820743996,0.641165742156689,
0.555265820743996,0.641165742156689,0.555265820743996,0.641165742156689,
0.555265820743996,0.641165742156689,0.555265820743996,0.641165742156689,
0.555265820743996,0.641165742156689,0.555265820743996,0.641165742156689,
0.555265820743996,0.641165742156689,0.555265820743996,0.641165742156689,
0.555265820743996,0.641165742156689,0.555265820743996,0.641165742156689,
0.555265820743996,0.641165742156689,0.555265820743996,0.641165742156689,
0.555265820743996,0.641165742156689,0.555265820743996,0.641165742156689,
0.555265820743996,0.641165742156689,0.555265820743996,0.641165742156689,
0.555265820743996,0.641165742156689,0.555265820743996,0.641165742156689,
0.555265820743996,0.641165742156689,0.555265820743996,0.641165742156689,
0.555265820743996,0.641165742156689,0.555265820743996,0.641165742156689,
0.555265820743996,0.641165742156689,0.555265820743996,0.641165742156689,
0.555265820743996,0.641165742156689,0.555265820743996,0.641165742156689,
0.555265820743996,0.641165742156689,0.555265820743996,0.641165742156689,
0.555265820743996,0.641165742156689,0.555265820743996,0.641165742156689,
0.555265820743996,0.641165742156689,0.555265820743996,0.641165742156689,
0.555265820743996,0.641165742156689,0.555265820743996,0.641165742156689,
0.555265820743996,0.641165742156689,0.555265820743996,0.641165742156689,
0.555265820743996,0.641165742156689,0.555265820743996,0.641165742156689,
0.555265820743996,0.641165742156689,0.555265820743996,0.641165742156689,
0.555265820743996,0.641165742156689,0.555265820743996,0.641165742156689,
0.555265820743996,0.641165742156689,0.555265820743996,0.641165742156689,
0.555265820743996,0.641165742156689,0.555265820743996,0.641165742156689,
0.555265820743996,0.641165742156689,0.555265820743996,0.641165742156689,
0.555265820743996,0.641165742156689,0.555265820743996,0.641165742156689,
0.555265820743996,0.641165742156689,0.555265820743996,0.641165742156689,
0.555265820743996,0.641165742156689,0.555265820743996,0.641165742156689,
0.555265820743996,0.641165742156689,0.555265820743996,0.641165742156689,
0.555265820743996,0.641165742156689,0.555265820743996,0.641165742156689,
0.555265820743996,0.641165742156689,0.555265820743996,0.641165742156689,
0.555265820743996,0.641165742156689,0.555265820743996,0.641165742156689,
0.555265820743996,0.641165742156689,0.555265820743996,0.641165742156689,
0.555265820743996,0.641165742156689,0.555265820743996,0.641165742156689,
0.555265820743996,0.641165742156689,0.555265820743996,0.641165742156689,
0.555265820743996,0.641165742156689,0.555265820743996,0.641165742156689,
0.555265820743996,0.641165742156689,0.555265820743996,0.641165742156689,
0.555265820743996,0.641165742156689,0.555265820743996,0.641165742156689,
0.555265820743996,0.641165742156689,0.555265820743996,0.641165742156689,
0.555265820743996,0.641165742156689,0.555265820743996,0.641165742156689,
0.555265820743996,0.641165742156689,0.555265820743996,0.641165742156689,
0.555265820743996,0.641165742156689,0.555265820743996,0.641165742156689,
0.555265820743996,0.641165742156689,0.555265820743996,0.641165742156689,
0.555265820743996,0.641165742156689,0.555265820743996,0.641165742156689,
0.555265820743996,0.641165742156689,0.555265820743996,0.641165742156689,
0.555265820743996,0.641165742156689,0.555265820743996,0.641165742156689,
0.555265820743996,0.641165742156689,0.555265820743996,0.641165742156689,
0.555265820743996,0.641165742156689,0.555265820743996,0.641165742156689,
0.555265820743996,0.641165742156689,0.555265820743996,0.641165742156689,
0.555265820743996,0.641165742156689,0.555265820743996,0.641165742156689,
0.555265820743996,0.641165742156689,0.555265820743996,0.641165742156689,
0.555265820743996,0.641165742156689,0.555265820743996,0.641165742156689,
0.555265820743996,0.641165742156689,0.555265820743996,0.641165742156689,
0.555265820743996,0.641165742156689,0.555265820743996,0.641165742156689,
0.555265820743996,0.641165742156689,0.555265820743996,0.641165742156689,
0.555265820743996,0.641165742156689,0.555265820743996,0.641165742156689,
0.555265820743996,0.641165742156689,0.555265820743996,0.641165742156689,
0.555265820743996,0.641165742156689,0.555265820743996,0.641165742156689,
0.555265820743996,0.641165742156689,0.555265820743996,0.641165742156689,
0.555265820743996,0.641165742156689,0.555265820743996,0.641165742156689,
0.555265820743996,0.641165742156689,0.555265820743996,0.641165742156689,
0.555265820743996,0.641165742156689,0.555265820743996,0.641165742156689,
0.555265820743996,0.641165742156689,0.555265820743996,0.641165742156689,
0.555265820743996,0.641165742156689,0.555265820743996,0.641165742156689,
0.555265820743996,0.641165742156689,0.555265820743996,0.641165742156689,
0.555265820743996,0.641165742156689,0.555265820743996,0.641165742156689,
0.555265820743996,0.641165742156689,0.555265820743996,0.641165742156689,
0.555265820743996,0.641165742156689,0.555265820743996,0.641165742156689,
0.555265820743996,0.641165742156689,0.555265820743996,0.641165742156689,
0.555265820743996,0.641165742156689,0.555265820743996,0.641165742156689,
0.555265820743996,0.641165742156689,0.555265820743996,0.641165742156689,
0.555265820743996,0.641165742156689,0.555265820743996,0.641165742156689,
0.555265820743996,0.641165742156689,0.555265820743996,0.641165742156689,
0.555265820743996,0.641165742156689,0.555265820743996,0.641165742156689,
0.555265820743996,0.641165742156689,0.555265820743996,0.641165742156689,
0.555265820743996,0.641165742156689,0.555265820743996,0.641165742156689,
0.555265820743996,0.641165742156689,0.555265820743996,0.641165742156689,
0.555265820743996,0.641165742156689,0.555265820743996,0.641165742156689,
0.555265820743996,0.641165742156689,0.555265820743996,0.641165742156689,
0.555265820743996,0.641165742156689,0.555265820743996,0.641165742156689,
0.555265820743996,0.641165742156689,0.555265820743996,0.641165742156689,
0.555265820743996,0.641165742156689,0.555265820743996,0.641165742156689,
0.555265820743996,0.641165742156689,0.555265820743996,0.641165742156689,
0.555265820743996,0.641165742156689,0.555265820743996,0.641165742156689,
0.555265820743996,0.641165742156689,0.555265820743996,0.641165742156689,
0.555265820743996,0.641165742156689,0.555265820743996,0.641165742156689,
0.555265820743996,0.641165742156689,0.555265820743996,0.641165742156689,
0.555265820743996,0.641165742156689,0.555265820743996,0.641165742156689,
0.555265820743996,0.641165742156689,0.555265820743996,0.641165742156689,
0.555265820743996,0.641165742156689,0.555265820743996,0.641165742156689,
0.555265820743996,0.641165742156689,0.555265820743996,0.641165742156689,
0.555265820743996,0.641165742156689,0.555265820743996,0.641165742156689,
0.555265820743996,0.641165742156689,0.555265820743996,0.641165742156689,
0.555265820743996,0.641165742156689,0.555265820743996,0.641165742156689,
0.555265820743996,0.641165742156689,0.555265820743996,0.641165742156689,
0.555265820743996,0.641165742156689,0.555265820743996,0.641165742156689,
0.555265820743996,0.641165742156689,0.555265820743996,0.641165742156689,
0.555265820743996,0.641165742156689,0.555265820743996,0.641165742156689,
0.555265820743996,0.641165742156689,0.555265820743996,0.641165742156689,
0.555265820743996,0.641165742156689,0.555265820743996,0.641165742156689,
0.555265820743996,0.641165742156689,0.555265820743996,0.641165742156689,
0.555265820743996,0.641165742156689,0.555265820743996,0.641165742156689,
0.555265820743996,0.641165742156689,0.555265820743996,0.641165742156689,
0.555265820743996,0.641165742156689,0.555265820743996,0.641165742156689,
0.555265820743996,0.641165742156689,0.555265820743996,0.641165742156689,
0.555265820743996,0.641165742156689,0.555265820743996,0.641165742156689,
0.555265820743996,0.641165742156689,0.555265820743996,0.641165742156689,
0.555265820743996,0.641165742156689,0.555265820743996,0.641165742156689,
0.555265820743996,0.641165742156689,0.555265820743996,0.641165742156689,
0.555265820743996,0.641165742156689,0.555265820743996,0.641165742156689,
0.555265820743996,0.641165742156689,0.555265820743996,0.641165742156689,
0.555265820743996,0.641165742156689,0.555265820743996,0.641165742156689,
0.555265820743996,0.641165742156689,0.555265820743996,0.641165742156689,
0.555265820743996,0.641165742156689,0.555265820743996,0.641165742156689,
0.555265820743996,0.641165742156689,0.555265820743996,0.641165742156689,
0.555265820743996,0.641165742156689,0.555265820743996,0.641165742156689,
0.555265820743996,0.641165742156689,0.555265820743996,0.641165742156689,
0.555265820743996,0.641165742156689,0.555265820743996,0.641165742156689,
0.555265820743996,0.641165742156689,0.555265820743996,0.641165742156689,
0.555265820743996,0.641165742156689,0.555265820743996,0.641165742156689,
0.555265820743996,0.641165742156689,0.555265820743996,0.641165742156689,
0.555265820743996,0.641165742156689,0.555265820743996,0.641165742156689,
0.555265820743996,0.641165742156689,0.555265820743996,0.641165742156689,
0.555265820743996,0.641165742156689,0.555265820743996,0.641165742156689,
0.555265820743996,0.641165742156689,0.555265820743996,0.641165742156689,
0.555265820743996,0.641165742156689,0.555265820743996,0.641165742156689,
0.555265820743996,0.641165742156689,0.555265820743996,0.641165742156689,
0.555265820743996,0.641165742156689,0.555265820743996,0.641165742156689,
0.555265820743996,0.641165742156689,0.555265820743996,0.641165742156689,
0.555265820743996,0.641165742156689,0.555265820743996,0.641165742156689,
0.555265820743996,0.641165742156689,0.555265820743996,0.641165742156689,
0.555265820743996,0.641165742156689,0.555265820743996,0.641165742156689,
0.555265820743996,0.641165742156689,0.555265820743996,0.641165742156689,
0.555265820743996,0.641165742156689,0.555265820743996,0.641165742156689,
0.555265820743996,0.641165742156689,0.555265820743996,0.641165742156689,
0.555265820743996,0.641165742156689,0.555265820743996,0.641165742156689,
0.555265820743996,0.641165742156689,0.555265820743996,0.641165742156689,
0.555265820743996,0.641165742156689,0.555265820743996,0.641165742156689,
0.555265820743996,0.641165742156689,0.555265820743996,0.641165742156689,
0.555265820743996,0.641165742156689,0.555265820743996,0.641165742156689,
0.555265820743996,0.641165742156689,0.555265820743996,0.641165742156689,
0.555265820743996,0.641165742156689,0.555265820743996,0.641165742156689,
0.555265820743996,0.641165742156689,0.555265820743996,0.641165742156689,
0.555265820743996,0.641165742156689,0.555265820743996,0.641165742156689,
0.555265820743996,0.641165742156689,0.555265820743996,0.641165742156689,
0.555265820743996,0.641165742156689,0.555265820743996,0.641165742156689,
0.555265820743996,0.641165742156689,0.555265820743996,0.641165742156689,
0.555265820743996,0.641165742156689,0.555265820743996,0.641165742156689,
0.555265820743996,0.641165742156689,0.555265820743996,0.641165742156689,
0.555265820743996,0.641165742156689,0.555265820743996,0.641165742156689,
0.555265820743996,0.641165742156689,0.555265820743996,0.641165742156689,
0.555265820743996,0.641165742156689,0.555265820743996,0.641165742156689,
0.555265820743996,0.641165742156689,0.555265820743996,0.641165742156689,
0.555265820743996,0.641165742156689,0.555265820743996,0.641165742156689,
0.555265820743996,0.641165742156689,0.555265820743996,0.641165742156689,
0.555265820743996,0.641165742156689,0.555265820743996,0.641165742156689,
0.555265820743996,0.641165742156689,0.555265820743996,0.641165742156689,
0.555265820743996,0.641165742156689,0.555265820743996,0.641165742156689,
0.555265820743996,0.641165742156689,0.555265820743996,0.641165742156689,
0.555265820743996,0.641165742156689,0.555265820743996,0.641165742156689,
0.555265820743996,0.641165742156689,0.555265820743996,0.641165742156689,
0.555265820743996,0.641165742156689,0.555265820743996,0.641165742156689,
0.555265820743996,0.641165742156689,0.555265820743996,0.641165742156689,
0.555265820743996,0.641165742156689,0.555265820743996,0.641165742156689,
0.555265820743996,0.641165742156689,0.555265820743996,0.641165742156689,
0.555265820743996,0.641165742156689,0.555265820743996,0.641165742156689,
0.555265820743996,0.641165742156689,0.555265820743996,0.641165742156689,
0.555265820743996,0.641165742156689,0.555265820743996,0.641165742156689,
0.555265820743996,0.641165742156689,0.555265820743996,0.641165742156689,
0.555265820743996,0.641165742156689,0.555265820743996,0.641165742156689,
0.555265820743996,0.641165742156689,0.555265820743996,0.641165742156689,
0.555265820743996,0.641165742156689,0.555265820743996,0.641165742156689,
0.555265820743996,0.641165742156689,0.555265820743996,0.641165742156689,
0.555265820743996,0.641165742156689,0.555265820743996,0.641165742156689,
0.555265820743996,0.641165742156689,0.555265820743996,0.641165742156689,
0.555265820743996,0.641165742156689,0.555265820743996,0.641165742156689,
0.555265820743996,0.641165742156689,0.555265820743996,0.641165742156689,
0.555265820743996,0.641165742156689,0.555265820743996,0.641165742156689,
0.555265820743996,0.641165742156689,0.555265820743996,0.641165742156689,
0.555265820743996,0.641165742156689,0.555265820743996,0.641165742156689,
0.555265820743996,0.641165742156689,0.555265820743996,0.641165742156689,
0.555265820743996,0.641165742156689,0.555265820743996,0.641165742156689,
0.555265820743996,0.641165742156689,0.555265820743996,0.641165742156689,
0.555265820743996,0.641165742156689,0.555265820743996,0.641165742156689,
0.555265820743996,0.641165742156689,0.555265820743996,0.641165742156689,
0.555265820743996,0.641165742156689,0.555265820743996,0.641165742156689,
0.555265820743996,0.641165742156689,0.555265820743996,0.641165742156689,
0.555265820743996,0.641165742156689,0.555265820743996,0.641165742156689,
0.555265820743996,0.641165742156689,0.555265820743996,0.641165742156689,
0.555265820743996,0.641165742156689,0.555265820743996,0.641165742156689,
0.555265820743996,0.641165742156689,0.555265820743996,0.641165742156689,
0.555265820743996,0.641165742156689,0.555265820743996,0.641165742156689,
0.555265820743996,0.641165742156689,0.555265820743996,0.641165742156689,
0.555265820743996,0.641165742156689,0.555265820743996,0.641165742156689,
0.555265820743996,0.641165742156689,0.555265820743996,0.641165742156689,
0.555265820743996,0.641165742156689,0.555265820743996,0.641165742156689,
0.555265820743996,0.641165742156689,0.555265820743996,0.641165742156689,
0.555265820743996,0.641165742156689,0.555265820743996,0.641165742156689,
0.555265820743996,0.641165742156689,0.555265820743996,0.641165742156689,
0.555265820743996,0.641165742156689,0.555265820743996,0.641165742156689,
0.555265820743996,0.641165742156689),(1.,0.866025403784439,1.,0.866025403784439,
1.,0.866025403784439,1.,0.866025403784439,1.,0.866025403784439,1.,0.866025403784439,
1.,0.866025403784439,1.,0.866025403784439,1.,0.866025403784439,1.,0.866025403784439,
1.,0.866025403784439,1.,0.866025403784439,1.,0.866025403784439,1.,0.866025403784439,
1.,0.866025403784439,1.,0.866025403784439,1.,0.866025403784439,1.,0.866025403784439,
1.,0.866025403784439,1.,0.866025403784439,1.,0.866025403784439,1.,0.866025403784439,
1.,0.866025403784439,1.,0.866025403784439,1.,0.866025403784439,1.,0.866025403784439,
1.,0.866025403784439,1.,0.866025403784439,1.,0.866025403784439,1.,0.866025403784439,
1.,0.866025403784439,1.,0.866025403784439,1.,0.866025403784439,1.,0.866025403784439,
1.,0.866025403784439,1.,0.866025403784439,1.,0.866025403784439,1.,0.866025403784439,
1.,0.866025403784439,1.,0.866025403784439,1.,0.866025403784439,1.,0.866025403784439,
1.,0.866025403784439,1.,0.866025403784439,1.,0.866025403784439,1.,0.866025403784439,
1.,0.866025403784439,1.,0.866025403784439,1.,0.866025403784439,1.,0.866025403784439,
1.,0.866025403784439,1.,0.866025403784439,1.,0.866025403784439,1.,0.866025403784439,
1.,0.866025403784439,1.,0.866025403784439,1.,0.866025403784439,1.,0.866025403784439,
1.,0.866025403784439,1.,0.866025403784439,1.,0.866025403784439,1.,0.866025403784439,
1.,0.866025403784439,1.,0.866025403784439,1.,0.866025403784439,1.,0.866025403784439,
1.,0.866025403784439,1.,0.866025403784439,1.,0.866025403784439,1.,0.866025403784439,
1.,0.866025403784439,1.,0.866025403784439,1.,0.866025403784439,1.,0.866025403784439,
1.,0.866025403784439,1.,0.866025403784439,1.,0.866025403784439,1.,0.866025403784439,
1.,0.866025403784439,1.,0.866025403784439,1.,0.866025403784439,1.,0.866025403784439,
1.,0.866025403784439,1.,0.866025403784439,1.,0.866025403784439,1.,0.866025403784439,
1.,0.866025403784439,1.,0.866025403784439,1.,0.866025403784439,1.,0.866025403784439,
1.,0.866025403784439,1.,0.866025403784439,1.,0.866025403784439,1.,0.866025403784439,
1.,0.866025403784439,1.,0.866025403784439,1.,0.866025403784439,1.,0.866025403784439,
1.,0.866025403784439,1.,0.866025403784439,1.,0.866025403784439,1.,0.866025403784439,
1.,0.866025403784439,1.,0.866025403784439,1.,0.866025403784439,1.,0.866025403784439,
1.,0.866025403784439,1.,0.866025403784439,1.,0.866025403784439,1.,0.866025403784439,
1.,0.866025403784439,1.,0.866025403784439,1.,0.866025403784439,1.,0.866025403784439,
1.,0.866025403784439,1.,0.866025403784439,1.,0.866025403784439,1.,0.866025403784439,
1.,0.866025403784439,1.,0.866025403784439,1.,0.866025403784439,1.,0.866025403784439,
1.,0.866025403784439,1.,0.866025403784439,1.,0.866025403784439,1.,0.866025403784439,
1.,0.866025403784439,1.,0.866025403784439,1.,0.866025403784439,1.,0.866025403784439,
1.,0.866025403784439,1.,0.866025403784439,1.,0.866025403784439,1.,0.866025403784439,
1.,0.866025403784439,1.,0.866025403784439,1.,0.866025403784439,1.,0.866025403784439,
1.,0.866025403784439,1.,0.866025403784439,1.,0.866025403784439,1.,0.866025403784439,
1.,0.866025403784439,1.,0.866025403784439,1.,0.866025403784439,1.,0.866025403784439,
1.,0.866025403784439,1.,0.866025403784439,1.,0.866025403784439,1.,0.866025403784439,
1.,0.866025403784439,1.,0.866025403784439,1.,0.866025403784439,1.,0.866025403784439,
1.,0.866025403784439,1.,0.866025403784439,1.,0.866025403784439,1.,0.866025403784439,
1.,0.866025403784439,1.,0.866025403784439,1.,0.866025403784439,1.,0.866025403784439,
1.,0.866025403784439,1.,0.866025403784439,1.,0.866025403784439,1.,0.866025403784439,
1.,0.866025403784439,1.,0.866025403784439,1.,0.866025403784439,1.,0.866025403784439,
1.,0.866025403784439,1.,0.866025403784439,1.,0.866025403784439,1.,0.866025403784439,
1.,0.866025403784439,1.,0.866025403784439,1.,0.866025403784439,1.,0.866025403784439,
1.,0.866025403784439,1.,0.866025403784439,1.,0.866025403784439,1.,0.866025403784439,
1.,0.866025403784439,1.,0.866025403784439,1.,0.866025403784439,1.,0.866025403784439,
1.,0.866025403784439,1.,0.866025403784439,1.,0.866025403784439,1.,0.866025403784439,
1.,0.866025403784439,1.,0.866025403784439,1.,0.866025403784439,1.,0.866025403784439,
1.,0.866025403784439,1.,0.866025403784439,1.,0.866025403784439,1.,0.866025403784439,
1.,0.866025403784439,1.,0.866025403784439,1.,0.866025403784439,1.,0.866025403784439,
1.,0.866025403784439,1.,0.866025403784439,1.,0.866025403784439,1.,0.866025403784439,
1.,0.866025403784439,1.,0.866025403784439,1.,0.866025403784439,1.,0.866025403784439,
1.,0.866025403784439,1.,0.866025403784439,1.,0.866025403784439,1.,0.866025403784439,
1.,0.866025403784439,1.,0.866025403784439,1.,0.866025403784439,1.,0.866025403784439,
1.,0.866025403784439,1.,0.866025403784439,1.,0.866025403784439,1.,0.866025403784439,
1.,0.866025403784439,1.,0.866025403784439,1.,0.866025403784439,1.,0.866025403784439,
1.,0.866025403784439,1.,0.866025403784439,1.,0.866025403784439,1.,0.866025403784439,
1.,0.866025403784439,1.,0.866025403784439,1.,0.866025403784439,1.,0.866025403784439,
1.,0.866025403784439,1.,0.866025403784439,1.,0.866025403784439,1.,0.866025403784439,
1.,0.866025403784439,1.,0.866025403784439,1.,0.866025403784439,1.,0.866025403784439,
1.,0.866025403784439,1.,0.866025403784439,1.,0.866025403784439,1.,0.866025403784439,
1.,0.866025403784439,1.,0.866025403784439,1.,0.866025403784439,1.,0.866025403784439,
1.,0.866025403784439,1.,0.866025403784439,1.,0.866025403784439,1.,0.866025403784439,
1.,0.866025403784439,1.,0.866025403784439,1.,0.866025403784439,1.,0.866025403784439,
1.,0.866025403784439,1.,0.866025403784439,1.,0.866025403784439,1.,0.866025403784439,
1.,0.866025403784439,1.,0.866025403784439,1.,0.866025403784439,1.,0.866025403784439,
1.,0.866025403784439,1.,0.866025403784439,1.,0.866025403784439,1.,0.866025403784439,
1.,0.866025403784439,1.,0.866025403784439,1.,0.866025403784439,1.,0.866025403784439,
1.,0.866025403784439,1.,0.866025403784439,1.,0.866025403784439,1.,0.866025403784439,
1.,0.866025403784439,1.,0.866025403784439,1.,0.866025403784439,1.,0.866025403784439,
1.,0.866025403784439,1.,0.866025403784439,1.,0.866025403784439,1.,0.866025403784439,
1.,0.866025403784439,1.,0.866025403784439,1.,0.866025403784439,1.,0.866025403784439,
1.,0.866025403784439,1.,0.866025403784439,1.,0.866025403784439,1.,0.866025403784439,
1.,0.866025403784439,1.,0.866025403784439,1.,0.866025403784439,1.,0.866025403784439,
1.,0.866025403784439,1.,0.866025403784439,1.,0.866025403784439,1.,0.866025403784439,
1.,0.866025403784439,1.,0.866025403784439,1.,0.866025403784439,1.,0.866025403784439,
1.,0.866025403784439,1.,0.866025403784439,1.,0.866025403784439,1.,0.866025403784439,
1.,0.866025403784439,1.,0.866025403784439,1.,0.866025403784439,1.,0.866025403784439,
1.,0.866025403784439,1.,0.866025403784439,1.,0.866025403784439,1.,0.866025403784439,
1.,0.866025403784439,1.,0.866025403784439,1.,0.866025403784439,1.,0.866025403784439,
1.,0.866025403784439,1.,0.866025403784439,1.,0.866025403784439,1.,0.866025403784439,
1.,0.866025403784439,1.,0.866025403784439,1.,0.866025403784439,1.,0.866025403784439,
1.,0.866025403784439,1.,0.866025403784439,1.,0.866025403784439,1.,0.866025403784439,
1.,0.866025403784439,1.,0.866025403784439,1.,0.866025403784439,1.,0.866025403784439,
1.,0.866025403784439,1.,0.866025403784439,1.,0.866025403784439,1.,0.866025403784439,
1.,0.866025403784439,1.,0.866025403784439,1.,0.866025403784439,1.,0.866025403784439,
1.,0.866025403784439,1.,0.866025403784439,1.,0.866025403784439,1.,0.866025403784439,
1.,0.866025403784439,1.,0.866025403784439,1.,0.866025403784439,1.,0.866025403784439,
1.,0.866025403784439,1.,0.866025403784439,1.,0.866025403784439,1.,0.866025403784439,
1.,0.866025403784439,1.,0.866025403784439,1.,0.866025403784439,1.,0.866025403784439,
1.,0.866025403784439,1.,0.866025403784439,1.,0.866025403784439,1.,0.866025403784439,
1.,0.866025403784439,1.,0.866025403784439,1.,0.866025403784439,1.,0.866025403784439,
1.,0.866025403784439,1.,0.866025403784439,1.,0.866025403784439,1.,0.866025403784439,
1.,0.866025403784439,1.,0.866025403784439,1.,0.866025403784439,1.,0.866025403784439,
1.,0.866025403784439,1.,0.866025403784439,1.,0.866025403784439,1.,0.866025403784439,
1.,0.866025403784439,1.,0.866025403784439,1.,0.866025403784439,1.,0.866025403784439,
1.,0.866025403784439,1.,0.866025403784439,1.,0.866025403784439,1.,0.866025403784439,
1.,0.866025403784439,1.,0.866025403784439,1.,0.866025403784439,1.,0.866025403784439,
1.,0.866025403784439,1.,0.866025403784439,1.,0.866025403784439,1.,0.866025403784439,
1.,0.866025403784439,1.,0.866025403784439,1.,0.866025403784439,1.,0.866025403784439,
1.,0.866025403784439,1.,0.866025403784439,1.,0.866025403784439,1.,0.866025403784439,
1.,0.866025403784439,1.,0.866025403784439,1.,0.866025403784439,1.,0.866025403784439,
1.,0.866025403784439,1.,0.866025403784439,1.,0.866025403784439,1.,0.866025403784439,
1.,0.866025403784439,1.,0.866025403784439,1.,0.866025403784439,1.,0.866025403784439,
1.,0.866025403784439,1.,0.866025403784439,1.,0.866025403784439,1.,0.866025403784439,
1.,0.866025403784439,1.,0.866025403784439,1.,0.866025403784439,1.,0.866025403784439,
1.,0.866025403784439,1.,0.866025403784439,1.,0.866025403784439,1.,0.866025403784439,
1.,0.866025403784439,1.,0.866025403784439,1.,0.866025403784439,1.,0.866025403784439,
1.,0.866025403784439,1.,0.866025403784439,1.,0.866025403784439,1.,0.866025403784439,
1.,0.866025403784439,1.,0.866025403784439,1.,0.866025403784439,1.,0.866025403784439,
1.,0.866025403784439,1.,0.866025403784439,1.,0.866025403784439,1.,0.866025403784439,
1.,0.866025403784439,1.,0.866025403784439,1.,0.866025403784439,1.,0.866025403784439,
1.,0.866025403784439,1.,0.866025403784439,1.,0.866025403784439,1.,0.866025403784439,
1.,0.866025403784439,1.,0.866025403784439,1.,0.866025403784439,1.,0.866025403784439,
1.,0.866025403784439,1.,0.866025403784439,1.,0.866025403784439,1.,0.866025403784439,
1.,0.866025403784439,1.,0.866025403784439,1.,0.866025403784439,1.,0.866025403784439,
1.,0.866025403784439,1.,0.866025403784439,1.,0.866025403784439,1.,0.866025403784439,
1.,0.866025403784439,1.,0.866025403784439,1.,0.866025403784439,1.,0.866025403784439,
1.,0.866025403784439,1.,0.866025403784439,1.,0.866025403784439,1.,0.866025403784439,
1.,0.866025403784439,1.,0.866025403784439,1.,0.866025403784439,1.,0.866025403784439,
1.,0.866025403784439,1.,0.866025403784439,1.,0.866025403784439,1.,0.866025403784439,
1.)))
REPRESENTATION_ITEM('')
SURFACE()
);
#152=(
BOUNDED_SURFACE()
B_SPLINE_SURFACE(3,2,((#25753,#25754,#25755),(#25756,#25757,#25758),(#25759,
#25760,#25761),(#25762,#25763,#25764),(#25765,#25766,#25767),(#25768,#25769,
#25770),(#25771,#25772,#25773),(#25774,#25775,#25776),(#25777,#25778,#25779),
(#25780,#25781,#25782),(#25783,#25784,#25785),(#25786,#25787,#25788)),
 .UNSPECIFIED.,.F.,.F.,.F.)
B_SPLINE_SURFACE_WITH_KNOTS((4,2,2,2,2,4),(3,3),(1.5707963267949,1.96349540849362,
2.35619449019234,2.74889357189107,2.94524311274043,3.14159265358979),(0.,
1.),.UNSPECIFIED.)
GEOMETRIC_REPRESENTATION_ITEM()
RATIONAL_B_SPLINE_SURFACE(((1.,1.,1.),(1.,1.00006916239765,1.),(1.,0.995525209532845,
1.),(1.,0.979889883266457,1.),(1.,0.96878674661341,1.),(1.,0.945974626665763,
1.),(1.,0.934399279488173,1.),(1.,0.921892172356123,1.),(1.,0.918525872087786,
1.),(1.,0.913964997467621,1.),(1.,0.912767252466787,1.),(1.,0.912773552586276,
1.)))
REPRESENTATION_ITEM('')
SURFACE()
);
#153=(
BOUNDED_SURFACE()
B_SPLINE_SURFACE(3,2,((#25861,#25862,#25863),(#25864,#25865,#25866),(#25867,
#25868,#25869),(#25870,#25871,#25872)),.UNSPECIFIED.,.F.,.F.,.F.)
B_SPLINE_SURFACE_WITH_KNOTS((4,4),(3,3),(0.,0.00117394043814937),(0.,1.),
 .UNSPECIFIED.)
GEOMETRIC_REPRESENTATION_ITEM()
RATIONAL_B_SPLINE_SURFACE(((1.,0.707106781186547,1.),(1.,0.716249811896345,
1.),(1.,0.725602237863733,1.),(1.,0.73518030613814,1.)))
REPRESENTATION_ITEM('')
SURFACE()
);
#154=(
BOUNDED_SURFACE()
B_SPLINE_SURFACE(3,2,((#25874,#25875,#25876),(#25877,#25878,#25879),(#25880,
#25881,#25882),(#25883,#25884,#25885),(#25886,#25887,#25888),(#25889,#25890,
#25891),(#25892,#25893,#25894),(#25895,#25896,#25897),(#25898,#25899,#25900),
(#25901,#25902,#25903),(#25904,#25905,#25906),(#25907,#25908,#25909),(#25910,
#25911,#25912),(#25913,#25914,#25915)),.UNSPECIFIED.,.F.,.F.,.F.)
B_SPLINE_SURFACE_WITH_KNOTS((4,2,2,2,2,2,4),(3,3),(0.00114691688133867,
0.00238785904737931,0.00362880121341995,0.00486974337946059,0.00611068554550123,
0.0085925698775825,0.0110744542096638),(0.,1.),.UNSPECIFIED.)
GEOMETRIC_REPRESENTATION_ITEM()
RATIONAL_B_SPLINE_SURFACE(((1.,0.73518030613814,1.),(1.,0.747335275388272,
1.),(1.,0.761871430108272,1.),(1.,0.792538055362494,1.),(1.,0.808614330671284,
1.),(1.,0.840725708343004,1.),(1.,0.856795297690254,1.),(1.,0.887571556502581,
1.),(1.,0.902056904395603,1.),(1.,0.941769515107707,1.),(1.,0.963202620969872,
1.),(1.,0.992355658691941,1.),(1.,1.00006184400175,1.),(1.,1.,1.)))
REPRESENTATION_ITEM('')
SURFACE()
);
#155=(
BOUNDED_SURFACE()
B_SPLINE_SURFACE(3,2,((#25992,#25993,#25994),(#25995,#25996,#25997),(#25998,
#25999,#26000),(#26001,#26002,#26003),(#26004,#26005,#26006),(#26007,#26008,
#26009),(#26010,#26011,#26012),(#26013,#26014,#26015),(#26016,#26017,#26018),
(#26019,#26020,#26021),(#26022,#26023,#26024),(#26025,#26026,#26027)),
 .UNSPECIFIED.,.F.,.F.,.F.)
B_SPLINE_SURFACE_WITH_KNOTS((4,2,2,2,2,4),(3,3),(1.5707963267949,1.96349540849362,
2.35619449019234,2.74889357189107,2.94524311274043,3.14159265358979),(0.,
1.),.UNSPECIFIED.)
GEOMETRIC_REPRESENTATION_ITEM()
RATIONAL_B_SPLINE_SURFACE(((1.,1.,1.),(1.,1.00006916239765,1.),(1.,0.995525209532845,
1.),(1.,0.979889883266457,1.),(1.,0.968786746613379,1.),(1.,0.945974626665793,
1.),(1.,0.934399279488203,1.),(1.,0.921892172356108,1.),(1.,0.918525872087757,
1.),(1.,0.91396499746765,1.),(1.,0.912767252466765,1.),(1.,0.912773552586276,
1.)))
REPRESENTATION_ITEM('')
SURFACE()
);
#156=(
BOUNDED_SURFACE()
B_SPLINE_SURFACE(3,2,((#26100,#26101,#26102),(#26103,#26104,#26105),(#26106,
#26107,#26108),(#26109,#26110,#26111)),.UNSPECIFIED.,.F.,.F.,.F.)
B_SPLINE_SURFACE_WITH_KNOTS((4,4),(3,3),(-3.46944695195361E-18,0.00117394043814936),
(0.,1.),.UNSPECIFIED.)
GEOMETRIC_REPRESENTATION_ITEM()
RATIONAL_B_SPLINE_SURFACE(((1.,0.707106781186547,1.),(1.,0.716249811896345,
1.),(1.,0.725602237863732,1.),(1.,0.73518030613814,1.)))
REPRESENTATION_ITEM('')
SURFACE()
);
#157=(
BOUNDED_SURFACE()
B_SPLINE_SURFACE(3,2,((#26113,#26114,#26115),(#26116,#26117,#26118),(#26119,
#26120,#26121),(#26122,#26123,#26124),(#26125,#26126,#26127),(#26128,#26129,
#26130),(#26131,#26132,#26133),(#26134,#26135,#26136),(#26137,#26138,#26139),
(#26140,#26141,#26142),(#26143,#26144,#26145),(#26146,#26147,#26148),(#26149,
#26150,#26151),(#26152,#26153,#26154),(#26155,#26156,#26157),(#26158,#26159,
#26160)),.UNSPECIFIED.,.F.,.F.,.F.)
B_SPLINE_SURFACE_WITH_KNOTS((4,2,2,2,2,2,2,4),(3,3),(0.,0.00123568368061385,
0.00247136736122769,0.00370705104184154,0.00494273472245539,0.00617841840306923,
0.00741410208368308,0.00988546944491077),(0.,1.),.UNSPECIFIED.)
GEOMETRIC_REPRESENTATION_ITEM()
RATIONAL_B_SPLINE_SURFACE(((1.,0.73518030613814,1.),(1.,0.74764045440481,
1.),(1.,0.76189463212101,1.),(1.,0.792176992862199,1.),(1.,0.808203903859881,
1.),(1.,0.840503928826669,1.),(1.,0.856707888838066,1.),(1.,0.887226799422037,
1.),(1.,0.901676438639821,1.),(1.,0.928191888592131,1.),(1.,0.940260041314769,
1.),(1.,0.961420720965591,1.),(1.,0.970500238972907,1.),(1.,0.992409706176274,
1.),(1.,1.00002397099295,1.),(1.,1.,1.)))
REPRESENTATION_ITEM('')
SURFACE()
);
#158=(
BOUNDED_SURFACE()
B_SPLINE_SURFACE(3,2,((#26237,#26238,#26239),(#26240,#26241,#26242),(#26243,
#26244,#26245),(#26246,#26247,#26248),(#26249,#26250,#26251),(#26252,#26253,
#26254),(#26255,#26256,#26257),(#26258,#26259,#26260),(#26261,#26262,#26263),
(#26264,#26265,#26266),(#26267,#26268,#26269),(#26270,#26271,#26272)),
 .UNSPECIFIED.,.F.,.F.,.F.)
B_SPLINE_SURFACE_WITH_KNOTS((4,2,2,2,2,4),(3,3),(1.5707963267949,1.96349540849362,
2.35619449019234,2.74889357189107,2.94524311274043,3.14159265358979),(0.,
1.),.UNSPECIFIED.)
GEOMETRIC_REPRESENTATION_ITEM()
RATIONAL_B_SPLINE_SURFACE(((1.,1.,1.),(1.,1.00006916239765,1.),(1.,0.995525209532845,
1.),(1.,0.979889883266457,1.),(1.,0.968786746613379,1.),(1.,0.945974626665793,
1.),(1.,0.934399279488143,1.),(1.,0.921892172356137,1.),(1.,0.918525872087757,
1.),(1.,0.91396499746765,1.),(1.,0.912767252466764,1.),(1.,0.912773552586276,
1.)))
REPRESENTATION_ITEM('')
SURFACE()
);
#159=(
BOUNDED_SURFACE()
B_SPLINE_SURFACE(3,2,((#26345,#26346,#26347),(#26348,#26349,#26350),(#26351,
#26352,#26353),(#26354,#26355,#26356)),.UNSPECIFIED.,.F.,.F.,.F.)
B_SPLINE_SURFACE_WITH_KNOTS((4,4),(3,3),(0.,0.00117394043814937),(0.,1.),
 .UNSPECIFIED.)
GEOMETRIC_REPRESENTATION_ITEM()
RATIONAL_B_SPLINE_SURFACE(((1.,0.707106781186548,1.),(1.,0.716249811896345,
1.),(1.,0.725602237863732,1.),(1.,0.73518030613814,1.)))
REPRESENTATION_ITEM('')
SURFACE()
);
#160=(
BOUNDED_SURFACE()
B_SPLINE_SURFACE(3,2,((#26358,#26359,#26360),(#26361,#26362,#26363),(#26364,
#26365,#26366),(#26367,#26368,#26369),(#26370,#26371,#26372),(#26373,#26374,
#26375),(#26376,#26377,#26378),(#26379,#26380,#26381),(#26382,#26383,#26384),
(#26385,#26386,#26387),(#26388,#26389,#26390),(#26391,#26392,#26393),(#26394,
#26395,#26396),(#26397,#26398,#26399),(#26400,#26401,#26402),(#26403,#26404,
#26405)),.UNSPECIFIED.,.F.,.F.,.F.)
B_SPLINE_SURFACE_WITH_KNOTS((4,2,2,2,2,2,2,4),(3,3),(0.,0.00123568368061384,
0.00247136736122769,0.00370705104184153,0.00494273472245538,0.00617841840306922,
0.00741410208368307,0.00988546944491076),(0.,1.),.UNSPECIFIED.)
GEOMETRIC_REPRESENTATION_ITEM()
RATIONAL_B_SPLINE_SURFACE(((1.,0.73518030613814,1.),(1.,0.74764045440481,
1.),(1.,0.76189463212101,1.),(1.,0.792176992862198,1.),(1.,0.808203903859835,
1.),(1.,0.840503928826715,1.),(1.,0.856707888838066,1.),(1.,0.887226799422036,
1.),(1.,0.901676438639843,1.),(1.,0.928191888592107,1.),(1.,0.940260041314815,
1.),(1.,0.961420720965544,1.),(1.,0.970500238972907,1.),(1.,0.992409706176273,
1.),(1.,1.00002397099295,1.),(1.,1.,1.)))
REPRESENTATION_ITEM('')
SURFACE()
);
#161=(
BOUNDED_SURFACE()
B_SPLINE_SURFACE(3,2,((#26406,#26407,#26408),(#26409,#26410,#26411),(#26412,
#26413,#26414),(#26415,#26416,#26417),(#26418,#26419,#26420),(#26421,#26422,
#26423),(#26424,#26425,#26426),(#26427,#26428,#26429),(#26430,#26431,#26432),
(#26433,#26434,#26435),(#26436,#26437,#26438),(#26439,#26440,#26441),(#26442,
#26443,#26444),(#26445,#26446,#26447)),.UNSPECIFIED.,.F.,.F.,.F.)
B_SPLINE_SURFACE_WITH_KNOTS((4,2,2,2,2,2,4),(3,3),(0.00114691688133867,
0.00238785904737931,0.00362880121341995,0.00486974337946058,0.00611068554550122,
0.0085925698775825,0.0110744542096638),(0.,1.),.UNSPECIFIED.)
GEOMETRIC_REPRESENTATION_ITEM()
RATIONAL_B_SPLINE_SURFACE(((1.,0.73518030613814,1.),(1.,0.747335275388254,
1.),(1.,0.761871430108295,1.),(1.,0.79253805536247,1.),(1.,0.808614330671284,
1.),(1.,0.840725708343004,1.),(1.,0.856795297690208,1.),(1.,0.887571556502627,
1.),(1.,0.902056904395603,1.),(1.,0.941769515107708,1.),(1.,0.963202620969872,
1.),(1.,0.992355658691941,1.),(1.,1.00006184400175,1.),(1.,1.,1.)))
REPRESENTATION_ITEM('')
SURFACE()
);
#162=(
BOUNDED_SURFACE()
B_SPLINE_SURFACE(3,2,((#26449,#26450,#26451),(#26452,#26453,#26454),(#26455,
#26456,#26457),(#26458,#26459,#26460)),.UNSPECIFIED.,.F.,.F.,.F.)
B_SPLINE_SURFACE_WITH_KNOTS((4,4),(3,3),(0.,0.00117394043814936),(0.,1.),
 .UNSPECIFIED.)
GEOMETRIC_REPRESENTATION_ITEM()
RATIONAL_B_SPLINE_SURFACE(((1.,0.707106781186548,1.),(1.,0.716249811896344,
1.),(1.,0.725602237863733,1.),(1.,0.73518030613814,1.)))
REPRESENTATION_ITEM('')
SURFACE()
);
#163=(
BOUNDED_SURFACE()
B_SPLINE_SURFACE(3,2,((#26533,#26534,#26535),(#26536,#26537,#26538),(#26539,
#26540,#26541),(#26542,#26543,#26544),(#26545,#26546,#26547),(#26548,#26549,
#26550),(#26551,#26552,#26553),(#26554,#26555,#26556),(#26557,#26558,#26559),
(#26560,#26561,#26562),(#26563,#26564,#26565),(#26566,#26567,#26568)),
 .UNSPECIFIED.,.F.,.F.,.F.)
B_SPLINE_SURFACE_WITH_KNOTS((4,2,2,2,2,4),(3,3),(1.5707963267949,1.96349540849362,
2.35619449019234,2.74889357189107,2.94524311274043,3.14159265358979),(0.,
1.),.UNSPECIFIED.)
GEOMETRIC_REPRESENTATION_ITEM()
RATIONAL_B_SPLINE_SURFACE(((1.,1.,1.),(1.,1.00006916239762,1.),(1.,0.995525209532876,
1.),(1.,0.979889883266425,1.),(1.,0.968786746613409,1.),(1.,0.945974626665762,
1.),(1.,0.934399279488143,1.),(1.,0.921892172356137,1.),(1.,0.918525872087764,
1.),(1.,0.913964997467643,1.),(1.,0.912767252466769,1.),(1.,0.912773552586275,
1.)))
REPRESENTATION_ITEM('')
SURFACE()
);
#164=(
BOUNDED_SURFACE()
B_SPLINE_SURFACE(3,2,((#26571,#26572,#26573),(#26574,#26575,#26576),(#26577,
#26578,#26579),(#26580,#26581,#26582),(#26583,#26584,#26585),(#26586,#26587,
#26588),(#26589,#26590,#26591),(#26592,#26593,#26594),(#26595,#26596,#26597),
(#26598,#26599,#26600),(#26601,#26602,#26603),(#26604,#26605,#26606)),
 .UNSPECIFIED.,.F.,.F.,.F.)
B_SPLINE_SURFACE_WITH_KNOTS((4,2,2,2,2,4),(3,3),(1.5707963267949,1.96349540849362,
2.35619449019234,2.74889357189107,2.94524311274043,3.14159265358979),(0.,
1.),.UNSPECIFIED.)
GEOMETRIC_REPRESENTATION_ITEM()
RATIONAL_B_SPLINE_SURFACE(((1.,1.,1.),(1.,1.00006916239762,1.),(1.,0.995525209532877,
1.),(1.,0.979889883266426,1.),(1.,0.968786746613333,1.),(1.,0.945974626665839,
1.),(1.,0.934399279488187,1.),(1.,0.921892172356115,1.),(1.,0.918525872087757,
1.),(1.,0.91396499746765,1.),(1.,0.912767252466765,1.),(1.,0.912773552586276,
1.)))
REPRESENTATION_ITEM('')
SURFACE()
);
#165=(
BOUNDED_SURFACE()
B_SPLINE_SURFACE(3,2,((#26679,#26680,#26681),(#26682,#26683,#26684),(#26685,
#26686,#26687),(#26688,#26689,#26690)),.UNSPECIFIED.,.F.,.F.,.F.)
B_SPLINE_SURFACE_WITH_KNOTS((4,4),(3,3),(0.,0.00117394043814935),(0.,1.),
 .UNSPECIFIED.)
GEOMETRIC_REPRESENTATION_ITEM()
RATIONAL_B_SPLINE_SURFACE(((1.,0.707106781186548,1.),(1.,0.716249811896346,
1.),(1.,0.725602237863731,1.),(1.,0.73518030613814,1.)))
REPRESENTATION_ITEM('')
SURFACE()
);
#166=(
BOUNDED_SURFACE()
B_SPLINE_SURFACE(3,2,((#26692,#26693,#26694),(#26695,#26696,#26697),(#26698,
#26699,#26700),(#26701,#26702,#26703),(#26704,#26705,#26706),(#26707,#26708,
#26709),(#26710,#26711,#26712),(#26713,#26714,#26715),(#26716,#26717,#26718),
(#26719,#26720,#26721),(#26722,#26723,#26724),(#26725,#26726,#26727),(#26728,
#26729,#26730),(#26731,#26732,#26733),(#26734,#26735,#26736),(#26737,#26738,
#26739)),.UNSPECIFIED.,.F.,.F.,.F.)
B_SPLINE_SURFACE_WITH_KNOTS((4,2,2,2,2,2,2,4),(3,3),(0.,0.00123568368061385,
0.00247136736122769,0.00370705104184154,0.00494273472245539,0.00617841840306923,
0.00741410208368308,0.00988546944491077),(0.,1.),.UNSPECIFIED.)
GEOMETRIC_REPRESENTATION_ITEM()
RATIONAL_B_SPLINE_SURFACE(((1.,0.73518030613814,1.),(1.,0.747640454404809,
1.),(1.,0.76189463212101,1.),(1.,0.792176992862198,1.),(1.,0.808203903859881,
1.),(1.,0.840503928826668,1.),(1.,0.856707888838043,1.),(1.,0.887226799422059,
1.),(1.,0.901676438639843,1.),(1.,0.928191888592107,1.),(1.,0.940260041314768,
1.),(1.,0.96142072096559,1.),(1.,0.970500238972907,1.),(1.,0.992409706176274,
1.),(1.,1.00002397099295,1.),(1.,1.,1.)))
REPRESENTATION_ITEM('')
SURFACE()
);
#167=(
BOUNDED_SURFACE()
B_SPLINE_SURFACE(3,2,((#26740,#26741,#26742),(#26743,#26744,#26745),(#26746,
#26747,#26748),(#26749,#26750,#26751),(#26752,#26753,#26754),(#26755,#26756,
#26757),(#26758,#26759,#26760),(#26761,#26762,#26763),(#26764,#26765,#26766),
(#26767,#26768,#26769),(#26770,#26771,#26772),(#26773,#26774,#26775),(#26776,
#26777,#26778),(#26779,#26780,#26781)),.UNSPECIFIED.,.F.,.F.,.F.)
B_SPLINE_SURFACE_WITH_KNOTS((4,2,2,2,2,2,4),(3,3),(0.00114691688133867,
0.00238785904737931,0.00362880121341994,0.00486974337946058,0.00611068554550122,
0.0085925698775825,0.0110744542096638),(0.,1.),.UNSPECIFIED.)
GEOMETRIC_REPRESENTATION_ITEM()
RATIONAL_B_SPLINE_SURFACE(((1.,0.73518030613814,1.),(1.,0.747335275388254,
1.),(1.,0.761871430108295,1.),(1.,0.79253805536247,1.),(1.,0.808614330671261,
1.),(1.,0.840725708343027,1.),(1.,0.856795297690161,1.),(1.,0.887571556502673,
1.),(1.,0.90205690439558,1.),(1.,0.941769515107753,1.),(1.,0.963202620969917,
1.),(1.,0.992355658691895,1.),(1.,1.00006184400178,1.),(1.,1.,1.)))
REPRESENTATION_ITEM('')
SURFACE()
);
#168=(
BOUNDED_SURFACE()
B_SPLINE_SURFACE(3,2,((#26783,#26784,#26785),(#26786,#26787,#26788),(#26789,
#26790,#26791),(#26792,#26793,#26794)),.UNSPECIFIED.,.F.,.F.,.F.)
B_SPLINE_SURFACE_WITH_KNOTS((4,4),(3,3),(0.,0.00117394043814939),(0.,1.),
 .UNSPECIFIED.)
GEOMETRIC_REPRESENTATION_ITEM()
RATIONAL_B_SPLINE_SURFACE(((1.,0.707106781186547,1.),(1.,0.716249811896344,
1.),(1.,0.725602237863731,1.),(1.,0.73518030613814,1.)))
REPRESENTATION_ITEM('')
SURFACE()
);
#169=(
BOUNDED_SURFACE()
B_SPLINE_SURFACE(3,2,((#26867,#26868,#26869),(#26870,#26871,#26872),(#26873,
#26874,#26875),(#26876,#26877,#26878),(#26879,#26880,#26881),(#26882,#26883,
#26884),(#26885,#26886,#26887),(#26888,#26889,#26890),(#26891,#26892,#26893),
(#26894,#26895,#26896),(#26897,#26898,#26899),(#26900,#26901,#26902)),
 .UNSPECIFIED.,.F.,.F.,.F.)
B_SPLINE_SURFACE_WITH_KNOTS((4,2,2,2,2,4),(3,3),(1.5707963267949,1.96349540849362,
2.35619449019234,2.74889357189107,2.94524311274043,3.14159265358979),(0.,
1.),.UNSPECIFIED.)
GEOMETRIC_REPRESENTATION_ITEM()
RATIONAL_B_SPLINE_SURFACE(((1.,1.,1.),(1.,1.00006916239765,1.),(1.,0.995525209532845,
1.),(1.,0.979889883266457,1.),(1.,0.968786746613394,1.),(1.,0.945974626665778,
1.),(1.,0.934399279488158,1.),(1.,0.92189217235613,1.),(1.,0.918525872087771,
1.),(1.,0.913964997467635,1.),(1.,0.912767252466775,1.),(1.,0.912773552586276,
1.)))
REPRESENTATION_ITEM('')
SURFACE()
);
#170=(
BOUNDED_SURFACE()
B_SPLINE_SURFACE(3,2,((#26979,#26980,#26981),(#26982,#26983,#26984),(#26985,
#26986,#26987),(#26988,#26989,#26990),(#26991,#26992,#26993),(#26994,#26995,
#26996),(#26997,#26998,#26999),(#27000,#27001,#27002)),.UNSPECIFIED.,.F.,
 .F.,.F.)
B_SPLINE_SURFACE_WITH_KNOTS((4,2,2,4),(3,3),(0.,0.00109785791663237,0.00219571583326473,
0.00439143166652947),(0.,1.),.UNSPECIFIED.)
GEOMETRIC_REPRESENTATION_ITEM()
RATIONAL_B_SPLINE_SURFACE(((1.,0.707106781186549,1.),(1.,0.75082909814959,
1.),(1.,0.792349205138272,1.),(1.,0.866373214279049,1.),(1.,0.897828374333773,
1.),(1.,0.973720746971429,1.),(1.,1.00018625880497,1.),(1.,1.,1.)))
REPRESENTATION_ITEM('')
SURFACE()
);
#171=(
BOUNDED_SURFACE()
B_SPLINE_SURFACE(3,2,((#27018,#27019,#27020),(#27021,#27022,#27023),(#27024,
#27025,#27026),(#27027,#27028,#27029),(#27030,#27031,#27032),(#27033,#27034,
#27035),(#27036,#27037,#27038),(#27039,#27040,#27041)),.UNSPECIFIED.,.F.,
 .F.,.F.)
B_SPLINE_SURFACE_WITH_KNOTS((4,2,2,4),(3,3),(0.,0.00109785791663237,0.00219571583326474,
0.00439143166652948),(0.,1.),.UNSPECIFIED.)
GEOMETRIC_REPRESENTATION_ITEM()
RATIONAL_B_SPLINE_SURFACE(((1.,0.707106781186548,1.),(1.,0.75082909814959,
1.),(1.,0.792349205138269,1.),(1.,0.866373214279046,1.),(1.,0.897828374333914,
1.),(1.,0.973720746971144,1.),(1.,1.00018625880519,1.),(1.,1.,1.)))
REPRESENTATION_ITEM('')
SURFACE()
);
#172=(
BOUNDED_SURFACE()
B_SPLINE_SURFACE(3,2,((#27042,#27043,#27044),(#27045,#27046,#27047),(#27048,
#27049,#27050),(#27051,#27052,#27053),(#27054,#27055,#27056),(#27057,#27058,
#27059),(#27060,#27061,#27062),(#27063,#27064,#27065)),.UNSPECIFIED.,.F.,
 .F.,.F.)
B_SPLINE_SURFACE_WITH_KNOTS((4,2,2,4),(3,3),(0.,0.00109785791663237,0.00219571583326473,
0.00439143166652947),(0.,1.),.UNSPECIFIED.)
GEOMETRIC_REPRESENTATION_ITEM()
RATIONAL_B_SPLINE_SURFACE(((1.,0.707106781186548,1.),(1.,0.750829098149542,
1.),(1.,0.79234920513833,1.),(1.,0.866373214278985,1.),(1.,0.897828374333792,
1.),(1.,0.973720746971387,1.),(1.,1.000186258805,1.),(1.,1.,1.)))
REPRESENTATION_ITEM('')
SURFACE()
);
#173=(
BOUNDED_SURFACE()
B_SPLINE_SURFACE(3,2,((#27081,#27082,#27083),(#27084,#27085,#27086),(#27087,
#27088,#27089),(#27090,#27091,#27092),(#27093,#27094,#27095),(#27096,#27097,
#27098),(#27099,#27100,#27101),(#27102,#27103,#27104)),.UNSPECIFIED.,.F.,
 .F.,.F.)
B_SPLINE_SURFACE_WITH_KNOTS((4,2,2,4),(3,3),(0.,0.00109785791663236,0.00219571583326473,
0.00439143166652946),(0.,1.),.UNSPECIFIED.)
GEOMETRIC_REPRESENTATION_ITEM()
RATIONAL_B_SPLINE_SURFACE(((1.,0.707106781186548,1.),(1.,0.750829098149437,
1.),(1.,0.792349205138475,1.),(1.,0.866373214278842,1.),(1.,0.897828374333691,
1.),(1.,0.973720746971589,1.),(1.,1.00018625880485,1.),(1.,1.,1.)))
REPRESENTATION_ITEM('')
SURFACE()
);
#174=(
BOUNDED_SURFACE()
B_SPLINE_SURFACE(3,2,((#27105,#27106,#27107),(#27108,#27109,#27110),(#27111,
#27112,#27113),(#27114,#27115,#27116),(#27117,#27118,#27119),(#27120,#27121,
#27122),(#27123,#27124,#27125),(#27126,#27127,#27128)),.UNSPECIFIED.,.F.,
 .F.,.F.)
B_SPLINE_SURFACE_WITH_KNOTS((4,2,2,4),(3,3),(0.,0.00109785791663237,0.00219571583326474,
0.00439143166652948),(0.,1.),.UNSPECIFIED.)
GEOMETRIC_REPRESENTATION_ITEM()
RATIONAL_B_SPLINE_SURFACE(((1.,0.707106781186548,1.),(1.,0.750829098149496,
1.),(1.,0.792349205138392,1.),(1.,0.866373214278923,1.),(1.,0.897828374333732,
1.),(1.,0.973720746971509,1.),(1.,1.00018625880491,1.),(1.,1.,1.)))
REPRESENTATION_ITEM('')
SURFACE()
);
#175=(
BOUNDED_SURFACE()
B_SPLINE_SURFACE(3,2,((#27141,#27142,#27143),(#27144,#27145,#27146),(#27147,
#27148,#27149),(#27150,#27151,#27152),(#27153,#27154,#27155),(#27156,#27157,
#27158),(#27159,#27160,#27161),(#27162,#27163,#27164)),.UNSPECIFIED.,.F.,
 .F.,.F.)
B_SPLINE_SURFACE_WITH_KNOTS((4,2,2,4),(3,3),(-7.58941520739853E-19,0.00109785791663237,
0.00219571583326474,0.00439143166652947),(0.,1.),.UNSPECIFIED.)
GEOMETRIC_REPRESENTATION_ITEM()
RATIONAL_B_SPLINE_SURFACE(((1.,0.707106781186548,1.),(1.,0.750829098149468,
1.),(1.,0.792349205138434,1.),(1.,0.866373214278884,1.),(1.,0.897828374333793,
1.),(1.,0.973720746971388,1.),(1.,1.000186258805,1.),(1.,1.,1.)))
REPRESENTATION_ITEM('')
SURFACE()
);
#176=(
BOUNDED_SURFACE()
B_SPLINE_SURFACE(3,2,((#27166,#27167,#27168),(#27169,#27170,#27171),(#27172,
#27173,#27174),(#27175,#27176,#27177),(#27178,#27179,#27180),(#27181,#27182,
#27183),(#27184,#27185,#27186),(#27187,#27188,#27189),(#27190,#27191,#27192),
(#27193,#27194,#27195),(#27196,#27197,#27198),(#27199,#27200,#27201),(#27202,
#27203,#27204),(#27205,#27206,#27207),(#27208,#27209,#27210),(#27211,#27212,
#27213),(#27214,#27215,#27216),(#27217,#27218,#27219),(#27220,#27221,#27222),
(#27223,#27224,#27225),(#27226,#27227,#27228),(#27229,#27230,#27231),(#27232,
#27233,#27234),(#27235,#27236,#27237),(#27238,#27239,#27240),(#27241,#27242,
#27243),(#27244,#27245,#27246),(#27247,#27248,#27249),(#27250,#27251,#27252),
(#27253,#27254,#27255),(#27256,#27257,#27258),(#27259,#27260,#27261),(#27262,
#27263,#27264),(#27265,#27266,#27267),(#27268,#27269,#27270),(#27271,#27272,
#27273),(#27274,#27275,#27276),(#27277,#27278,#27279),(#27280,#27281,#27282),
(#27283,#27284,#27285),(#27286,#27287,#27288),(#27289,#27290,#27291)),
 .UNSPECIFIED.,.F.,.F.,.F.)
B_SPLINE_SURFACE_WITH_KNOTS((4,2,2,2,2,2,2,2,2,2,2,2,2,2,2,2,2,2,2,2,4),
(3,3),(-7.80561738159264E-5,0.00108972446965002,0.00217944893930003,0.00326917340895005,
0.00435889787860006,0.00490376011342507,0.00544862234825008,0.00653834681790009,
0.00762807128755011,0.00871779575720013,0.00926265799202513,0.00980752022685014,
0.0103523824616751,0.0108972446965002,0.0119869691661502,0.0130766936358002,
0.0141664181054502,0.0152561425751002,0.0158010048099252,0.0163458670447502,
0.0174687351854262),(-3.31436710259121E-5,1.00007805617382),
 .UNSPECIFIED.)
GEOMETRIC_REPRESENTATION_ITEM()
RATIONAL_B_SPLINE_SURFACE(((1.00003154503853,0.524079561564375,1.00007429459434),
(1.0000315937412,0.523344783661835,1.00007440929844),(1.00003141682542,
0.526013914411658,1.00007399262799),(1.0000307068602,0.536725169717461,
1.0000723205242),(1.00003019055673,0.544514647394406,1.00007110453086),
(1.00002895723913,0.563121727335801,1.00006819983221),(1.0000282411969,
0.573924666524174,1.00006651341591),(1.00002671338234,0.596974826160331,
1.00006291512064),(1.00002591662213,0.608995558662043,1.00006103859807),
(1.00002475586398,0.626507933141575,1.00005830479079),(1.00002437347723,
0.632277007329064,1.00005740419693),(1.00002362687254,0.643541042834223,
1.00005564580019),(1.00002326100253,0.649060928800113,1.00005478410639),
(1.00002222356725,0.664712729342052,1.00005234074805),(1.00002160723677,
0.674011315953667,1.00005088917198),(1.00002057219885,0.689626947600185,
1.00004845145987),(1.00002015115486,0.695979244110157,1.00004745982082),
(1.00001958356106,0.704542539723916,1.00004612302894),(1.00001943064549,
0.706849579098284,1.00004576288355),(1.00001940985656,0.707163222049774,
1.00004571392163),(1.00001943845365,0.706731777363891,1.00004578127324),
(1.00001956476706,0.704826085066601,1.00004607876548),(1.00001966207446,
0.703358006931155,1.00004630794301),(1.00001992151192,0.69944387046907,
1.00004691896779),(1.00002008365206,0.696997659863913,1.00004730083881),
(1.00002047017319,0.691166210187756,1.00004821116994),(1.00002069610127,
0.687757630052989,1.00004874327375),(1.00002145040546,0.676377432111549,
1.00005051980428),(1.00002205383492,0.667273483461506,1.00005194099597),
(1.00002340996085,0.646813592510669,1.00005513493171),(1.0000241670402,
0.635391525693089,1.00005691799827),(1.00002570900064,0.612127947016899,
1.00006054960978),(1.00002650093244,0.600180060818586,1.00006241476052),
(1.0000280417883,0.576933146876439,1.00006604377054),(1.00002877367107,
0.565891221185074,1.00006776749435),(1.00002972027581,0.551609782278378,
1.00006999692941),(1.0000300115584,0.547215197654337,1.00007068295559),
(1.00003053161739,0.53936906050514,1.00007190779388),(1.00003076145279,
0.535901530604989,1.00007244910017),(1.00003133743645,0.527211656986592,
1.00007380565178),(1.00003154549653,0.52407265171366,1.00007429567302),
(1.00003155264458,0.523964808953251,1.00007431250805)))
REPRESENTATION_ITEM('')
SURFACE()
);
#177=(
BOUNDED_SURFACE()
B_SPLINE_SURFACE(3,2,((#27578,#27579,#27580),(#27581,#27582,#27583),(#27584,
#27585,#27586),(#27587,#27588,#27589),(#27590,#27591,#27592),(#27593,#27594,
#27595),(#27596,#27597,#27598),(#27599,#27600,#27601),(#27602,#27603,#27604),
(#27605,#27606,#27607),(#27608,#27609,#27610),(#27611,#27612,#27613),(#27614,
#27615,#27616),(#27617,#27618,#27619),(#27620,#27621,#27622),(#27623,#27624,
#27625),(#27626,#27627,#27628),(#27629,#27630,#27631),(#27632,#27633,#27634),
(#27635,#27636,#27637),(#27638,#27639,#27640),(#27641,#27642,#27643),(#27644,
#27645,#27646),(#27647,#27648,#27649),(#27650,#27651,#27652),(#27653,#27654,
#27655),(#27656,#27657,#27658),(#27659,#27660,#27661),(#27662,#27663,#27664),
(#27665,#27666,#27667),(#27668,#27669,#27670),(#27671,#27672,#27673),(#27674,
#27675,#27676),(#27677,#27678,#27679),(#27680,#27681,#27682),(#27683,#27684,
#27685),(#27686,#27687,#27688),(#27689,#27690,#27691),(#27692,#27693,#27694),
(#27695,#27696,#27697),(#27698,#27699,#27700),(#27701,#27702,#27703)),
 .UNSPECIFIED.,.F.,.F.,.F.)
B_SPLINE_SURFACE_WITH_KNOTS((4,2,2,2,2,2,2,2,2,2,2,2,2,2,2,2,2,2,2,2,4),
(3,3),(0.,0.00108936814645749,0.00217873629291499,0.00326810443937248,0.00435747258582998,
0.00490215665905872,0.00544684073228747,0.00653620887874497,0.00762557702520246,
0.00871494517165995,0.0092596292448887,0.00980431331811745,0.0103489973913462,
0.0108936814645749,0.0119830496110324,0.0130724177574899,0.0141617859039474,
0.0152511540504049,0.0157958381236337,0.0163405221968624,0.0174298903433199),
(0.,1.),.UNSPECIFIED.)
GEOMETRIC_REPRESENTATION_ITEM()
RATIONAL_B_SPLINE_SURFACE(((1.,0.706882331541542,1.),(1.,0.707679638835941,
1.),(1.,0.706337831680188,1.),(1.,0.699641298231053,1.),(1.,0.694186850878167,
1.),(1.,0.680019624674915,1.),(1.,0.671327778173696,1.),(1.,0.65139771038903,
1.),(1.,0.640295384304893,1.),(1.,0.623043177807755,1.),(1.,0.617175274503255,
1.),(1.,0.605346721741376,1.),(1.,0.599355525156456,1.),(1.,0.581798773133271,
1.),(1.,0.570600832874572,1.),(1.,0.550711868458482,1.),(1.,0.541963614343013,
1.),(1.,0.529372137830182,1.),(1.,0.525443344962623,1.),(1.,0.523784577113156,
1.),(1.,0.523945004135255,1.),(1.,0.525692544902627,1.),(1.,0.527267041649223,
1.),(1.,0.531692982742457,1.),(1.,0.534544195639033,1.),(1.,0.541381698420683,
1.),(1.,0.545393688389137,1.),(1.,0.55869257877852,1.),(1.,0.569170005808865,
1.),(1.,0.591697019613681,1.),(1.,0.603798924645628,1.),(1.,0.6273058031179,
1.),(1.,0.638830492715536,1.),(1.,0.660348218640802,1.),(1.,0.670109592161733,
1.),(1.,0.682456253372296,1.),(1.,0.686205595551818,1.),(1.,0.692883150338747,
1.),(1.,0.695824965165441,1.),(1.,0.703162804007318,1.),(1.,0.706044886129699,
1.),(1.,0.706866009891837,1.)))
REPRESENTATION_ITEM('')
SURFACE()
);
#178=(
BOUNDED_SURFACE()
B_SPLINE_SURFACE(1,2,((#28772,#28773,#28774,#28775,#28776,#28777,#28778,
#28779,#28780,#28781,#28782,#28783,#28784,#28785,#28786,#28787,#28788,#28789,
#28790,#28791,#28792,#28793,#28794,#28795,#28796,#28797,#28798,#28799,#28800,
#28801,#28802,#28803,#28804,#28805,#28806,#28807,#28808,#28809,#28810,#28811,
#28812,#28813,#28814,#28815,#28816,#28817,#28818,#28819,#28820,#28821,#28822,
#28823,#28824,#28825,#28826,#28827,#28828,#28829,#28830,#28831,#28832,#28833,
#28834,#28835,#28836,#28837,#28838,#28839,#28840,#28841,#28842,#28843,#28844,
#28845,#28846,#28847,#28848,#28849,#28850,#28851,#28852,#28853,#28854,#28855,
#28856,#28857,#28858,#28859,#28860,#28861,#28862,#28863,#28864,#28865,#28866,
#28867,#28868,#28869,#28870,#28871,#28872,#28873,#28874,#28875,#28876,#28877,
#28878,#28879,#28880,#28881,#28882,#28883,#28884,#28885,#28886,#28887,#28888,
#28889,#28890,#28891,#28892,#28893,#28894,#28895,#28896,#28897,#28898,#28899,
#28900,#28901,#28902,#28903,#28904,#28905,#28906,#28907,#28908,#28909,#28910,
#28911,#28912,#28913,#28914,#28915,#28916,#28917,#28918,#28919,#28920,#28921,
#28922,#28923,#28924,#28925,#28926,#28927,#28928,#28929,#28930,#28931,#28932,
#28933,#28934,#28935,#28936,#28937,#28938,#28939,#28940,#28941,#28942,#28943,
#28944,#28945,#28946,#28947,#28948,#28949,#28950,#28951,#28952,#28953,#28954,
#28955,#28956,#28957,#28958,#28959,#28960,#28961,#28962,#28963,#28964,#28965,
#28966,#28967,#28968,#28969,#28970,#28971,#28972,#28973,#28974,#28975,#28976,
#28977,#28978,#28979,#28980,#28981,#28982,#28983,#28984,#28985,#28986,#28987,
#28988,#28989,#28990,#28991,#28992,#28993,#28994,#28995,#28996,#28997,#28998,
#28999,#29000,#29001,#29002,#29003,#29004,#29005,#29006,#29007,#29008,#29009,
#29010,#29011,#29012,#29013,#29014,#29015,#29016,#29017,#29018,#29019,#29020,
#29021,#29022,#29023,#29024,#29025,#29026,#29027,#29028,#29029,#29030,#29031,
#29032,#29033,#29034,#29035,#29036,#29037,#29038,#29039,#29040,#29041,#29042,
#29043,#29044,#29045,#29046,#29047,#29048,#29049,#29050,#29051,#29052,#29053,
#29054,#29055,#29056,#29057,#29058,#29059,#29060,#29061,#29062,#29063,#29064,
#29065,#29066,#29067,#29068,#29069,#29070,#29071,#29072,#29073,#29074,#29075,
#29076,#29077,#29078,#29079,#29080,#29081,#29082,#29083,#29084,#29085,#29086,
#29087,#29088,#29089,#29090,#29091,#29092,#29093,#29094,#29095,#29096,#29097,
#29098,#29099,#29100,#29101,#29102,#29103,#29104,#29105,#29106,#29107,#29108,
#29109,#29110,#29111,#29112,#29113,#29114,#29115,#29116,#29117,#29118,#29119,
#29120,#29121,#29122,#29123,#29124,#29125,#29126,#29127,#29128,#29129,#29130,
#29131,#29132,#29133,#29134,#29135,#29136,#29137,#29138,#29139,#29140,#29141,
#29142,#29143,#29144,#29145,#29146,#29147,#29148,#29149,#29150,#29151,#29152,
#29153,#29154,#29155,#29156,#29157,#29158,#29159,#29160,#29161,#29162,#29163,
#29164,#29165,#29166,#29167,#29168,#29169,#29170,#29171,#29172,#29173,#29174,
#29175,#29176,#29177,#29178,#29179,#29180,#29181,#29182,#29183,#29184,#29185,
#29186,#29187,#29188,#29189,#29190,#29191,#29192,#29193,#29194,#29195,#29196,
#29197,#29198,#29199,#29200,#29201,#29202,#29203,#29204,#29205,#29206,#29207,
#29208,#29209,#29210,#29211,#29212,#29213,#29214,#29215,#29216,#29217,#29218,
#29219,#29220,#29221,#29222,#29223,#29224,#29225,#29226,#29227,#29228,#29229,
#29230,#29231,#29232,#29233,#29234,#29235,#29236,#29237,#29238,#29239,#29240,
#29241,#29242,#29243,#29244,#29245,#29246,#29247,#29248,#29249,#29250,#29251,
#29252,#29253,#29254,#29255,#29256,#29257,#29258,#29259,#29260,#29261,#29262,
#29263,#29264,#29265,#29266,#29267,#29268,#29269,#29270,#29271,#29272,#29273,
#29274,#29275,#29276,#29277,#29278,#29279,#29280,#29281,#29282,#29283,#29284,
#29285,#29286,#29287,#29288,#29289,#29290,#29291,#29292,#29293,#29294,#29295,
#29296,#29297,#29298,#29299,#29300,#29301,#29302,#29303,#29304,#29305,#29306,
#29307,#29308,#29309,#29310,#29311,#29312,#29313,#29314,#29315,#29316,#29317,
#29318,#29319,#29320,#29321,#29322,#29323,#29324,#29325,#29326,#29327,#29328,
#29329,#29330,#29331,#29332,#29333,#29334,#29335,#29336,#29337,#29338,#29339,
#29340,#29341,#29342,#29343,#29344,#29345,#29346,#29347,#29348,#29349,#29350,
#29351,#29352,#29353,#29354,#29355,#29356,#29357,#29358,#29359,#29360,#29361,
#29362,#29363,#29364,#29365,#29366,#29367,#29368,#29369,#29370,#29371,#29372,
#29373,#29374,#29375,#29376,#29377,#29378,#29379,#29380,#29381,#29382,#29383,
#29384,#29385,#29386,#29387,#29388,#29389,#29390,#29391,#29392,#29393,#29394,
#29395,#29396,#29397,#29398,#29399,#29400,#29401,#29402,#29403,#29404,#29405,
#29406,#29407,#29408,#29409,#29410,#29411,#29412,#29413,#29414,#29415,#29416,
#29417,#29418,#29419,#29420,#29421,#29422,#29423,#29424,#29425,#29426,#29427,
#29428,#29429,#29430,#29431,#29432,#29433,#29434,#29435,#29436,#29437,#29438,
#29439,#29440,#29441,#29442,#29443,#29444,#29445,#29446,#29447,#29448,#29449,
#29450,#29451,#29452,#29453,#29454,#29455,#29456,#29457,#29458,#29459,#29460,
#29461,#29462,#29463,#29464,#29465,#29466,#29467,#29468,#29469,#29470,#29471,
#29472,#29473,#29474,#29475,#29476,#29477,#29478,#29479,#29480,#29481,#29482,
#29483,#29484,#29485,#29486,#29487,#29488,#29489,#29490,#29491,#29492,#29493,
#29494,#29495,#29496,#29497,#29498,#29499,#29500,#29501,#29502,#29503,#29504,
#29505,#29506,#29507,#29508,#29509,#29510,#29511,#29512,#29513,#29514,#29515,
#29516,#29517,#29518,#29519,#29520,#29521,#29522,#29523,#29524,#29525,#29526,
#29527,#29528,#29529,#29530,#29531,#29532,#29533,#29534,#29535,#29536,#29537,
#29538,#29539,#29540,#29541,#29542,#29543,#29544,#29545,#29546,#29547,#29548,
#29549,#29550,#29551,#29552,#29553,#29554,#29555,#29556,#29557,#29558,#29559,
#29560,#29561,#29562,#29563,#29564,#29565,#29566,#29567,#29568,#29569,#29570,
#29571,#29572,#29573,#29574,#29575,#29576,#29577,#29578,#29579,#29580,#29581,
#29582,#29583,#29584,#29585,#29586,#29587,#29588,#29589,#29590,#29591,#29592,
#29593,#29594,#29595,#29596,#29597,#29598,#29599,#29600,#29601,#29602,#29603,
#29604,#29605,#29606,#29607,#29608,#29609,#29610,#29611,#29612,#29613,#29614,
#29615,#29616,#29617,#29618,#29619,#29620,#29621,#29622,#29623,#29624,#29625,
#29626,#29627,#29628,#29629,#29630,#29631,#29632,#29633,#29634,#29635,#29636,
#29637,#29638,#29639,#29640,#29641,#29642,#29643,#29644,#29645,#29646,#29647,
#29648,#29649,#29650,#29651,#29652,#29653,#29654,#29655,#29656,#29657,#29658,
#29659,#29660,#29661,#29662,#29663,#29664,#29665,#29666,#29667,#29668,#29669,
#29670,#29671,#29672,#29673,#29674,#29675,#29676,#29677,#29678,#29679,#29680,
#29681,#29682,#29683,#29684,#29685,#29686,#29687,#29688,#29689,#29690,#29691,
#29692,#29693,#29694,#29695,#29696,#29697,#29698,#29699,#29700,#29701,#29702,
#29703,#29704,#29705,#29706,#29707,#29708,#29709,#29710,#29711,#29712,#29713,
#29714,#29715,#29716,#29717,#29718,#29719,#29720,#29721,#29722,#29723,#29724,
#29725,#29726,#29727,#29728,#29729,#29730,#29731,#29732,#29733,#29734,#29735,
#29736,#29737,#29738,#29739,#29740,#29741,#29742,#29743,#29744),(#29745,
#29746,#29747,#29748,#29749,#29750,#29751,#29752,#29753,#29754,#29755,#29756,
#29757,#29758,#29759,#29760,#29761,#29762,#29763,#29764,#29765,#29766,#29767,
#29768,#29769,#29770,#29771,#29772,#29773,#29774,#29775,#29776,#29777,#29778,
#29779,#29780,#29781,#29782,#29783,#29784,#29785,#29786,#29787,#29788,#29789,
#29790,#29791,#29792,#29793,#29794,#29795,#29796,#29797,#29798,#29799,#29800,
#29801,#29802,#29803,#29804,#29805,#29806,#29807,#29808,#29809,#29810,#29811,
#29812,#29813,#29814,#29815,#29816,#29817,#29818,#29819,#29820,#29821,#29822,
#29823,#29824,#29825,#29826,#29827,#29828,#29829,#29830,#29831,#29832,#29833,
#29834,#29835,#29836,#29837,#29838,#29839,#29840,#29841,#29842,#29843,#29844,
#29845,#29846,#29847,#29848,#29849,#29850,#29851,#29852,#29853,#29854,#29855,
#29856,#29857,#29858,#29859,#29860,#29861,#29862,#29863,#29864,#29865,#29866,
#29867,#29868,#29869,#29870,#29871,#29872,#29873,#29874,#29875,#29876,#29877,
#29878,#29879,#29880,#29881,#29882,#29883,#29884,#29885,#29886,#29887,#29888,
#29889,#29890,#29891,#29892,#29893,#29894,#29895,#29896,#29897,#29898,#29899,
#29900,#29901,#29902,#29903,#29904,#29905,#29906,#29907,#29908,#29909,#29910,
#29911,#29912,#29913,#29914,#29915,#29916,#29917,#29918,#29919,#29920,#29921,
#29922,#29923,#29924,#29925,#29926,#29927,#29928,#29929,#29930,#29931,#29932,
#29933,#29934,#29935,#29936,#29937,#29938,#29939,#29940,#29941,#29942,#29943,
#29944,#29945,#29946,#29947,#29948,#29949,#29950,#29951,#29952,#29953,#29954,
#29955,#29956,#29957,#29958,#29959,#29960,#29961,#29962,#29963,#29964,#29965,
#29966,#29967,#29968,#29969,#29970,#29971,#29972,#29973,#29974,#29975,#29976,
#29977,#29978,#29979,#29980,#29981,#29982,#29983,#29984,#29985,#29986,#29987,
#29988,#29989,#29990,#29991,#29992,#29993,#29994,#29995,#29996,#29997,#29998,
#29999,#30000,#30001,#30002,#30003,#30004,#30005,#30006,#30007,#30008,#30009,
#30010,#30011,#30012,#30013,#30014,#30015,#30016,#30017,#30018,#30019,#30020,
#30021,#30022,#30023,#30024,#30025,#30026,#30027,#30028,#30029,#30030,#30031,
#30032,#30033,#30034,#30035,#30036,#30037,#30038,#30039,#30040,#30041,#30042,
#30043,#30044,#30045,#30046,#30047,#30048,#30049,#30050,#30051,#30052,#30053,
#30054,#30055,#30056,#30057,#30058,#30059,#30060,#30061,#30062,#30063,#30064,
#30065,#30066,#30067,#30068,#30069,#30070,#30071,#30072,#30073,#30074,#30075,
#30076,#30077,#30078,#30079,#30080,#30081,#30082,#30083,#30084,#30085,#30086,
#30087,#30088,#30089,#30090,#30091,#30092,#30093,#30094,#30095,#30096,#30097,
#30098,#30099,#30100,#30101,#30102,#30103,#30104,#30105,#30106,#30107,#30108,
#30109,#30110,#30111,#30112,#30113,#30114,#30115,#30116,#30117,#30118,#30119,
#30120,#30121,#30122,#30123,#30124,#30125,#30126,#30127,#30128,#30129,#30130,
#30131,#30132,#30133,#30134,#30135,#30136,#30137,#30138,#30139,#30140,#30141,
#30142,#30143,#30144,#30145,#30146,#30147,#30148,#30149,#30150,#30151,#30152,
#30153,#30154,#30155,#30156,#30157,#30158,#30159,#30160,#30161,#30162,#30163,
#30164,#30165,#30166,#30167,#30168,#30169,#30170,#30171,#30172,#30173,#30174,
#30175,#30176,#30177,#30178,#30179,#30180,#30181,#30182,#30183,#30184,#30185,
#30186,#30187,#30188,#30189,#30190,#30191,#30192,#30193,#30194,#30195,#30196,
#30197,#30198,#30199,#30200,#30201,#30202,#30203,#30204,#30205,#30206,#30207,
#30208,#30209,#30210,#30211,#30212,#30213,#30214,#30215,#30216,#30217,#30218,
#30219,#30220,#30221,#30222,#30223,#30224,#30225,#30226,#30227,#30228,#30229,
#30230,#30231,#30232,#30233,#30234,#30235,#30236,#30237,#30238,#30239,#30240,
#30241,#30242,#30243,#30244,#30245,#30246,#30247,#30248,#30249,#30250,#30251,
#30252,#30253,#30254,#30255,#30256,#30257,#30258,#30259,#30260,#30261,#30262,
#30263,#30264,#30265,#30266,#30267,#30268,#30269,#30270,#30271,#30272,#30273,
#30274,#30275,#30276,#30277,#30278,#30279,#30280,#30281,#30282,#30283,#30284,
#30285,#30286,#30287,#30288,#30289,#30290,#30291,#30292,#30293,#30294,#30295,
#30296,#30297,#30298,#30299,#30300,#30301,#30302,#30303,#30304,#30305,#30306,
#30307,#30308,#30309,#30310,#30311,#30312,#30313,#30314,#30315,#30316,#30317,
#30318,#30319,#30320,#30321,#30322,#30323,#30324,#30325,#30326,#30327,#30328,
#30329,#30330,#30331,#30332,#30333,#30334,#30335,#30336,#30337,#30338,#30339,
#30340,#30341,#30342,#30343,#30344,#30345,#30346,#30347,#30348,#30349,#30350,
#30351,#30352,#30353,#30354,#30355,#30356,#30357,#30358,#30359,#30360,#30361,
#30362,#30363,#30364,#30365,#30366,#30367,#30368,#30369,#30370,#30371,#30372,
#30373,#30374,#30375,#30376,#30377,#30378,#30379,#30380,#30381,#30382,#30383,
#30384,#30385,#30386,#30387,#30388,#30389,#30390,#30391,#30392,#30393,#30394,
#30395,#30396,#30397,#30398,#30399,#30400,#30401,#30402,#30403,#30404,#30405,
#30406,#30407,#30408,#30409,#30410,#30411,#30412,#30413,#30414,#30415,#30416,
#30417,#30418,#30419,#30420,#30421,#30422,#30423,#30424,#30425,#30426,#30427,
#30428,#30429,#30430,#30431,#30432,#30433,#30434,#30435,#30436,#30437,#30438,
#30439,#30440,#30441,#30442,#30443,#30444,#30445,#30446,#30447,#30448,#30449,
#30450,#30451,#30452,#30453,#30454,#30455,#30456,#30457,#30458,#30459,#30460,
#30461,#30462,#30463,#30464,#30465,#30466,#30467,#30468,#30469,#30470,#30471,
#30472,#30473,#30474,#30475,#30476,#30477,#30478,#30479,#30480,#30481,#30482,
#30483,#30484,#30485,#30486,#30487,#30488,#30489,#30490,#30491,#30492,#30493,
#30494,#30495,#30496,#30497,#30498,#30499,#30500,#30501,#30502,#30503,#30504,
#30505,#30506,#30507,#30508,#30509,#30510,#30511,#30512,#30513,#30514,#30515,
#30516,#30517,#30518,#30519,#30520,#30521,#30522,#30523,#30524,#30525,#30526,
#30527,#30528,#30529,#30530,#30531,#30532,#30533,#30534,#30535,#30536,#30537,
#30538,#30539,#30540,#30541,#30542,#30543,#30544,#30545,#30546,#30547,#30548,
#30549,#30550,#30551,#30552,#30553,#30554,#30555,#30556,#30557,#30558,#30559,
#30560,#30561,#30562,#30563,#30564,#30565,#30566,#30567,#30568,#30569,#30570,
#30571,#30572,#30573,#30574,#30575,#30576,#30577,#30578,#30579,#30580,#30581,
#30582,#30583,#30584,#30585,#30586,#30587,#30588,#30589,#30590,#30591,#30592,
#30593,#30594,#30595,#30596,#30597,#30598,#30599,#30600,#30601,#30602,#30603,
#30604,#30605,#30606,#30607,#30608,#30609,#30610,#30611,#30612,#30613,#30614,
#30615,#30616,#30617,#30618,#30619,#30620,#30621,#30622,#30623,#30624,#30625,
#30626,#30627,#30628,#30629,#30630,#30631,#30632,#30633,#30634,#30635,#30636,
#30637,#30638,#30639,#30640,#30641,#30642,#30643,#30644,#30645,#30646,#30647,
#30648,#30649,#30650,#30651,#30652,#30653,#30654,#30655,#30656,#30657,#30658,
#30659,#30660,#30661,#30662,#30663,#30664,#30665,#30666,#30667,#30668,#30669,
#30670,#30671,#30672,#30673,#30674,#30675,#30676,#30677,#30678,#30679,#30680,
#30681,#30682,#30683,#30684,#30685,#30686,#30687,#30688,#30689,#30690,#30691,
#30692,#30693,#30694,#30695,#30696,#30697,#30698,#30699,#30700,#30701,#30702,
#30703,#30704,#30705,#30706,#30707,#30708,#30709,#30710,#30711,#30712,#30713,
#30714,#30715,#30716,#30717)),.UNSPECIFIED.,.F.,.F.,.F.)
B_SPLINE_SURFACE_WITH_KNOTS((2,2),(3,2,2,2,2,2,2,2,2,2,2,2,2,2,2,2,2,2,
2,2,2,2,2,2,2,2,2,2,2,2,2,2,2,2,2,2,2,2,2,2,2,2,2,2,2,2,2,2,2,2,2,2,2,2,
2,2,2,2,2,2,2,2,2,2,2,2,2,2,2,2,2,2,2,2,2,2,2,2,2,2,2,2,2,2,2,2,2,2,2,2,
2,2,2,2,2,2,2,2,2,2,2,2,2,2,2,2,2,2,2,2,2,2,2,2,2,2,2,2,2,2,2,2,2,2,2,2,
2,2,2,2,2,2,2,2,2,2,2,2,2,2,2,2,2,2,2,2,2,2,2,2,2,2,2,2,2,2,2,2,2,2,2,2,
2,2,2,2,2,2,2,2,2,2,2,2,2,2,2,2,2,2,2,2,2,2,2,2,2,2,2,2,2,2,2,2,2,2,2,2,
2,2,2,2,2,2,2,2,2,2,2,2,2,2,2,2,2,2,2,2,2,2,2,2,2,2,2,2,2,2,2,2,2,2,2,2,
2,2,2,2,2,2,2,2,2,2,2,2,2,2,2,2,2,2,2,2,2,2,2,2,2,2,2,2,2,2,2,2,2,2,2,2,
2,2,2,2,2,2,2,2,2,2,2,2,2,2,2,2,2,2,2,2,2,2,2,2,2,2,2,2,2,2,2,2,2,2,2,2,
2,2,2,2,2,2,2,2,2,2,2,2,2,2,2,2,2,2,2,2,2,2,2,2,2,2,2,2,2,2,2,2,2,2,2,2,
2,2,2,2,2,2,2,2,2,2,2,2,2,2,2,2,2,2,2,2,2,2,2,2,2,2,2,2,2,2,2,2,2,2,2,2,
2,2,2,2,2,2,2,2,2,2,2,2,2,2,2,2,2,2,2,2,2,2,2,2,2,2,2,2,2,2,2,2,2,2,2,2,
2,2,2,2,2,2,2,2,2,2,2,2,2,2,2,2,2,2,2,2,2,2,2,2,2,2,2,2,2,2,2,2,2,2,2,2,
2,2,2,2,2,2,2,2,2,2,2,2,2,2,2,2,2,2,2,2,2,2,2,2,2,2,2,2,2,2,2,2,2,2,2,2,
3),(0.,1.),(0.,0.00205761316872428,0.00411522633744856,0.00617283950617284,
0.00823045267489712,0.0102880658436214,0.0123456790123457,0.01440329218107,
0.0164609053497942,0.0185185185185185,0.0205761316872428,0.0226337448559671,
0.0246913580246914,0.0267489711934156,0.0288065843621399,0.0308641975308642,
0.0329218106995885,0.0349794238683128,0.037037037037037,0.0390946502057613,
0.0411522633744856,0.0432098765432099,0.0452674897119342,0.0473251028806584,
0.0493827160493827,0.051440329218107,0.0534979423868313,0.0555555555555556,
0.0576131687242798,0.0596707818930041,0.0617283950617284,0.0637860082304527,
0.065843621399177,0.0679012345679012,0.0699588477366255,0.0720164609053498,
0.0740740740740741,0.0761316872427984,0.0781893004115226,0.0802469135802469,
0.0823045267489712,0.0843621399176955,0.0864197530864197,0.088477366255144,
0.0905349794238683,0.0925925925925926,0.0946502057613169,0.0967078189300412,
0.0987654320987654,0.10082304526749,0.102880658436214,0.104938271604938,
0.106995884773663,0.109053497942387,0.111111111111111,0.113168724279835,
0.11522633744856,0.117283950617284,0.119341563786008,0.121399176954733,
0.123456790123457,0.125514403292181,0.127572016460905,0.12962962962963,
0.131687242798354,0.133744855967078,0.135802469135802,0.137860082304527,
0.139917695473251,0.141975308641975,0.1440329218107,0.146090534979424,0.148148148148148,
0.150205761316872,0.152263374485597,0.154320987654321,0.156378600823045,
0.15843621399177,0.160493827160494,0.162551440329218,0.164609053497942,
0.166666666666667,0.168724279835391,0.170781893004115,0.172839506172839,
0.174897119341564,0.176954732510288,0.179012345679012,0.181069958847737,
0.183127572016461,0.185185185185185,0.187242798353909,0.189300411522634,
0.191358024691358,0.193415637860082,0.195473251028807,0.197530864197531,
0.199588477366255,0.201646090534979,0.203703703703704,0.205761316872428,
0.207818930041152,0.209876543209877,0.211934156378601,0.213991769547325,
0.216049382716049,0.218106995884774,0.220164609053498,0.222222222222222,
0.224279835390947,0.226337448559671,0.228395061728395,0.230452674897119,
0.232510288065844,0.234567901234568,0.236625514403292,0.238683127572016,
0.240740740740741,0.242798353909465,0.244855967078189,0.246913580246914,
0.248971193415638,0.251028806584362,0.253086419753086,0.255144032921811,
0.257201646090535,0.259259259259259,0.261316872427984,0.263374485596708,
0.265432098765432,0.267489711934156,0.269547325102881,0.271604938271605,
0.273662551440329,0.275720164609054,0.277777777777778,0.279835390946502,
0.281893004115226,0.283950617283951,0.286008230452675,0.288065843621399,
0.290123456790123,0.292181069958848,0.294238683127572,0.296296296296296,
0.298353909465021,0.300411522633745,0.302469135802469,0.304526748971193,
0.306584362139918,0.308641975308642,0.310699588477366,0.312757201646091,
0.314814814814815,0.316872427983539,0.318930041152263,0.320987654320988,
0.323045267489712,0.325102880658436,0.327160493827161,0.329218106995885,
0.331275720164609,0.333333333333333,0.335390946502058,0.337448559670782,
0.339506172839506,0.34156378600823,0.343621399176955,0.345679012345679,
0.347736625514403,0.349794238683128,0.351851851851852,0.353909465020576,
0.3559670781893,0.358024691358025,0.360082304526749,0.362139917695473,0.364197530864198,
0.366255144032922,0.368312757201646,0.37037037037037,0.372427983539095,
0.374485596707819,0.376543209876543,0.378600823045267,0.380658436213992,
0.382716049382716,0.38477366255144,0.386831275720165,0.388888888888889,
0.390946502057613,0.393004115226337,0.395061728395062,0.397119341563786,
0.39917695473251,0.401234567901235,0.403292181069959,0.405349794238683,
0.407407407407407,0.409465020576132,0.411522633744856,0.41358024691358,
0.415637860082305,0.417695473251029,0.419753086419753,0.421810699588477,
0.423868312757202,0.425925925925926,0.42798353909465,0.430041152263374,
0.432098765432099,0.434156378600823,0.436213991769547,0.438271604938272,
0.440329218106996,0.44238683127572,0.444444444444444,0.446502057613169,
0.448559670781893,0.450617283950617,0.452674897119342,0.454732510288066,
0.45679012345679,0.458847736625514,0.460905349794239,0.462962962962963,
0.465020576131687,0.467078189300412,0.469135802469136,0.47119341563786,
0.473251028806584,0.475308641975309,0.477366255144033,0.479423868312757,
0.481481481481481,0.483539094650206,0.48559670781893,0.487654320987654,
0.489711934156379,0.491769547325103,0.493827160493827,0.495884773662551,
0.497942386831276,0.5,0.502057613168724,0.504115226337449,0.506172839506173,
0.508230452674897,0.510288065843621,0.512345679012346,0.51440329218107,
0.516460905349794,0.518518518518518,0.520576131687243,0.522633744855967,
0.524691358024691,0.526748971193416,0.52880658436214,0.530864197530864,
0.532921810699588,0.534979423868313,0.537037037037037,0.539094650205761,
0.541152263374486,0.54320987654321,0.545267489711934,0.547325102880658,
0.549382716049383,0.551440329218107,0.553497942386831,0.555555555555556,
0.55761316872428,0.559670781893004,0.561728395061728,0.563786008230453,
0.565843621399177,0.567901234567901,0.569958847736626,0.57201646090535,
0.574074074074074,0.576131687242798,0.578189300411523,0.580246913580247,
0.582304526748971,0.584362139917695,0.58641975308642,0.588477366255144,
0.590534979423868,0.592592592592593,0.594650205761317,0.596707818930041,
0.598765432098765,0.60082304526749,0.602880658436214,0.604938271604938,
0.606995884773663,0.609053497942387,0.611111111111111,0.613168724279835,
0.61522633744856,0.617283950617284,0.619341563786008,0.621399176954732,
0.623456790123457,0.625514403292181,0.627572016460905,0.62962962962963,
0.631687242798354,0.633744855967078,0.635802469135803,0.637860082304527,
0.639917695473251,0.641975308641975,0.6440329218107,0.646090534979424,0.648148148148148,
0.650205761316872,0.652263374485597,0.654320987654321,0.656378600823045,
0.65843621399177,0.660493827160494,0.662551440329218,0.664609053497942,
0.666666666666667,0.668724279835391,0.670781893004115,0.672839506172839,
0.674897119341564,0.676954732510288,0.679012345679012,0.681069958847737,
0.683127572016461,0.685185185185185,0.687242798353909,0.689300411522634,
0.691358024691358,0.693415637860082,0.695473251028807,0.697530864197531,
0.699588477366255,0.701646090534979,0.703703703703704,0.705761316872428,
0.707818930041152,0.709876543209877,0.711934156378601,0.713991769547325,
0.716049382716049,0.718106995884774,0.720164609053498,0.722222222222222,
0.724279835390947,0.726337448559671,0.728395061728395,0.730452674897119,
0.732510288065844,0.734567901234568,0.736625514403292,0.738683127572016,
0.740740740740741,0.742798353909465,0.744855967078189,0.746913580246914,
0.748971193415638,0.751028806584362,0.753086419753086,0.755144032921811,
0.757201646090535,0.759259259259259,0.761316872427984,0.763374485596708,
0.765432098765432,0.767489711934156,0.769547325102881,0.771604938271605,
0.773662551440329,0.775720164609053,0.777777777777778,0.779835390946502,
0.781893004115226,0.783950617283951,0.786008230452675,0.788065843621399,
0.790123456790123,0.792181069958848,0.794238683127572,0.796296296296296,
0.798353909465021,0.800411522633745,0.802469135802469,0.804526748971193,
0.806584362139918,0.808641975308642,0.810699588477366,0.812757201646091,
0.814814814814815,0.816872427983539,0.818930041152263,0.820987654320988,
0.823045267489712,0.825102880658436,0.827160493827161,0.829218106995885,
0.831275720164609,0.833333333333333,0.835390946502058,0.837448559670782,
0.839506172839506,0.84156378600823,0.843621399176955,0.845679012345679,
0.847736625514403,0.849794238683128,0.851851851851852,0.853909465020576,
0.8559670781893,0.858024691358025,0.860082304526749,0.862139917695473,0.864197530864197,
0.866255144032922,0.868312757201646,0.87037037037037,0.872427983539095,
0.874485596707819,0.876543209876543,0.878600823045268,0.880658436213992,
0.882716049382716,0.88477366255144,0.886831275720165,0.888888888888889,
0.890946502057613,0.893004115226337,0.895061728395062,0.897119341563786,
0.89917695473251,0.901234567901235,0.903292181069959,0.905349794238683,
0.907407407407407,0.909465020576132,0.911522633744856,0.91358024691358,
0.915637860082305,0.917695473251029,0.919753086419753,0.921810699588477,
0.923868312757202,0.925925925925926,0.92798353909465,0.930041152263374,
0.932098765432099,0.934156378600823,0.936213991769547,0.938271604938272,
0.940329218106996,0.94238683127572,0.944444444444444,0.946502057613169,
0.948559670781893,0.950617283950617,0.952674897119342,0.954732510288066,
0.95679012345679,0.958847736625514,0.960905349794239,0.962962962962963,
0.965020576131687,0.967078189300412,0.969135802469136,0.97119341563786,
0.973251028806584,0.975308641975309,0.977366255144033,0.979423868312757,
0.981481481481482,0.983539094650206,0.98559670781893,0.987654320987654,
0.989711934156379,0.991769547325103,0.993827160493827,0.995884773662551,
0.997942386831276,1.),.UNSPECIFIED.)
GEOMETRIC_REPRESENTATION_ITEM()
RATIONAL_B_SPLINE_SURFACE(((1.,0.866025403784439,1.,0.866025403784439,1.,
0.866025403784439,1.,0.866025403784439,1.,0.866025403784439,1.,0.866025403784439,
1.,0.866025403784439,1.,0.866025403784439,1.,0.866025403784439,1.,0.866025403784439,
1.,0.866025403784439,1.,0.866025403784439,1.,0.866025403784439,1.,0.866025403784439,
1.,0.866025403784439,1.,0.866025403784439,1.,0.866025403784439,1.,0.866025403784439,
1.,0.866025403784439,1.,0.866025403784439,1.,0.866025403784439,1.,0.866025403784439,
1.,0.866025403784439,1.,0.866025403784439,1.,0.866025403784439,1.,0.866025403784439,
1.,0.866025403784439,1.,0.866025403784439,1.,0.866025403784439,1.,0.866025403784439,
1.,0.866025403784439,1.,0.866025403784439,1.,0.866025403784439,1.,0.866025403784439,
1.,0.866025403784439,1.,0.866025403784439,1.,0.866025403784439,1.,0.866025403784439,
1.,0.866025403784439,1.,0.866025403784439,1.,0.866025403784439,1.,0.866025403784439,
1.,0.866025403784439,1.,0.866025403784439,1.,0.866025403784439,1.,0.866025403784439,
1.,0.866025403784439,1.,0.866025403784439,1.,0.866025403784439,1.,0.866025403784439,
1.,0.866025403784439,1.,0.866025403784439,1.,0.866025403784439,1.,0.866025403784439,
1.,0.866025403784439,1.,0.866025403784439,1.,0.866025403784439,1.,0.866025403784439,
1.,0.866025403784439,1.,0.866025403784439,1.,0.866025403784439,1.,0.866025403784439,
1.,0.866025403784439,1.,0.866025403784439,1.,0.866025403784439,1.,0.866025403784439,
1.,0.866025403784439,1.,0.866025403784439,1.,0.866025403784439,1.,0.866025403784439,
1.,0.866025403784439,1.,0.866025403784439,1.,0.866025403784439,1.,0.866025403784439,
1.,0.866025403784439,1.,0.866025403784439,1.,0.866025403784439,1.,0.866025403784439,
1.,0.866025403784439,1.,0.866025403784439,1.,0.866025403784439,1.,0.866025403784439,
1.,0.866025403784439,1.,0.866025403784439,1.,0.866025403784439,1.,0.866025403784439,
1.,0.866025403784439,1.,0.866025403784439,1.,0.866025403784439,1.,0.866025403784439,
1.,0.866025403784439,1.,0.866025403784439,1.,0.866025403784439,1.,0.866025403784439,
1.,0.866025403784439,1.,0.866025403784439,1.,0.866025403784439,1.,0.866025403784439,
1.,0.866025403784439,1.,0.866025403784439,1.,0.866025403784439,1.,0.866025403784439,
1.,0.866025403784439,1.,0.866025403784439,1.,0.866025403784439,1.,0.866025403784439,
1.,0.866025403784439,1.,0.866025403784439,1.,0.866025403784439,1.,0.866025403784439,
1.,0.866025403784439,1.,0.866025403784439,1.,0.866025403784439,1.,0.866025403784439,
1.,0.866025403784439,1.,0.866025403784439,1.,0.866025403784439,1.,0.866025403784439,
1.,0.866025403784439,1.,0.866025403784439,1.,0.866025403784439,1.,0.866025403784439,
1.,0.866025403784439,1.,0.866025403784439,1.,0.866025403784439,1.,0.866025403784439,
1.,0.866025403784439,1.,0.866025403784439,1.,0.866025403784439,1.,0.866025403784439,
1.,0.866025403784439,1.,0.866025403784439,1.,0.866025403784439,1.,0.866025403784439,
1.,0.866025403784439,1.,0.866025403784439,1.,0.866025403784439,1.,0.866025403784439,
1.,0.866025403784439,1.,0.866025403784439,1.,0.866025403784439,1.,0.866025403784439,
1.,0.866025403784439,1.,0.866025403784439,1.,0.866025403784439,1.,0.866025403784439,
1.,0.866025403784439,1.,0.866025403784439,1.,0.866025403784439,1.,0.866025403784439,
1.,0.866025403784439,1.,0.866025403784439,1.,0.866025403784439,1.,0.866025403784439,
1.,0.866025403784439,1.,0.866025403784439,1.,0.866025403784439,1.,0.866025403784439,
1.,0.866025403784439,1.,0.866025403784439,1.,0.866025403784439,1.,0.866025403784439,
1.,0.866025403784439,1.,0.866025403784439,1.,0.866025403784439,1.,0.866025403784439,
1.,0.866025403784439,1.,0.866025403784439,1.,0.866025403784439,1.,0.866025403784439,
1.,0.866025403784439,1.,0.866025403784439,1.,0.866025403784439,1.,0.866025403784439,
1.,0.866025403784439,1.,0.866025403784439,1.,0.866025403784439,1.,0.866025403784439,
1.,0.866025403784439,1.,0.866025403784439,1.,0.866025403784439,1.,0.866025403784439,
1.,0.866025403784439,1.,0.866025403784439,1.,0.866025403784439,1.,0.866025403784439,
1.,0.866025403784439,1.,0.866025403784439,1.,0.866025403784439,1.,0.866025403784439,
1.,0.866025403784439,1.,0.866025403784439,1.,0.866025403784439,1.,0.866025403784439,
1.,0.866025403784439,1.,0.866025403784439,1.,0.866025403784439,1.,0.866025403784439,
1.,0.866025403784439,1.,0.866025403784439,1.,0.866025403784439,1.,0.866025403784439,
1.,0.866025403784439,1.,0.866025403784439,1.,0.866025403784439,1.,0.866025403784439,
1.,0.866025403784439,1.,0.866025403784439,1.,0.866025403784439,1.,0.866025403784439,
1.,0.866025403784439,1.,0.866025403784439,1.,0.866025403784439,1.,0.866025403784439,
1.,0.866025403784439,1.,0.866025403784439,1.,0.866025403784439,1.,0.866025403784439,
1.,0.866025403784439,1.,0.866025403784439,1.,0.866025403784439,1.,0.866025403784439,
1.,0.866025403784439,1.,0.866025403784439,1.,0.866025403784439,1.,0.866025403784439,
1.,0.866025403784439,1.,0.866025403784439,1.,0.866025403784439,1.,0.866025403784439,
1.,0.866025403784439,1.,0.866025403784439,1.,0.866025403784439,1.,0.866025403784439,
1.,0.866025403784439,1.,0.866025403784439,1.,0.866025403784439,1.,0.866025403784439,
1.,0.866025403784439,1.,0.866025403784439,1.,0.866025403784439,1.,0.866025403784439,
1.,0.866025403784439,1.,0.866025403784439,1.,0.866025403784439,1.,0.866025403784439,
1.,0.866025403784439,1.,0.866025403784439,1.,0.866025403784439,1.,0.866025403784439,
1.,0.866025403784439,1.,0.866025403784439,1.,0.866025403784439,1.,0.866025403784439,
1.,0.866025403784439,1.,0.866025403784439,1.,0.866025403784439,1.,0.866025403784439,
1.,0.866025403784439,1.,0.866025403784439,1.,0.866025403784439,1.,0.866025403784439,
1.,0.866025403784439,1.,0.866025403784439,1.,0.866025403784439,1.,0.866025403784439,
1.,0.866025403784439,1.,0.866025403784439,1.,0.866025403784439,1.,0.866025403784439,
1.,0.866025403784439,1.,0.866025403784439,1.,0.866025403784439,1.,0.866025403784439,
1.,0.866025403784439,1.,0.866025403784439,1.,0.866025403784439,1.,0.866025403784439,
1.,0.866025403784439,1.,0.866025403784439,1.,0.866025403784439,1.,0.866025403784439,
1.,0.866025403784439,1.,0.866025403784439,1.,0.866025403784439,1.,0.866025403784439,
1.,0.866025403784439,1.,0.866025403784439,1.,0.866025403784439,1.,0.866025403784439,
1.,0.866025403784439,1.,0.866025403784439,1.,0.866025403784439,1.,0.866025403784439,
1.,0.866025403784439,1.,0.866025403784439,1.,0.866025403784439,1.,0.866025403784439,
1.,0.866025403784439,1.,0.866025403784439,1.,0.866025403784439,1.,0.866025403784439,
1.,0.866025403784439,1.,0.866025403784439,1.,0.866025403784439,1.,0.866025403784439,
1.,0.866025403784439,1.,0.866025403784439,1.,0.866025403784439,1.,0.866025403784439,
1.,0.866025403784439,1.,0.866025403784439,1.,0.866025403784439,1.,0.866025403784439,
1.,0.866025403784439,1.,0.866025403784439,1.,0.866025403784439,1.,0.866025403784439,
1.,0.866025403784439,1.,0.866025403784439,1.,0.866025403784439,1.,0.866025403784439,
1.,0.866025403784439,1.,0.866025403784439,1.,0.866025403784439,1.,0.866025403784439,
1.,0.866025403784439,1.,0.866025403784439,1.,0.866025403784439,1.,0.866025403784439,
1.,0.866025403784439,1.,0.866025403784439,1.,0.866025403784439,1.,0.866025403784439,
1.,0.866025403784439,1.,0.866025403784439,1.,0.866025403784439,1.,0.866025403784439,
1.,0.866025403784439,1.,0.866025403784439,1.,0.866025403784439,1.,0.866025403784439,
1.,0.866025403784439,1.,0.866025403784439,1.,0.866025403784439,1.,0.866025403784439,
1.,0.866025403784439,1.,0.866025403784439,1.,0.866025403784439,1.,0.866025403784439,
1.,0.866025403784439,1.,0.866025403784439,1.,0.866025403784439,1.,0.866025403784439,
1.,0.866025403784439,1.,0.866025403784439,1.,0.866025403784439,1.,0.866025403784439,
1.,0.866025403784439,1.,0.866025403784439,1.,0.866025403784439,1.,0.866025403784439,
1.,0.866025403784439,1.,0.866025403784439,1.,0.866025403784439,1.,0.866025403784439,
1.,0.866025403784439,1.,0.866025403784439,1.,0.866025403784439,1.,0.866025403784439,
1.,0.866025403784439,1.,0.866025403784439,1.,0.866025403784439,1.,0.866025403784439,
1.,0.866025403784439,1.,0.866025403784439,1.,0.866025403784439,1.,0.866025403784439,
1.,0.866025403784439,1.,0.866025403784439,1.,0.866025403784439,1.,0.866025403784439,
1.,0.866025403784439,1.,0.866025403784439,1.,0.866025403784439,1.,0.866025403784439,
1.,0.866025403784439,1.,0.866025403784439,1.,0.866025403784439,1.,0.866025403784439,
1.,0.866025403784439,1.,0.866025403784439,1.,0.866025403784439,1.,0.866025403784439,
1.,0.866025403784439,1.,0.866025403784439,1.,0.866025403784439,1.,0.866025403784439,
1.,0.866025403784439,1.,0.866025403784439,1.,0.866025403784439,1.,0.866025403784439,
1.,0.866025403784439,1.,0.866025403784439,1.,0.866025403784439,1.,0.866025403784439,
1.,0.866025403784439,1.,0.866025403784439,1.,0.866025403784439,1.,0.866025403784439,
1.,0.866025403784439,1.,0.866025403784439,1.,0.866025403784439,1.,0.866025403784439,
1.,0.866025403784439,1.,0.866025403784439,1.,0.866025403784439,1.,0.866025403784439,
1.,0.866025403784439,1.,0.866025403784439,1.,0.866025403784439,1.,0.866025403784439,
1.,0.866025403784439,1.,0.866025403784439,1.,0.866025403784439,1.,0.866025403784439,
1.,0.866025403784439,1.,0.866025403784439,1.,0.866025403784439,1.,0.866025403784439,
1.,0.866025403784439,1.,0.866025403784439,1.,0.866025403784439,1.,0.866025403784439,
1.,0.866025403784439,1.,0.866025403784439,1.,0.866025403784439,1.,0.866025403784439,
1.,0.866025403784439,1.,0.866025403784439,1.,0.866025403784439,1.,0.866025403784439,
1.,0.866025403784439,1.,0.866025403784439,1.,0.866025403784439,1.,0.866025403784439,
1.,0.866025403784439,1.,0.866025403784439,1.,0.866025403784439,1.,0.866025403784439,
1.,0.866025403784439,1.,0.866025403784439,1.,0.866025403784439,1.,0.866025403784439,
1.,0.866025403784439,1.,0.866025403784439,1.,0.866025403784439,1.,0.866025403784439,
1.,0.866025403784439,1.,0.866025403784439,1.,0.866025403784439,1.,0.866025403784439,
1.,0.866025403784439,1.,0.866025403784439,1.,0.866025403784439,1.,0.866025403784439,
1.,0.866025403784439,1.,0.866025403784439,1.,0.866025403784439,1.,0.866025403784439,
1.,0.866025403784439,1.,0.866025403784439,1.,0.866025403784439,1.,0.866025403784439,
1.,0.866025403784439,1.,0.866025403784439,1.,0.866025403784439,1.,0.866025403784439,
1.,0.866025403784439,1.,0.866025403784439,1.,0.866025403784439,1.,0.866025403784439,
1.,0.866025403784439,1.,0.866025403784439,1.,0.866025403784439,1.,0.866025403784439,
1.),(1.,0.866025403784439,1.,0.866025403784439,1.,0.866025403784439,1.,
0.866025403784439,1.,0.866025403784439,1.,0.866025403784439,1.,0.866025403784439,
1.,0.866025403784439,1.,0.866025403784439,1.,0.866025403784439,1.,0.866025403784439,
1.,0.866025403784439,1.,0.866025403784439,1.,0.866025403784439,1.,0.866025403784439,
1.,0.866025403784439,1.,0.866025403784439,1.,0.866025403784439,1.,0.866025403784439,
1.,0.866025403784439,1.,0.866025403784439,1.,0.866025403784439,1.,0.866025403784439,
1.,0.866025403784439,1.,0.866025403784439,1.,0.866025403784439,1.,0.866025403784439,
1.,0.866025403784439,1.,0.866025403784439,1.,0.866025403784439,1.,0.866025403784439,
1.,0.866025403784439,1.,0.866025403784439,1.,0.866025403784439,1.,0.866025403784439,
1.,0.866025403784439,1.,0.866025403784439,1.,0.866025403784439,1.,0.866025403784439,
1.,0.866025403784439,1.,0.866025403784439,1.,0.866025403784439,1.,0.866025403784439,
1.,0.866025403784439,1.,0.866025403784439,1.,0.866025403784439,1.,0.866025403784439,
1.,0.866025403784439,1.,0.866025403784439,1.,0.866025403784439,1.,0.866025403784439,
1.,0.866025403784439,1.,0.866025403784439,1.,0.866025403784439,1.,0.866025403784439,
1.,0.866025403784439,1.,0.866025403784439,1.,0.866025403784439,1.,0.866025403784439,
1.,0.866025403784439,1.,0.866025403784439,1.,0.866025403784439,1.,0.866025403784439,
1.,0.866025403784439,1.,0.866025403784439,1.,0.866025403784439,1.,0.866025403784439,
1.,0.866025403784439,1.,0.866025403784439,1.,0.866025403784439,1.,0.866025403784439,
1.,0.866025403784439,1.,0.866025403784439,1.,0.866025403784439,1.,0.866025403784439,
1.,0.866025403784439,1.,0.866025403784439,1.,0.866025403784439,1.,0.866025403784439,
1.,0.866025403784439,1.,0.866025403784439,1.,0.866025403784439,1.,0.866025403784439,
1.,0.866025403784439,1.,0.866025403784439,1.,0.866025403784439,1.,0.866025403784439,
1.,0.866025403784439,1.,0.866025403784439,1.,0.866025403784439,1.,0.866025403784439,
1.,0.866025403784439,1.,0.866025403784439,1.,0.866025403784439,1.,0.866025403784439,
1.,0.866025403784439,1.,0.866025403784439,1.,0.866025403784439,1.,0.866025403784439,
1.,0.866025403784439,1.,0.866025403784439,1.,0.866025403784439,1.,0.866025403784439,
1.,0.866025403784439,1.,0.866025403784439,1.,0.866025403784439,1.,0.866025403784439,
1.,0.866025403784439,1.,0.866025403784439,1.,0.866025403784439,1.,0.866025403784439,
1.,0.866025403784439,1.,0.866025403784439,1.,0.866025403784439,1.,0.866025403784439,
1.,0.866025403784439,1.,0.866025403784439,1.,0.866025403784439,1.,0.866025403784439,
1.,0.866025403784439,1.,0.866025403784439,1.,0.866025403784439,1.,0.866025403784439,
1.,0.866025403784439,1.,0.866025403784439,1.,0.866025403784439,1.,0.866025403784439,
1.,0.866025403784439,1.,0.866025403784439,1.,0.866025403784439,1.,0.866025403784439,
1.,0.866025403784439,1.,0.866025403784439,1.,0.866025403784439,1.,0.866025403784439,
1.,0.866025403784439,1.,0.866025403784439,1.,0.866025403784439,1.,0.866025403784439,
1.,0.866025403784439,1.,0.866025403784439,1.,0.866025403784439,1.,0.866025403784439,
1.,0.866025403784439,1.,0.866025403784439,1.,0.866025403784439,1.,0.866025403784439,
1.,0.866025403784439,1.,0.866025403784439,1.,0.866025403784439,1.,0.866025403784439,
1.,0.866025403784439,1.,0.866025403784439,1.,0.866025403784439,1.,0.866025403784439,
1.,0.866025403784439,1.,0.866025403784439,1.,0.866025403784439,1.,0.866025403784439,
1.,0.866025403784439,1.,0.866025403784439,1.,0.866025403784439,1.,0.866025403784439,
1.,0.866025403784439,1.,0.866025403784439,1.,0.866025403784439,1.,0.866025403784439,
1.,0.866025403784439,1.,0.866025403784439,1.,0.866025403784439,1.,0.866025403784439,
1.,0.866025403784439,1.,0.866025403784439,1.,0.866025403784439,1.,0.866025403784439,
1.,0.866025403784439,1.,0.866025403784439,1.,0.866025403784439,1.,0.866025403784439,
1.,0.866025403784439,1.,0.866025403784439,1.,0.866025403784439,1.,0.866025403784439,
1.,0.866025403784439,1.,0.866025403784439,1.,0.866025403784439,1.,0.866025403784439,
1.,0.866025403784439,1.,0.866025403784439,1.,0.866025403784439,1.,0.866025403784439,
1.,0.866025403784439,1.,0.866025403784439,1.,0.866025403784439,1.,0.866025403784439,
1.,0.866025403784439,1.,0.866025403784439,1.,0.866025403784439,1.,0.866025403784439,
1.,0.866025403784439,1.,0.866025403784439,1.,0.866025403784439,1.,0.866025403784439,
1.,0.866025403784439,1.,0.866025403784439,1.,0.866025403784439,1.,0.866025403784439,
1.,0.866025403784439,1.,0.866025403784439,1.,0.866025403784439,1.,0.866025403784439,
1.,0.866025403784439,1.,0.866025403784439,1.,0.866025403784439,1.,0.866025403784439,
1.,0.866025403784439,1.,0.866025403784439,1.,0.866025403784439,1.,0.866025403784439,
1.,0.866025403784439,1.,0.866025403784439,1.,0.866025403784439,1.,0.866025403784439,
1.,0.866025403784439,1.,0.866025403784439,1.,0.866025403784439,1.,0.866025403784439,
1.,0.866025403784439,1.,0.866025403784439,1.,0.866025403784439,1.,0.866025403784439,
1.,0.866025403784439,1.,0.866025403784439,1.,0.866025403784439,1.,0.866025403784439,
1.,0.866025403784439,1.,0.866025403784439,1.,0.866025403784439,1.,0.866025403784439,
1.,0.866025403784439,1.,0.866025403784439,1.,0.866025403784439,1.,0.866025403784439,
1.,0.866025403784439,1.,0.866025403784439,1.,0.866025403784439,1.,0.866025403784439,
1.,0.866025403784439,1.,0.866025403784439,1.,0.866025403784439,1.,0.866025403784439,
1.,0.866025403784439,1.,0.866025403784439,1.,0.866025403784439,1.,0.866025403784439,
1.,0.866025403784439,1.,0.866025403784439,1.,0.866025403784439,1.,0.866025403784439,
1.,0.866025403784439,1.,0.866025403784439,1.,0.866025403784439,1.,0.866025403784439,
1.,0.866025403784439,1.,0.866025403784439,1.,0.866025403784439,1.,0.866025403784439,
1.,0.866025403784439,1.,0.866025403784439,1.,0.866025403784439,1.,0.866025403784439,
1.,0.866025403784439,1.,0.866025403784439,1.,0.866025403784439,1.,0.866025403784439,
1.,0.866025403784439,1.,0.866025403784439,1.,0.866025403784439,1.,0.866025403784439,
1.,0.866025403784439,1.,0.866025403784439,1.,0.866025403784439,1.,0.866025403784439,
1.,0.866025403784439,1.,0.866025403784439,1.,0.866025403784439,1.,0.866025403784439,
1.,0.866025403784439,1.,0.866025403784439,1.,0.866025403784439,1.,0.866025403784439,
1.,0.866025403784439,1.,0.866025403784439,1.,0.866025403784439,1.,0.866025403784439,
1.,0.866025403784439,1.,0.866025403784439,1.,0.866025403784439,1.,0.866025403784439,
1.,0.866025403784439,1.,0.866025403784439,1.,0.866025403784439,1.,0.866025403784439,
1.,0.866025403784439,1.,0.866025403784439,1.,0.866025403784439,1.,0.866025403784439,
1.,0.866025403784439,1.,0.866025403784439,1.,0.866025403784439,1.,0.866025403784439,
1.,0.866025403784439,1.,0.866025403784439,1.,0.866025403784439,1.,0.866025403784439,
1.,0.866025403784439,1.,0.866025403784439,1.,0.866025403784439,1.,0.866025403784439,
1.,0.866025403784439,1.,0.866025403784439,1.,0.866025403784439,1.,0.866025403784439,
1.,0.866025403784439,1.,0.866025403784439,1.,0.866025403784439,1.,0.866025403784439,
1.,0.866025403784439,1.,0.866025403784439,1.,0.866025403784439,1.,0.866025403784439,
1.,0.866025403784439,1.,0.866025403784439,1.,0.866025403784439,1.,0.866025403784439,
1.,0.866025403784439,1.,0.866025403784439,1.,0.866025403784439,1.,0.866025403784439,
1.,0.866025403784439,1.,0.866025403784439,1.,0.866025403784439,1.,0.866025403784439,
1.,0.866025403784439,1.,0.866025403784439,1.,0.866025403784439,1.,0.866025403784439,
1.,0.866025403784439,1.,0.866025403784439,1.,0.866025403784439,1.,0.866025403784439,
1.,0.866025403784439,1.,0.866025403784439,1.,0.866025403784439,1.,0.866025403784439,
1.,0.866025403784439,1.,0.866025403784439,1.,0.866025403784439,1.,0.866025403784439,
1.,0.866025403784439,1.,0.866025403784439,1.,0.866025403784439,1.,0.866025403784439,
1.,0.866025403784439,1.,0.866025403784439,1.,0.866025403784439,1.,0.866025403784439,
1.,0.866025403784439,1.,0.866025403784439,1.,0.866025403784439,1.,0.866025403784439,
1.,0.866025403784439,1.,0.866025403784439,1.,0.866025403784439,1.,0.866025403784439,
1.,0.866025403784439,1.,0.866025403784439,1.,0.866025403784439,1.,0.866025403784439,
1.,0.866025403784439,1.,0.866025403784439,1.,0.866025403784439,1.,0.866025403784439,
1.,0.866025403784439,1.,0.866025403784439,1.,0.866025403784439,1.,0.866025403784439,
1.,0.866025403784439,1.,0.866025403784439,1.,0.866025403784439,1.,0.866025403784439,
1.,0.866025403784439,1.,0.866025403784439,1.,0.866025403784439,1.,0.866025403784439,
1.,0.866025403784439,1.,0.866025403784439,1.,0.866025403784439,1.,0.866025403784439,
1.,0.866025403784439,1.,0.866025403784439,1.,0.866025403784439,1.,0.866025403784439,
1.,0.866025403784439,1.,0.866025403784439,1.,0.866025403784439,1.,0.866025403784439,
1.,0.866025403784439,1.,0.866025403784439,1.,0.866025403784439,1.,0.866025403784439,
1.,0.866025403784439,1.,0.866025403784439,1.,0.866025403784439,1.,0.866025403784439,
1.,0.866025403784439,1.,0.866025403784439,1.,0.866025403784439,1.,0.866025403784439,
1.,0.866025403784439,1.,0.866025403784439,1.,0.866025403784439,1.,0.866025403784439,
1.,0.866025403784439,1.,0.866025403784439,1.,0.866025403784439,1.,0.866025403784439,
1.,0.866025403784439,1.,0.866025403784439,1.,0.866025403784439,1.,0.866025403784439,
1.,0.866025403784439,1.,0.866025403784439,1.,0.866025403784439,1.,0.866025403784439,
1.,0.866025403784439,1.,0.866025403784439,1.,0.866025403784439,1.,0.866025403784439,
1.,0.866025403784439,1.,0.866025403784439,1.,0.866025403784439,1.,0.866025403784439,
1.,0.866025403784439,1.,0.866025403784439,1.,0.866025403784439,1.,0.866025403784439,
1.,0.866025403784439,1.,0.866025403784439,1.,0.866025403784439,1.,0.866025403784439,
1.,0.866025403784439,1.,0.866025403784439,1.,0.866025403784439,1.,0.866025403784439,
1.,0.866025403784439,1.,0.866025403784439,1.,0.866025403784439,1.,0.866025403784439,
1.,0.866025403784439,1.,0.866025403784439,1.,0.866025403784439,1.,0.866025403784439,
1.,0.866025403784439,1.,0.866025403784439,1.,0.866025403784439,1.,0.866025403784439,
1.,0.866025403784439,1.,0.866025403784439,1.,0.866025403784439,1.,0.866025403784439,
1.,0.866025403784439,1.,0.866025403784439,1.,0.866025403784439,1.,0.866025403784439,
1.,0.866025403784439,1.,0.866025403784439,1.,0.866025403784439,1.,0.866025403784439,
1.,0.866025403784439,1.,0.866025403784439,1.,0.866025403784439,1.,0.866025403784439,
1.,0.866025403784439,1.,0.866025403784439,1.,0.866025403784439,1.)))
REPRESENTATION_ITEM('')
SURFACE()
);
#179=(
BOUNDED_SURFACE()
B_SPLINE_SURFACE(3,2,((#32628,#32629,#32630,#32631,#32632,#32633,#32634,
#32635,#32636,#32637,#32638,#32639,#32640,#32641,#32642,#32643,#32644,#32645,
#32646,#32647,#32648,#32649,#32650,#32651,#32652,#32653,#32654,#32655,#32656,
#32657,#32658,#32659,#32660,#32661,#32662,#32663,#32664,#32665,#32666,#32667,
#32668,#32669,#32670,#32671,#32672,#32673,#32674,#32675,#32676,#32677,#32678,
#32679,#32680,#32681,#32682,#32683,#32684,#32685,#32686,#32687,#32688,#32689,
#32690,#32691,#32692,#32693,#32694,#32695,#32696,#32697,#32698,#32699,#32700,
#32701,#32702,#32703,#32704,#32705,#32706,#32707,#32708,#32709,#32710,#32711,
#32712,#32713,#32714,#32715,#32716,#32717,#32718,#32719,#32720,#32721,#32722,
#32723,#32724,#32725,#32726,#32727,#32728,#32729,#32730,#32731,#32732,#32733,
#32734,#32735,#32736,#32737,#32738,#32739,#32740,#32741,#32742,#32743,#32744,
#32745,#32746,#32747,#32748,#32749,#32750,#32751,#32752,#32753,#32754,#32755,
#32756,#32757,#32758,#32759,#32760,#32761,#32762,#32763,#32764,#32765,#32766,
#32767,#32768,#32769,#32770,#32771,#32772,#32773,#32774,#32775,#32776,#32777,
#32778,#32779,#32780,#32781,#32782,#32783,#32784,#32785,#32786,#32787,#32788,
#32789,#32790,#32791,#32792,#32793,#32794,#32795,#32796,#32797,#32798,#32799,
#32800,#32801,#32802,#32803,#32804,#32805,#32806,#32807,#32808,#32809,#32810,
#32811,#32812,#32813,#32814,#32815,#32816,#32817,#32818,#32819,#32820,#32821,
#32822,#32823,#32824,#32825,#32826,#32827,#32828,#32829,#32830,#32831,#32832,
#32833,#32834,#32835,#32836,#32837,#32838,#32839,#32840,#32841,#32842,#32843,
#32844,#32845,#32846,#32847,#32848,#32849,#32850,#32851,#32852,#32853,#32854,
#32855,#32856,#32857,#32858,#32859,#32860,#32861,#32862,#32863,#32864,#32865,
#32866,#32867,#32868,#32869,#32870,#32871,#32872,#32873,#32874,#32875,#32876,
#32877,#32878,#32879,#32880,#32881,#32882,#32883,#32884,#32885,#32886,#32887,
#32888,#32889,#32890,#32891,#32892,#32893,#32894,#32895,#32896,#32897,#32898,
#32899,#32900,#32901,#32902,#32903,#32904,#32905,#32906,#32907,#32908,#32909,
#32910,#32911,#32912,#32913,#32914,#32915,#32916,#32917,#32918,#32919,#32920,
#32921,#32922,#32923,#32924,#32925,#32926,#32927,#32928,#32929,#32930,#32931,
#32932,#32933,#32934,#32935,#32936,#32937,#32938,#32939,#32940,#32941,#32942,
#32943,#32944,#32945,#32946,#32947,#32948,#32949,#32950,#32951,#32952,#32953,
#32954,#32955,#32956,#32957,#32958,#32959,#32960,#32961,#32962,#32963,#32964,
#32965,#32966,#32967,#32968,#32969,#32970,#32971,#32972,#32973,#32974,#32975,
#32976,#32977,#32978,#32979,#32980,#32981,#32982,#32983,#32984,#32985,#32986,
#32987,#32988,#32989,#32990,#32991,#32992,#32993,#32994,#32995,#32996,#32997,
#32998,#32999,#33000,#33001,#33002,#33003,#33004,#33005,#33006,#33007,#33008,
#33009,#33010,#33011,#33012,#33013,#33014,#33015,#33016,#33017,#33018,#33019,
#33020,#33021,#33022,#33023,#33024,#33025,#33026,#33027,#33028,#33029,#33030,
#33031,#33032,#33033,#33034,#33035,#33036,#33037,#33038,#33039,#33040,#33041,
#33042,#33043,#33044,#33045,#33046,#33047,#33048,#33049,#33050,#33051,#33052,
#33053,#33054,#33055,#33056,#33057,#33058,#33059,#33060,#33061,#33062,#33063,
#33064,#33065,#33066,#33067,#33068,#33069,#33070,#33071,#33072,#33073,#33074,
#33075,#33076,#33077,#33078,#33079,#33080,#33081,#33082,#33083,#33084,#33085,
#33086,#33087,#33088,#33089,#33090,#33091,#33092,#33093,#33094,#33095,#33096,
#33097,#33098,#33099,#33100,#33101,#33102,#33103,#33104,#33105,#33106,#33107,
#33108,#33109,#33110,#33111,#33112,#33113,#33114,#33115,#33116,#33117,#33118,
#33119,#33120,#33121,#33122,#33123,#33124,#33125,#33126,#33127,#33128,#33129,
#33130,#33131,#33132,#33133,#33134,#33135,#33136,#33137,#33138,#33139,#33140,
#33141,#33142,#33143,#33144,#33145,#33146,#33147,#33148,#33149,#33150,#33151,
#33152,#33153,#33154,#33155,#33156,#33157,#33158,#33159,#33160,#33161,#33162,
#33163,#33164,#33165,#33166,#33167,#33168,#33169,#33170,#33171,#33172,#33173,
#33174,#33175,#33176,#33177,#33178,#33179,#33180,#33181,#33182,#33183,#33184,
#33185,#33186,#33187,#33188,#33189,#33190,#33191,#33192,#33193,#33194,#33195,
#33196,#33197,#33198,#33199,#33200,#33201,#33202,#33203,#33204,#33205,#33206,
#33207,#33208,#33209,#33210,#33211,#33212,#33213,#33214,#33215,#33216,#33217,
#33218,#33219,#33220,#33221,#33222,#33223,#33224,#33225,#33226,#33227,#33228,
#33229,#33230,#33231,#33232,#33233,#33234,#33235,#33236,#33237,#33238,#33239,
#33240,#33241,#33242,#33243,#33244,#33245,#33246,#33247,#33248,#33249,#33250,
#33251,#33252,#33253,#33254,#33255,#33256,#33257,#33258,#33259,#33260,#33261,
#33262,#33263,#33264,#33265,#33266,#33267,#33268,#33269,#33270,#33271,#33272,
#33273,#33274,#33275,#33276,#33277,#33278,#33279,#33280,#33281,#33282,#33283,
#33284,#33285,#33286,#33287,#33288,#33289,#33290,#33291,#33292,#33293,#33294,
#33295,#33296,#33297,#33298,#33299,#33300,#33301,#33302,#33303,#33304,#33305,
#33306,#33307,#33308,#33309,#33310,#33311,#33312,#33313,#33314,#33315,#33316,
#33317,#33318,#33319,#33320,#33321,#33322,#33323,#33324,#33325,#33326,#33327,
#33328,#33329,#33330,#33331,#33332,#33333,#33334,#33335,#33336,#33337,#33338,
#33339,#33340,#33341,#33342,#33343,#33344,#33345,#33346,#33347,#33348,#33349,
#33350,#33351,#33352,#33353,#33354,#33355,#33356,#33357,#33358,#33359,#33360,
#33361,#33362,#33363,#33364,#33365,#33366,#33367,#33368,#33369,#33370,#33371,
#33372,#33373,#33374,#33375,#33376,#33377,#33378,#33379,#33380,#33381,#33382,
#33383,#33384,#33385,#33386,#33387,#33388,#33389,#33390,#33391,#33392,#33393,
#33394,#33395,#33396,#33397,#33398,#33399,#33400,#33401,#33402,#33403,#33404,
#33405,#33406,#33407,#33408,#33409,#33410,#33411,#33412,#33413,#33414,#33415,
#33416,#33417,#33418,#33419,#33420,#33421,#33422,#33423,#33424,#33425,#33426,
#33427,#33428,#33429,#33430,#33431,#33432,#33433,#33434,#33435,#33436,#33437,
#33438,#33439,#33440,#33441,#33442,#33443,#33444,#33445,#33446,#33447,#33448,
#33449,#33450,#33451,#33452,#33453,#33454,#33455,#33456,#33457,#33458,#33459,
#33460,#33461,#33462,#33463,#33464,#33465,#33466,#33467,#33468,#33469,#33470,
#33471,#33472,#33473,#33474,#33475,#33476,#33477,#33478,#33479,#33480,#33481,
#33482,#33483,#33484,#33485,#33486,#33487,#33488,#33489,#33490,#33491,#33492,
#33493,#33494,#33495,#33496,#33497,#33498,#33499,#33500,#33501,#33502,#33503,
#33504,#33505,#33506,#33507,#33508,#33509,#33510,#33511,#33512,#33513,#33514,
#33515,#33516,#33517,#33518,#33519,#33520,#33521,#33522,#33523,#33524,#33525,
#33526,#33527,#33528,#33529,#33530,#33531,#33532,#33533,#33534,#33535,#33536,
#33537,#33538,#33539,#33540,#33541,#33542,#33543,#33544,#33545,#33546,#33547,
#33548,#33549,#33550,#33551,#33552,#33553,#33554,#33555,#33556,#33557,#33558,
#33559,#33560,#33561,#33562,#33563,#33564,#33565,#33566,#33567,#33568,#33569,
#33570,#33571,#33572,#33573,#33574,#33575,#33576,#33577,#33578,#33579,#33580,
#33581,#33582,#33583,#33584,#33585,#33586,#33587,#33588,#33589,#33590,#33591,
#33592,#33593,#33594,#33595,#33596,#33597,#33598,#33599,#33600),(#33601,
#33602,#33603,#33604,#33605,#33606,#33607,#33608,#33609,#33610,#33611,#33612,
#33613,#33614,#33615,#33616,#33617,#33618,#33619,#33620,#33621,#33622,#33623,
#33624,#33625,#33626,#33627,#33628,#33629,#33630,#33631,#33632,#33633,#33634,
#33635,#33636,#33637,#33638,#33639,#33640,#33641,#33642,#33643,#33644,#33645,
#33646,#33647,#33648,#33649,#33650,#33651,#33652,#33653,#33654,#33655,#33656,
#33657,#33658,#33659,#33660,#33661,#33662,#33663,#33664,#33665,#33666,#33667,
#33668,#33669,#33670,#33671,#33672,#33673,#33674,#33675,#33676,#33677,#33678,
#33679,#33680,#33681,#33682,#33683,#33684,#33685,#33686,#33687,#33688,#33689,
#33690,#33691,#33692,#33693,#33694,#33695,#33696,#33697,#33698,#33699,#33700,
#33701,#33702,#33703,#33704,#33705,#33706,#33707,#33708,#33709,#33710,#33711,
#33712,#33713,#33714,#33715,#33716,#33717,#33718,#33719,#33720,#33721,#33722,
#33723,#33724,#33725,#33726,#33727,#33728,#33729,#33730,#33731,#33732,#33733,
#33734,#33735,#33736,#33737,#33738,#33739,#33740,#33741,#33742,#33743,#33744,
#33745,#33746,#33747,#33748,#33749,#33750,#33751,#33752,#33753,#33754,#33755,
#33756,#33757,#33758,#33759,#33760,#33761,#33762,#33763,#33764,#33765,#33766,
#33767,#33768,#33769,#33770,#33771,#33772,#33773,#33774,#33775,#33776,#33777,
#33778,#33779,#33780,#33781,#33782,#33783,#33784,#33785,#33786,#33787,#33788,
#33789,#33790,#33791,#33792,#33793,#33794,#33795,#33796,#33797,#33798,#33799,
#33800,#33801,#33802,#33803,#33804,#33805,#33806,#33807,#33808,#33809,#33810,
#33811,#33812,#33813,#33814,#33815,#33816,#33817,#33818,#33819,#33820,#33821,
#33822,#33823,#33824,#33825,#33826,#33827,#33828,#33829,#33830,#33831,#33832,
#33833,#33834,#33835,#33836,#33837,#33838,#33839,#33840,#33841,#33842,#33843,
#33844,#33845,#33846,#33847,#33848,#33849,#33850,#33851,#33852,#33853,#33854,
#33855,#33856,#33857,#33858,#33859,#33860,#33861,#33862,#33863,#33864,#33865,
#33866,#33867,#33868,#33869,#33870,#33871,#33872,#33873,#33874,#33875,#33876,
#33877,#33878,#33879,#33880,#33881,#33882,#33883,#33884,#33885,#33886,#33887,
#33888,#33889,#33890,#33891,#33892,#33893,#33894,#33895,#33896,#33897,#33898,
#33899,#33900,#33901,#33902,#33903,#33904,#33905,#33906,#33907,#33908,#33909,
#33910,#33911,#33912,#33913,#33914,#33915,#33916,#33917,#33918,#33919,#33920,
#33921,#33922,#33923,#33924,#33925,#33926,#33927,#33928,#33929,#33930,#33931,
#33932,#33933,#33934,#33935,#33936,#33937,#33938,#33939,#33940,#33941,#33942,
#33943,#33944,#33945,#33946,#33947,#33948,#33949,#33950,#33951,#33952,#33953,
#33954,#33955,#33956,#33957,#33958,#33959,#33960,#33961,#33962,#33963,#33964,
#33965,#33966,#33967,#33968,#33969,#33970,#33971,#33972,#33973,#33974,#33975,
#33976,#33977,#33978,#33979,#33980,#33981,#33982,#33983,#33984,#33985,#33986,
#33987,#33988,#33989,#33990,#33991,#33992,#33993,#33994,#33995,#33996,#33997,
#33998,#33999,#34000,#34001,#34002,#34003,#34004,#34005,#34006,#34007,#34008,
#34009,#34010,#34011,#34012,#34013,#34014,#34015,#34016,#34017,#34018,#34019,
#34020,#34021,#34022,#34023,#34024,#34025,#34026,#34027,#34028,#34029,#34030,
#34031,#34032,#34033,#34034,#34035,#34036,#34037,#34038,#34039,#34040,#34041,
#34042,#34043,#34044,#34045,#34046,#34047,#34048,#34049,#34050,#34051,#34052,
#34053,#34054,#34055,#34056,#34057,#34058,#34059,#34060,#34061,#34062,#34063,
#34064,#34065,#34066,#34067,#34068,#34069,#34070,#34071,#34072,#34073,#34074,
#34075,#34076,#34077,#34078,#34079,#34080,#34081,#34082,#34083,#34084,#34085,
#34086,#34087,#34088,#34089,#34090,#34091,#34092,#34093,#34094,#34095,#34096,
#34097,#34098,#34099,#34100,#34101,#34102,#34103,#34104,#34105,#34106,#34107,
#34108,#34109,#34110,#34111,#34112,#34113,#34114,#34115,#34116,#34117,#34118,
#34119,#34120,#34121,#34122,#34123,#34124,#34125,#34126,#34127,#34128,#34129,
#34130,#34131,#34132,#34133,#34134,#34135,#34136,#34137,#34138,#34139,#34140,
#34141,#34142,#34143,#34144,#34145,#34146,#34147,#34148,#34149,#34150,#34151,
#34152,#34153,#34154,#34155,#34156,#34157,#34158,#34159,#34160,#34161,#34162,
#34163,#34164,#34165,#34166,#34167,#34168,#34169,#34170,#34171,#34172,#34173,
#34174,#34175,#34176,#34177,#34178,#34179,#34180,#34181,#34182,#34183,#34184,
#34185,#34186,#34187,#34188,#34189,#34190,#34191,#34192,#34193,#34194,#34195,
#34196,#34197,#34198,#34199,#34200,#34201,#34202,#34203,#34204,#34205,#34206,
#34207,#34208,#34209,#34210,#34211,#34212,#34213,#34214,#34215,#34216,#34217,
#34218,#34219,#34220,#34221,#34222,#34223,#34224,#34225,#34226,#34227,#34228,
#34229,#34230,#34231,#34232,#34233,#34234,#34235,#34236,#34237,#34238,#34239,
#34240,#34241,#34242,#34243,#34244,#34245,#34246,#34247,#34248,#34249,#34250,
#34251,#34252,#34253,#34254,#34255,#34256,#34257,#34258,#34259,#34260,#34261,
#34262,#34263,#34264,#34265,#34266,#34267,#34268,#34269,#34270,#34271,#34272,
#34273,#34274,#34275,#34276,#34277,#34278,#34279,#34280,#34281,#34282,#34283,
#34284,#34285,#34286,#34287,#34288,#34289,#34290,#34291,#34292,#34293,#34294,
#34295,#34296,#34297,#34298,#34299,#34300,#34301,#34302,#34303,#34304,#34305,
#34306,#34307,#34308,#34309,#34310,#34311,#34312,#34313,#34314,#34315,#34316,
#34317,#34318,#34319,#34320,#34321,#34322,#34323,#34324,#34325,#34326,#34327,
#34328,#34329,#34330,#34331,#34332,#34333,#34334,#34335,#34336,#34337,#34338,
#34339,#34340,#34341,#34342,#34343,#34344,#34345,#34346,#34347,#34348,#34349,
#34350,#34351,#34352,#34353,#34354,#34355,#34356,#34357,#34358,#34359,#34360,
#34361,#34362,#34363,#34364,#34365,#34366,#34367,#34368,#34369,#34370,#34371,
#34372,#34373,#34374,#34375,#34376,#34377,#34378,#34379,#34380,#34381,#34382,
#34383,#34384,#34385,#34386,#34387,#34388,#34389,#34390,#34391,#34392,#34393,
#34394,#34395,#34396,#34397,#34398,#34399,#34400,#34401,#34402,#34403,#34404,
#34405,#34406,#34407,#34408,#34409,#34410,#34411,#34412,#34413,#34414,#34415,
#34416,#34417,#34418,#34419,#34420,#34421,#34422,#34423,#34424,#34425,#34426,
#34427,#34428,#34429,#34430,#34431,#34432,#34433,#34434,#34435,#34436,#34437,
#34438,#34439,#34440,#34441,#34442,#34443,#34444,#34445,#34446,#34447,#34448,
#34449,#34450,#34451,#34452,#34453,#34454,#34455,#34456,#34457,#34458,#34459,
#34460,#34461,#34462,#34463,#34464,#34465,#34466,#34467,#34468,#34469,#34470,
#34471,#34472,#34473,#34474,#34475,#34476,#34477,#34478,#34479,#34480,#34481,
#34482,#34483,#34484,#34485,#34486,#34487,#34488,#34489,#34490,#34491,#34492,
#34493,#34494,#34495,#34496,#34497,#34498,#34499,#34500,#34501,#34502,#34503,
#34504,#34505,#34506,#34507,#34508,#34509,#34510,#34511,#34512,#34513,#34514,
#34515,#34516,#34517,#34518,#34519,#34520,#34521,#34522,#34523,#34524,#34525,
#34526,#34527,#34528,#34529,#34530,#34531,#34532,#34533,#34534,#34535,#34536,
#34537,#34538,#34539,#34540,#34541,#34542,#34543,#34544,#34545,#34546,#34547,
#34548,#34549,#34550,#34551,#34552,#34553,#34554,#34555,#34556,#34557,#34558,
#34559,#34560,#34561,#34562,#34563,#34564,#34565,#34566,#34567,#34568,#34569,
#34570,#34571,#34572,#34573),(#34574,#34575,#34576,#34577,#34578,#34579,
#34580,#34581,#34582,#34583,#34584,#34585,#34586,#34587,#34588,#34589,#34590,
#34591,#34592,#34593,#34594,#34595,#34596,#34597,#34598,#34599,#34600,#34601,
#34602,#34603,#34604,#34605,#34606,#34607,#34608,#34609,#34610,#34611,#34612,
#34613,#34614,#34615,#34616,#34617,#34618,#34619,#34620,#34621,#34622,#34623,
#34624,#34625,#34626,#34627,#34628,#34629,#34630,#34631,#34632,#34633,#34634,
#34635,#34636,#34637,#34638,#34639,#34640,#34641,#34642,#34643,#34644,#34645,
#34646,#34647,#34648,#34649,#34650,#34651,#34652,#34653,#34654,#34655,#34656,
#34657,#34658,#34659,#34660,#34661,#34662,#34663,#34664,#34665,#34666,#34667,
#34668,#34669,#34670,#34671,#34672,#34673,#34674,#34675,#34676,#34677,#34678,
#34679,#34680,#34681,#34682,#34683,#34684,#34685,#34686,#34687,#34688,#34689,
#34690,#34691,#34692,#34693,#34694,#34695,#34696,#34697,#34698,#34699,#34700,
#34701,#34702,#34703,#34704,#34705,#34706,#34707,#34708,#34709,#34710,#34711,
#34712,#34713,#34714,#34715,#34716,#34717,#34718,#34719,#34720,#34721,#34722,
#34723,#34724,#34725,#34726,#34727,#34728,#34729,#34730,#34731,#34732,#34733,
#34734,#34735,#34736,#34737,#34738,#34739,#34740,#34741,#34742,#34743,#34744,
#34745,#34746,#34747,#34748,#34749,#34750,#34751,#34752,#34753,#34754,#34755,
#34756,#34757,#34758,#34759,#34760,#34761,#34762,#34763,#34764,#34765,#34766,
#34767,#34768,#34769,#34770,#34771,#34772,#34773,#34774,#34775,#34776,#34777,
#34778,#34779,#34780,#34781,#34782,#34783,#34784,#34785,#34786,#34787,#34788,
#34789,#34790,#34791,#34792,#34793,#34794,#34795,#34796,#34797,#34798,#34799,
#34800,#34801,#34802,#34803,#34804,#34805,#34806,#34807,#34808,#34809,#34810,
#34811,#34812,#34813,#34814,#34815,#34816,#34817,#34818,#34819,#34820,#34821,
#34822,#34823,#34824,#34825,#34826,#34827,#34828,#34829,#34830,#34831,#34832,
#34833,#34834,#34835,#34836,#34837,#34838,#34839,#34840,#34841,#34842,#34843,
#34844,#34845,#34846,#34847,#34848,#34849,#34850,#34851,#34852,#34853,#34854,
#34855,#34856,#34857,#34858,#34859,#34860,#34861,#34862,#34863,#34864,#34865,
#34866,#34867,#34868,#34869,#34870,#34871,#34872,#34873,#34874,#34875,#34876,
#34877,#34878,#34879,#34880,#34881,#34882,#34883,#34884,#34885,#34886,#34887,
#34888,#34889,#34890,#34891,#34892,#34893,#34894,#34895,#34896,#34897,#34898,
#34899,#34900,#34901,#34902,#34903,#34904,#34905,#34906,#34907,#34908,#34909,
#34910,#34911,#34912,#34913,#34914,#34915,#34916,#34917,#34918,#34919,#34920,
#34921,#34922,#34923,#34924,#34925,#34926,#34927,#34928,#34929,#34930,#34931,
#34932,#34933,#34934,#34935,#34936,#34937,#34938,#34939,#34940,#34941,#34942,
#34943,#34944,#34945,#34946,#34947,#34948,#34949,#34950,#34951,#34952,#34953,
#34954,#34955,#34956,#34957,#34958,#34959,#34960,#34961,#34962,#34963,#34964,
#34965,#34966,#34967,#34968,#34969,#34970,#34971,#34972,#34973,#34974,#34975,
#34976,#34977,#34978,#34979,#34980,#34981,#34982,#34983,#34984,#34985,#34986,
#34987,#34988,#34989,#34990,#34991,#34992,#34993,#34994,#34995,#34996,#34997,
#34998,#34999,#35000,#35001,#35002,#35003,#35004,#35005,#35006,#35007,#35008,
#35009,#35010,#35011,#35012,#35013,#35014,#35015,#35016,#35017,#35018,#35019,
#35020,#35021,#35022,#35023,#35024,#35025,#35026,#35027,#35028,#35029,#35030,
#35031,#35032,#35033,#35034,#35035,#35036,#35037,#35038,#35039,#35040,#35041,
#35042,#35043,#35044,#35045,#35046,#35047,#35048,#35049,#35050,#35051,#35052,
#35053,#35054,#35055,#35056,#35057,#35058,#35059,#35060,#35061,#35062,#35063,
#35064,#35065,#35066,#35067,#35068,#35069,#35070,#35071,#35072,#35073,#35074,
#35075,#35076,#35077,#35078,#35079,#35080,#35081,#35082,#35083,#35084,#35085,
#35086,#35087,#35088,#35089,#35090,#35091,#35092,#35093,#35094,#35095,#35096,
#35097,#35098,#35099,#35100,#35101,#35102,#35103,#35104,#35105,#35106,#35107,
#35108,#35109,#35110,#35111,#35112,#35113,#35114,#35115,#35116,#35117,#35118,
#35119,#35120,#35121,#35122,#35123,#35124,#35125,#35126,#35127,#35128,#35129,
#35130,#35131,#35132,#35133,#35134,#35135,#35136,#35137,#35138,#35139,#35140,
#35141,#35142,#35143,#35144,#35145,#35146,#35147,#35148,#35149,#35150,#35151,
#35152,#35153,#35154,#35155,#35156,#35157,#35158,#35159,#35160,#35161,#35162,
#35163,#35164,#35165,#35166,#35167,#35168,#35169,#35170,#35171,#35172,#35173,
#35174,#35175,#35176,#35177,#35178,#35179,#35180,#35181,#35182,#35183,#35184,
#35185,#35186,#35187,#35188,#35189,#35190,#35191,#35192,#35193,#35194,#35195,
#35196,#35197,#35198,#35199,#35200,#35201,#35202,#35203,#35204,#35205,#35206,
#35207,#35208,#35209,#35210,#35211,#35212,#35213,#35214,#35215,#35216,#35217,
#35218,#35219,#35220,#35221,#35222,#35223,#35224,#35225,#35226,#35227,#35228,
#35229,#35230,#35231,#35232,#35233,#35234,#35235,#35236,#35237,#35238,#35239,
#35240,#35241,#35242,#35243,#35244,#35245,#35246,#35247,#35248,#35249,#35250,
#35251,#35252,#35253,#35254,#35255,#35256,#35257,#35258,#35259,#35260,#35261,
#35262,#35263,#35264,#35265,#35266,#35267,#35268,#35269,#35270,#35271,#35272,
#35273,#35274,#35275,#35276,#35277,#35278,#35279,#35280,#35281,#35282,#35283,
#35284,#35285,#35286,#35287,#35288,#35289,#35290,#35291,#35292,#35293,#35294,
#35295,#35296,#35297,#35298,#35299,#35300,#35301,#35302,#35303,#35304,#35305,
#35306,#35307,#35308,#35309,#35310,#35311,#35312,#35313,#35314,#35315,#35316,
#35317,#35318,#35319,#35320,#35321,#35322,#35323,#35324,#35325,#35326,#35327,
#35328,#35329,#35330,#35331,#35332,#35333,#35334,#35335,#35336,#35337,#35338,
#35339,#35340,#35341,#35342,#35343,#35344,#35345,#35346,#35347,#35348,#35349,
#35350,#35351,#35352,#35353,#35354,#35355,#35356,#35357,#35358,#35359,#35360,
#35361,#35362,#35363,#35364,#35365,#35366,#35367,#35368,#35369,#35370,#35371,
#35372,#35373,#35374,#35375,#35376,#35377,#35378,#35379,#35380,#35381,#35382,
#35383,#35384,#35385,#35386,#35387,#35388,#35389,#35390,#35391,#35392,#35393,
#35394,#35395,#35396,#35397,#35398,#35399,#35400,#35401,#35402,#35403,#35404,
#35405,#35406,#35407,#35408,#35409,#35410,#35411,#35412,#35413,#35414,#35415,
#35416,#35417,#35418,#35419,#35420,#35421,#35422,#35423,#35424,#35425,#35426,
#35427,#35428,#35429,#35430,#35431,#35432,#35433,#35434,#35435,#35436,#35437,
#35438,#35439,#35440,#35441,#35442,#35443,#35444,#35445,#35446,#35447,#35448,
#35449,#35450,#35451,#35452,#35453,#35454,#35455,#35456,#35457,#35458,#35459,
#35460,#35461,#35462,#35463,#35464,#35465,#35466,#35467,#35468,#35469,#35470,
#35471,#35472,#35473,#35474,#35475,#35476,#35477,#35478,#35479,#35480,#35481,
#35482,#35483,#35484,#35485,#35486,#35487,#35488,#35489,#35490,#35491,#35492,
#35493,#35494,#35495,#35496,#35497,#35498,#35499,#35500,#35501,#35502,#35503,
#35504,#35505,#35506,#35507,#35508,#35509,#35510,#35511,#35512,#35513,#35514,
#35515,#35516,#35517,#35518,#35519,#35520,#35521,#35522,#35523,#35524,#35525,
#35526,#35527,#35528,#35529,#35530,#35531,#35532,#35533,#35534,#35535,#35536,
#35537,#35538,#35539,#35540,#35541,#35542,#35543,#35544,#35545,#35546),
(#35547,#35548,#35549,#35550,#35551,#35552,#35553,#35554,#35555,#35556,
#35557,#35558,#35559,#35560,#35561,#35562,#35563,#35564,#35565,#35566,#35567,
#35568,#35569,#35570,#35571,#35572,#35573,#35574,#35575,#35576,#35577,#35578,
#35579,#35580,#35581,#35582,#35583,#35584,#35585,#35586,#35587,#35588,#35589,
#35590,#35591,#35592,#35593,#35594,#35595,#35596,#35597,#35598,#35599,#35600,
#35601,#35602,#35603,#35604,#35605,#35606,#35607,#35608,#35609,#35610,#35611,
#35612,#35613,#35614,#35615,#35616,#35617,#35618,#35619,#35620,#35621,#35622,
#35623,#35624,#35625,#35626,#35627,#35628,#35629,#35630,#35631,#35632,#35633,
#35634,#35635,#35636,#35637,#35638,#35639,#35640,#35641,#35642,#35643,#35644,
#35645,#35646,#35647,#35648,#35649,#35650,#35651,#35652,#35653,#35654,#35655,
#35656,#35657,#35658,#35659,#35660,#35661,#35662,#35663,#35664,#35665,#35666,
#35667,#35668,#35669,#35670,#35671,#35672,#35673,#35674,#35675,#35676,#35677,
#35678,#35679,#35680,#35681,#35682,#35683,#35684,#35685,#35686,#35687,#35688,
#35689,#35690,#35691,#35692,#35693,#35694,#35695,#35696,#35697,#35698,#35699,
#35700,#35701,#35702,#35703,#35704,#35705,#35706,#35707,#35708,#35709,#35710,
#35711,#35712,#35713,#35714,#35715,#35716,#35717,#35718,#35719,#35720,#35721,
#35722,#35723,#35724,#35725,#35726,#35727,#35728,#35729,#35730,#35731,#35732,
#35733,#35734,#35735,#35736,#35737,#35738,#35739,#35740,#35741,#35742,#35743,
#35744,#35745,#35746,#35747,#35748,#35749,#35750,#35751,#35752,#35753,#35754,
#35755,#35756,#35757,#35758,#35759,#35760,#35761,#35762,#35763,#35764,#35765,
#35766,#35767,#35768,#35769,#35770,#35771,#35772,#35773,#35774,#35775,#35776,
#35777,#35778,#35779,#35780,#35781,#35782,#35783,#35784,#35785,#35786,#35787,
#35788,#35789,#35790,#35791,#35792,#35793,#35794,#35795,#35796,#35797,#35798,
#35799,#35800,#35801,#35802,#35803,#35804,#35805,#35806,#35807,#35808,#35809,
#35810,#35811,#35812,#35813,#35814,#35815,#35816,#35817,#35818,#35819,#35820,
#35821,#35822,#35823,#35824,#35825,#35826,#35827,#35828,#35829,#35830,#35831,
#35832,#35833,#35834,#35835,#35836,#35837,#35838,#35839,#35840,#35841,#35842,
#35843,#35844,#35845,#35846,#35847,#35848,#35849,#35850,#35851,#35852,#35853,
#35854,#35855,#35856,#35857,#35858,#35859,#35860,#35861,#35862,#35863,#35864,
#35865,#35866,#35867,#35868,#35869,#35870,#35871,#35872,#35873,#35874,#35875,
#35876,#35877,#35878,#35879,#35880,#35881,#35882,#35883,#35884,#35885,#35886,
#35887,#35888,#35889,#35890,#35891,#35892,#35893,#35894,#35895,#35896,#35897,
#35898,#35899,#35900,#35901,#35902,#35903,#35904,#35905,#35906,#35907,#35908,
#35909,#35910,#35911,#35912,#35913,#35914,#35915,#35916,#35917,#35918,#35919,
#35920,#35921,#35922,#35923,#35924,#35925,#35926,#35927,#35928,#35929,#35930,
#35931,#35932,#35933,#35934,#35935,#35936,#35937,#35938,#35939,#35940,#35941,
#35942,#35943,#35944,#35945,#35946,#35947,#35948,#35949,#35950,#35951,#35952,
#35953,#35954,#35955,#35956,#35957,#35958,#35959,#35960,#35961,#35962,#35963,
#35964,#35965,#35966,#35967,#35968,#35969,#35970,#35971,#35972,#35973,#35974,
#35975,#35976,#35977,#35978,#35979,#35980,#35981,#35982,#35983,#35984,#35985,
#35986,#35987,#35988,#35989,#35990,#35991,#35992,#35993,#35994,#35995,#35996,
#35997,#35998,#35999,#36000,#36001,#36002,#36003,#36004,#36005,#36006,#36007,
#36008,#36009,#36010,#36011,#36012,#36013,#36014,#36015,#36016,#36017,#36018,
#36019,#36020,#36021,#36022,#36023,#36024,#36025,#36026,#36027,#36028,#36029,
#36030,#36031,#36032,#36033,#36034,#36035,#36036,#36037,#36038,#36039,#36040,
#36041,#36042,#36043,#36044,#36045,#36046,#36047,#36048,#36049,#36050,#36051,
#36052,#36053,#36054,#36055,#36056,#36057,#36058,#36059,#36060,#36061,#36062,
#36063,#36064,#36065,#36066,#36067,#36068,#36069,#36070,#36071,#36072,#36073,
#36074,#36075,#36076,#36077,#36078,#36079,#36080,#36081,#36082,#36083,#36084,
#36085,#36086,#36087,#36088,#36089,#36090,#36091,#36092,#36093,#36094,#36095,
#36096,#36097,#36098,#36099,#36100,#36101,#36102,#36103,#36104,#36105,#36106,
#36107,#36108,#36109,#36110,#36111,#36112,#36113,#36114,#36115,#36116,#36117,
#36118,#36119,#36120,#36121,#36122,#36123,#36124,#36125,#36126,#36127,#36128,
#36129,#36130,#36131,#36132,#36133,#36134,#36135,#36136,#36137,#36138,#36139,
#36140,#36141,#36142,#36143,#36144,#36145,#36146,#36147,#36148,#36149,#36150,
#36151,#36152,#36153,#36154,#36155,#36156,#36157,#36158,#36159,#36160,#36161,
#36162,#36163,#36164,#36165,#36166,#36167,#36168,#36169,#36170,#36171,#36172,
#36173,#36174,#36175,#36176,#36177,#36178,#36179,#36180,#36181,#36182,#36183,
#36184,#36185,#36186,#36187,#36188,#36189,#36190,#36191,#36192,#36193,#36194,
#36195,#36196,#36197,#36198,#36199,#36200,#36201,#36202,#36203,#36204,#36205,
#36206,#36207,#36208,#36209,#36210,#36211,#36212,#36213,#36214,#36215,#36216,
#36217,#36218,#36219,#36220,#36221,#36222,#36223,#36224,#36225,#36226,#36227,
#36228,#36229,#36230,#36231,#36232,#36233,#36234,#36235,#36236,#36237,#36238,
#36239,#36240,#36241,#36242,#36243,#36244,#36245,#36246,#36247,#36248,#36249,
#36250,#36251,#36252,#36253,#36254,#36255,#36256,#36257,#36258,#36259,#36260,
#36261,#36262,#36263,#36264,#36265,#36266,#36267,#36268,#36269,#36270,#36271,
#36272,#36273,#36274,#36275,#36276,#36277,#36278,#36279,#36280,#36281,#36282,
#36283,#36284,#36285,#36286,#36287,#36288,#36289,#36290,#36291,#36292,#36293,
#36294,#36295,#36296,#36297,#36298,#36299,#36300,#36301,#36302,#36303,#36304,
#36305,#36306,#36307,#36308,#36309,#36310,#36311,#36312,#36313,#36314,#36315,
#36316,#36317,#36318,#36319,#36320,#36321,#36322,#36323,#36324,#36325,#36326,
#36327,#36328,#36329,#36330,#36331,#36332,#36333,#36334,#36335,#36336,#36337,
#36338,#36339,#36340,#36341,#36342,#36343,#36344,#36345,#36346,#36347,#36348,
#36349,#36350,#36351,#36352,#36353,#36354,#36355,#36356,#36357,#36358,#36359,
#36360,#36361,#36362,#36363,#36364,#36365,#36366,#36367,#36368,#36369,#36370,
#36371,#36372,#36373,#36374,#36375,#36376,#36377,#36378,#36379,#36380,#36381,
#36382,#36383,#36384,#36385,#36386,#36387,#36388,#36389,#36390,#36391,#36392,
#36393,#36394,#36395,#36396,#36397,#36398,#36399,#36400,#36401,#36402,#36403,
#36404,#36405,#36406,#36407,#36408,#36409,#36410,#36411,#36412,#36413,#36414,
#36415,#36416,#36417,#36418,#36419,#36420,#36421,#36422,#36423,#36424,#36425,
#36426,#36427,#36428,#36429,#36430,#36431,#36432,#36433,#36434,#36435,#36436,
#36437,#36438,#36439,#36440,#36441,#36442,#36443,#36444,#36445,#36446,#36447,
#36448,#36449,#36450,#36451,#36452,#36453,#36454,#36455,#36456,#36457,#36458,
#36459,#36460,#36461,#36462,#36463,#36464,#36465,#36466,#36467,#36468,#36469,
#36470,#36471,#36472,#36473,#36474,#36475,#36476,#36477,#36478,#36479,#36480,
#36481,#36482,#36483,#36484,#36485,#36486,#36487,#36488,#36489,#36490,#36491,
#36492,#36493,#36494,#36495,#36496,#36497,#36498,#36499,#36500,#36501,#36502,
#36503,#36504,#36505,#36506,#36507,#36508,#36509,#36510,#36511,#36512,#36513,
#36514,#36515,#36516,#36517,#36518,#36519)),.UNSPECIFIED.,.F.,.F.,.F.)
B_SPLINE_SURFACE_WITH_KNOTS((4,4),(3,2,2,2,2,2,2,2,2,2,2,2,2,2,2,2,2,2,
2,2,2,2,2,2,2,2,2,2,2,2,2,2,2,2,2,2,2,2,2,2,2,2,2,2,2,2,2,2,2,2,2,2,2,2,
2,2,2,2,2,2,2,2,2,2,2,2,2,2,2,2,2,2,2,2,2,2,2,2,2,2,2,2,2,2,2,2,2,2,2,2,
2,2,2,2,2,2,2,2,2,2,2,2,2,2,2,2,2,2,2,2,2,2,2,2,2,2,2,2,2,2,2,2,2,2,2,2,
2,2,2,2,2,2,2,2,2,2,2,2,2,2,2,2,2,2,2,2,2,2,2,2,2,2,2,2,2,2,2,2,2,2,2,2,
2,2,2,2,2,2,2,2,2,2,2,2,2,2,2,2,2,2,2,2,2,2,2,2,2,2,2,2,2,2,2,2,2,2,2,2,
2,2,2,2,2,2,2,2,2,2,2,2,2,2,2,2,2,2,2,2,2,2,2,2,2,2,2,2,2,2,2,2,2,2,2,2,
2,2,2,2,2,2,2,2,2,2,2,2,2,2,2,2,2,2,2,2,2,2,2,2,2,2,2,2,2,2,2,2,2,2,2,2,
2,2,2,2,2,2,2,2,2,2,2,2,2,2,2,2,2,2,2,2,2,2,2,2,2,2,2,2,2,2,2,2,2,2,2,2,
2,2,2,2,2,2,2,2,2,2,2,2,2,2,2,2,2,2,2,2,2,2,2,2,2,2,2,2,2,2,2,2,2,2,2,2,
2,2,2,2,2,2,2,2,2,2,2,2,2,2,2,2,2,2,2,2,2,2,2,2,2,2,2,2,2,2,2,2,2,2,2,2,
2,2,2,2,2,2,2,2,2,2,2,2,2,2,2,2,2,2,2,2,2,2,2,2,2,2,2,2,2,2,2,2,2,2,2,2,
2,2,2,2,2,2,2,2,2,2,2,2,2,2,2,2,2,2,2,2,2,2,2,2,2,2,2,2,2,2,2,2,2,2,2,2,
2,2,2,2,2,2,2,2,2,2,2,2,2,2,2,2,2,2,2,2,2,2,2,2,2,2,2,2,2,2,2,2,2,2,2,2,
3),(0.,1.),(0.,0.00205761316872428,0.00411522633744856,0.00617283950617284,
0.00823045267489712,0.0102880658436214,0.0123456790123457,0.01440329218107,
0.0164609053497942,0.0185185185185185,0.0205761316872428,0.0226337448559671,
0.0246913580246914,0.0267489711934156,0.0288065843621399,0.0308641975308642,
0.0329218106995885,0.0349794238683128,0.037037037037037,0.0390946502057613,
0.0411522633744856,0.0432098765432099,0.0452674897119342,0.0473251028806584,
0.0493827160493827,0.051440329218107,0.0534979423868313,0.0555555555555556,
0.0576131687242798,0.0596707818930041,0.0617283950617284,0.0637860082304527,
0.065843621399177,0.0679012345679012,0.0699588477366255,0.0720164609053498,
0.0740740740740741,0.0761316872427984,0.0781893004115226,0.0802469135802469,
0.0823045267489712,0.0843621399176955,0.0864197530864197,0.088477366255144,
0.0905349794238683,0.0925925925925926,0.0946502057613169,0.0967078189300412,
0.0987654320987654,0.10082304526749,0.102880658436214,0.104938271604938,
0.106995884773663,0.109053497942387,0.111111111111111,0.113168724279835,
0.11522633744856,0.117283950617284,0.119341563786008,0.121399176954733,
0.123456790123457,0.125514403292181,0.127572016460905,0.12962962962963,
0.131687242798354,0.133744855967078,0.135802469135802,0.137860082304527,
0.139917695473251,0.141975308641975,0.1440329218107,0.146090534979424,0.148148148148148,
0.150205761316872,0.152263374485597,0.154320987654321,0.156378600823045,
0.15843621399177,0.160493827160494,0.162551440329218,0.164609053497942,
0.166666666666667,0.168724279835391,0.170781893004115,0.172839506172839,
0.174897119341564,0.176954732510288,0.179012345679012,0.181069958847737,
0.183127572016461,0.185185185185185,0.187242798353909,0.189300411522634,
0.191358024691358,0.193415637860082,0.195473251028807,0.197530864197531,
0.199588477366255,0.201646090534979,0.203703703703704,0.205761316872428,
0.207818930041152,0.209876543209877,0.211934156378601,0.213991769547325,
0.216049382716049,0.218106995884774,0.220164609053498,0.222222222222222,
0.224279835390947,0.226337448559671,0.228395061728395,0.230452674897119,
0.232510288065844,0.234567901234568,0.236625514403292,0.238683127572016,
0.240740740740741,0.242798353909465,0.244855967078189,0.246913580246914,
0.248971193415638,0.251028806584362,0.253086419753086,0.255144032921811,
0.257201646090535,0.259259259259259,0.261316872427984,0.263374485596708,
0.265432098765432,0.267489711934156,0.269547325102881,0.271604938271605,
0.273662551440329,0.275720164609054,0.277777777777778,0.279835390946502,
0.281893004115226,0.283950617283951,0.286008230452675,0.288065843621399,
0.290123456790123,0.292181069958848,0.294238683127572,0.296296296296296,
0.298353909465021,0.300411522633745,0.302469135802469,0.304526748971193,
0.306584362139918,0.308641975308642,0.310699588477366,0.312757201646091,
0.314814814814815,0.316872427983539,0.318930041152263,0.320987654320988,
0.323045267489712,0.325102880658436,0.327160493827161,0.329218106995885,
0.331275720164609,0.333333333333333,0.335390946502058,0.337448559670782,
0.339506172839506,0.34156378600823,0.343621399176955,0.345679012345679,
0.347736625514403,0.349794238683128,0.351851851851852,0.353909465020576,
0.3559670781893,0.358024691358025,0.360082304526749,0.362139917695473,0.364197530864198,
0.366255144032922,0.368312757201646,0.37037037037037,0.372427983539095,
0.374485596707819,0.376543209876543,0.378600823045267,0.380658436213992,
0.382716049382716,0.38477366255144,0.386831275720165,0.388888888888889,
0.390946502057613,0.393004115226337,0.395061728395062,0.397119341563786,
0.39917695473251,0.401234567901235,0.403292181069959,0.405349794238683,
0.407407407407407,0.409465020576132,0.411522633744856,0.41358024691358,
0.415637860082305,0.417695473251029,0.419753086419753,0.421810699588477,
0.423868312757202,0.425925925925926,0.42798353909465,0.430041152263374,
0.432098765432099,0.434156378600823,0.436213991769547,0.438271604938272,
0.440329218106996,0.44238683127572,0.444444444444444,0.446502057613169,
0.448559670781893,0.450617283950617,0.452674897119342,0.454732510288066,
0.45679012345679,0.458847736625514,0.460905349794239,0.462962962962963,
0.465020576131687,0.467078189300412,0.469135802469136,0.47119341563786,
0.473251028806584,0.475308641975309,0.477366255144033,0.479423868312757,
0.481481481481481,0.483539094650206,0.48559670781893,0.487654320987654,
0.489711934156379,0.491769547325103,0.493827160493827,0.495884773662551,
0.497942386831276,0.5,0.502057613168724,0.504115226337449,0.506172839506173,
0.508230452674897,0.510288065843621,0.512345679012346,0.51440329218107,
0.516460905349794,0.518518518518518,0.520576131687243,0.522633744855967,
0.524691358024691,0.526748971193416,0.52880658436214,0.530864197530864,
0.532921810699588,0.534979423868313,0.537037037037037,0.539094650205761,
0.541152263374486,0.54320987654321,0.545267489711934,0.547325102880658,
0.549382716049383,0.551440329218107,0.553497942386831,0.555555555555556,
0.55761316872428,0.559670781893004,0.561728395061728,0.563786008230453,
0.565843621399177,0.567901234567901,0.569958847736626,0.57201646090535,
0.574074074074074,0.576131687242798,0.578189300411523,0.580246913580247,
0.582304526748971,0.584362139917695,0.58641975308642,0.588477366255144,
0.590534979423868,0.592592592592593,0.594650205761317,0.596707818930041,
0.598765432098765,0.60082304526749,0.602880658436214,0.604938271604938,
0.606995884773663,0.609053497942387,0.611111111111111,0.613168724279835,
0.61522633744856,0.617283950617284,0.619341563786008,0.621399176954732,
0.623456790123457,0.625514403292181,0.627572016460905,0.62962962962963,
0.631687242798354,0.633744855967078,0.635802469135803,0.637860082304527,
0.639917695473251,0.641975308641975,0.6440329218107,0.646090534979424,0.648148148148148,
0.650205761316872,0.652263374485597,0.654320987654321,0.656378600823045,
0.65843621399177,0.660493827160494,0.662551440329218,0.664609053497942,
0.666666666666667,0.668724279835391,0.670781893004115,0.672839506172839,
0.674897119341564,0.676954732510288,0.679012345679012,0.681069958847737,
0.683127572016461,0.685185185185185,0.687242798353909,0.689300411522634,
0.691358024691358,0.693415637860082,0.695473251028807,0.697530864197531,
0.699588477366255,0.701646090534979,0.703703703703704,0.705761316872428,
0.707818930041152,0.709876543209877,0.711934156378601,0.713991769547325,
0.716049382716049,0.718106995884774,0.720164609053498,0.722222222222222,
0.724279835390947,0.726337448559671,0.728395061728395,0.730452674897119,
0.732510288065844,0.734567901234568,0.736625514403292,0.738683127572016,
0.740740740740741,0.742798353909465,0.744855967078189,0.746913580246914,
0.748971193415638,0.751028806584362,0.753086419753086,0.755144032921811,
0.757201646090535,0.759259259259259,0.761316872427984,0.763374485596708,
0.765432098765432,0.767489711934156,0.769547325102881,0.771604938271605,
0.773662551440329,0.775720164609053,0.777777777777778,0.779835390946502,
0.781893004115226,0.783950617283951,0.786008230452675,0.788065843621399,
0.790123456790123,0.792181069958848,0.794238683127572,0.796296296296296,
0.798353909465021,0.800411522633745,0.802469135802469,0.804526748971193,
0.806584362139918,0.808641975308642,0.810699588477366,0.812757201646091,
0.814814814814815,0.816872427983539,0.818930041152263,0.820987654320988,
0.823045267489712,0.825102880658436,0.827160493827161,0.829218106995885,
0.831275720164609,0.833333333333333,0.835390946502058,0.837448559670782,
0.839506172839506,0.84156378600823,0.843621399176955,0.845679012345679,
0.847736625514403,0.849794238683128,0.851851851851852,0.853909465020576,
0.8559670781893,0.858024691358025,0.860082304526749,0.862139917695473,0.864197530864197,
0.866255144032922,0.868312757201646,0.87037037037037,0.872427983539095,
0.874485596707819,0.876543209876543,0.878600823045268,0.880658436213992,
0.882716049382716,0.88477366255144,0.886831275720165,0.888888888888889,
0.890946502057613,0.893004115226337,0.895061728395062,0.897119341563786,
0.89917695473251,0.901234567901235,0.903292181069959,0.905349794238683,
0.907407407407407,0.909465020576132,0.911522633744856,0.91358024691358,
0.915637860082305,0.917695473251029,0.919753086419753,0.921810699588477,
0.923868312757202,0.925925925925926,0.92798353909465,0.930041152263374,
0.932098765432099,0.934156378600823,0.936213991769547,0.938271604938272,
0.940329218106996,0.94238683127572,0.944444444444444,0.946502057613169,
0.948559670781893,0.950617283950617,0.952674897119342,0.954732510288066,
0.95679012345679,0.958847736625514,0.960905349794239,0.962962962962963,
0.965020576131687,0.967078189300412,0.969135802469136,0.97119341563786,
0.973251028806584,0.975308641975309,0.977366255144033,0.979423868312757,
0.981481481481482,0.983539094650206,0.98559670781893,0.987654320987654,
0.989711934156379,0.991769547325103,0.993827160493827,0.995884773662551,
0.997942386831276,1.),.UNSPECIFIED.)
GEOMETRIC_REPRESENTATION_ITEM()
RATIONAL_B_SPLINE_SURFACE(((1.,0.866025403784439,1.,0.866025403784439,1.,
0.866025403784439,1.,0.866025403784439,1.,0.866025403784439,1.,0.866025403784439,
1.,0.866025403784439,1.,0.866025403784439,1.,0.866025403784439,1.,0.866025403784439,
1.,0.866025403784439,1.,0.866025403784439,1.,0.866025403784439,1.,0.866025403784439,
1.,0.866025403784439,1.,0.866025403784439,1.,0.866025403784439,1.,0.866025403784439,
1.,0.866025403784439,1.,0.866025403784439,1.,0.866025403784439,1.,0.866025403784439,
1.,0.866025403784439,1.,0.866025403784439,1.,0.866025403784439,1.,0.866025403784439,
1.,0.866025403784439,1.,0.866025403784439,1.,0.866025403784439,1.,0.866025403784439,
1.,0.866025403784439,1.,0.866025403784439,1.,0.866025403784439,1.,0.866025403784439,
1.,0.866025403784439,1.,0.866025403784439,1.,0.866025403784439,1.,0.866025403784439,
1.,0.866025403784439,1.,0.866025403784439,1.,0.866025403784439,1.,0.866025403784439,
1.,0.866025403784439,1.,0.866025403784439,1.,0.866025403784439,1.,0.866025403784439,
1.,0.866025403784439,1.,0.866025403784439,1.,0.866025403784439,1.,0.866025403784439,
1.,0.866025403784439,1.,0.866025403784439,1.,0.866025403784439,1.,0.866025403784439,
1.,0.866025403784439,1.,0.866025403784439,1.,0.866025403784439,1.,0.866025403784439,
1.,0.866025403784439,1.,0.866025403784439,1.,0.866025403784439,1.,0.866025403784439,
1.,0.866025403784439,1.,0.866025403784439,1.,0.866025403784439,1.,0.866025403784439,
1.,0.866025403784439,1.,0.866025403784439,1.,0.866025403784439,1.,0.866025403784439,
1.,0.866025403784439,1.,0.866025403784439,1.,0.866025403784439,1.,0.866025403784439,
1.,0.866025403784439,1.,0.866025403784439,1.,0.866025403784439,1.,0.866025403784439,
1.,0.866025403784439,1.,0.866025403784439,1.,0.866025403784439,1.,0.866025403784439,
1.,0.866025403784439,1.,0.866025403784439,1.,0.866025403784439,1.,0.866025403784439,
1.,0.866025403784439,1.,0.866025403784439,1.,0.866025403784439,1.,0.866025403784439,
1.,0.866025403784439,1.,0.866025403784439,1.,0.866025403784439,1.,0.866025403784439,
1.,0.866025403784439,1.,0.866025403784439,1.,0.866025403784439,1.,0.866025403784439,
1.,0.866025403784439,1.,0.866025403784439,1.,0.866025403784439,1.,0.866025403784439,
1.,0.866025403784439,1.,0.866025403784439,1.,0.866025403784439,1.,0.866025403784439,
1.,0.866025403784439,1.,0.866025403784439,1.,0.866025403784439,1.,0.866025403784439,
1.,0.866025403784439,1.,0.866025403784439,1.,0.866025403784439,1.,0.866025403784439,
1.,0.866025403784439,1.,0.866025403784439,1.,0.866025403784439,1.,0.866025403784439,
1.,0.866025403784439,1.,0.866025403784439,1.,0.866025403784439,1.,0.866025403784439,
1.,0.866025403784439,1.,0.866025403784439,1.,0.866025403784439,1.,0.866025403784439,
1.,0.866025403784439,1.,0.866025403784439,1.,0.866025403784439,1.,0.866025403784439,
1.,0.866025403784439,1.,0.866025403784439,1.,0.866025403784439,1.,0.866025403784439,
1.,0.866025403784439,1.,0.866025403784439,1.,0.866025403784439,1.,0.866025403784439,
1.,0.866025403784439,1.,0.866025403784439,1.,0.866025403784439,1.,0.866025403784439,
1.,0.866025403784439,1.,0.866025403784439,1.,0.866025403784439,1.,0.866025403784439,
1.,0.866025403784439,1.,0.866025403784439,1.,0.866025403784439,1.,0.866025403784439,
1.,0.866025403784439,1.,0.866025403784439,1.,0.866025403784439,1.,0.866025403784439,
1.,0.866025403784439,1.,0.866025403784439,1.,0.866025403784439,1.,0.866025403784439,
1.,0.866025403784439,1.,0.866025403784439,1.,0.866025403784439,1.,0.866025403784439,
1.,0.866025403784439,1.,0.866025403784439,1.,0.866025403784439,1.,0.866025403784439,
1.,0.866025403784439,1.,0.866025403784439,1.,0.866025403784439,1.,0.866025403784439,
1.,0.866025403784439,1.,0.866025403784439,1.,0.866025403784439,1.,0.866025403784439,
1.,0.866025403784439,1.,0.866025403784439,1.,0.866025403784439,1.,0.866025403784439,
1.,0.866025403784439,1.,0.866025403784439,1.,0.866025403784439,1.,0.866025403784439,
1.,0.866025403784439,1.,0.866025403784439,1.,0.866025403784439,1.,0.866025403784439,
1.,0.866025403784439,1.,0.866025403784439,1.,0.866025403784439,1.,0.866025403784439,
1.,0.866025403784439,1.,0.866025403784439,1.,0.866025403784439,1.,0.866025403784439,
1.,0.866025403784439,1.,0.866025403784439,1.,0.866025403784439,1.,0.866025403784439,
1.,0.866025403784439,1.,0.866025403784439,1.,0.866025403784439,1.,0.866025403784439,
1.,0.866025403784439,1.,0.866025403784439,1.,0.866025403784439,1.,0.866025403784439,
1.,0.866025403784439,1.,0.866025403784439,1.,0.866025403784439,1.,0.866025403784439,
1.,0.866025403784439,1.,0.866025403784439,1.,0.866025403784439,1.,0.866025403784439,
1.,0.866025403784439,1.,0.866025403784439,1.,0.866025403784439,1.,0.866025403784439,
1.,0.866025403784439,1.,0.866025403784439,1.,0.866025403784439,1.,0.866025403784439,
1.,0.866025403784439,1.,0.866025403784439,1.,0.866025403784439,1.,0.866025403784439,
1.,0.866025403784439,1.,0.866025403784439,1.,0.866025403784439,1.,0.866025403784439,
1.,0.866025403784439,1.,0.866025403784439,1.,0.866025403784439,1.,0.866025403784439,
1.,0.866025403784439,1.,0.866025403784439,1.,0.866025403784439,1.,0.866025403784439,
1.,0.866025403784439,1.,0.866025403784439,1.,0.866025403784439,1.,0.866025403784439,
1.,0.866025403784439,1.,0.866025403784439,1.,0.866025403784439,1.,0.866025403784439,
1.,0.866025403784439,1.,0.866025403784439,1.,0.866025403784439,1.,0.866025403784439,
1.,0.866025403784439,1.,0.866025403784439,1.,0.866025403784439,1.,0.866025403784439,
1.,0.866025403784439,1.,0.866025403784439,1.,0.866025403784439,1.,0.866025403784439,
1.,0.866025403784439,1.,0.866025403784439,1.,0.866025403784439,1.,0.866025403784439,
1.,0.866025403784439,1.,0.866025403784439,1.,0.866025403784439,1.,0.866025403784439,
1.,0.866025403784439,1.,0.866025403784439,1.,0.866025403784439,1.,0.866025403784439,
1.,0.866025403784439,1.,0.866025403784439,1.,0.866025403784439,1.,0.866025403784439,
1.,0.866025403784439,1.,0.866025403784439,1.,0.866025403784439,1.,0.866025403784439,
1.,0.866025403784439,1.,0.866025403784439,1.,0.866025403784439,1.,0.866025403784439,
1.,0.866025403784439,1.,0.866025403784439,1.,0.866025403784439,1.,0.866025403784439,
1.,0.866025403784439,1.,0.866025403784439,1.,0.866025403784439,1.,0.866025403784439,
1.,0.866025403784439,1.,0.866025403784439,1.,0.866025403784439,1.,0.866025403784439,
1.,0.866025403784439,1.,0.866025403784439,1.,0.866025403784439,1.,0.866025403784439,
1.,0.866025403784439,1.,0.866025403784439,1.,0.866025403784439,1.,0.866025403784439,
1.,0.866025403784439,1.,0.866025403784439,1.,0.866025403784439,1.,0.866025403784439,
1.,0.866025403784439,1.,0.866025403784439,1.,0.866025403784439,1.,0.866025403784439,
1.,0.866025403784439,1.,0.866025403784439,1.,0.866025403784439,1.,0.866025403784439,
1.,0.866025403784439,1.,0.866025403784439,1.,0.866025403784439,1.,0.866025403784439,
1.,0.866025403784439,1.,0.866025403784439,1.,0.866025403784439,1.,0.866025403784439,
1.,0.866025403784439,1.,0.866025403784439,1.,0.866025403784439,1.,0.866025403784439,
1.,0.866025403784439,1.,0.866025403784439,1.,0.866025403784439,1.,0.866025403784439,
1.,0.866025403784439,1.,0.866025403784439,1.,0.866025403784439,1.,0.866025403784439,
1.,0.866025403784439,1.,0.866025403784439,1.,0.866025403784439,1.,0.866025403784439,
1.,0.866025403784439,1.,0.866025403784439,1.,0.866025403784439,1.,0.866025403784439,
1.,0.866025403784439,1.,0.866025403784439,1.,0.866025403784439,1.,0.866025403784439,
1.,0.866025403784439,1.,0.866025403784439,1.,0.866025403784439,1.,0.866025403784439,
1.,0.866025403784439,1.,0.866025403784439,1.,0.866025403784439,1.,0.866025403784439,
1.,0.866025403784439,1.,0.866025403784439,1.,0.866025403784439,1.,0.866025403784439,
1.,0.866025403784439,1.,0.866025403784439,1.,0.866025403784439,1.,0.866025403784439,
1.,0.866025403784439,1.,0.866025403784439,1.,0.866025403784439,1.,0.866025403784439,
1.,0.866025403784439,1.,0.866025403784439,1.,0.866025403784439,1.,0.866025403784439,
1.,0.866025403784439,1.,0.866025403784439,1.,0.866025403784439,1.,0.866025403784439,
1.,0.866025403784439,1.,0.866025403784439,1.,0.866025403784439,1.,0.866025403784439,
1.,0.866025403784439,1.,0.866025403784439,1.,0.866025403784439,1.,0.866025403784439,
1.,0.866025403784439,1.,0.866025403784439,1.,0.866025403784439,1.,0.866025403784439,
1.,0.866025403784439,1.,0.866025403784439,1.,0.866025403784439,1.,0.866025403784439,
1.,0.866025403784439,1.,0.866025403784439,1.,0.866025403784439,1.,0.866025403784439,
1.,0.866025403784439,1.,0.866025403784439,1.,0.866025403784439,1.,0.866025403784439,
1.,0.866025403784439,1.,0.866025403784439,1.,0.866025403784439,1.,0.866025403784439,
1.,0.866025403784439,1.,0.866025403784439,1.,0.866025403784439,1.,0.866025403784439,
1.,0.866025403784439,1.,0.866025403784439,1.,0.866025403784439,1.,0.866025403784439,
1.,0.866025403784439,1.,0.866025403784439,1.,0.866025403784439,1.,0.866025403784439,
1.,0.866025403784439,1.,0.866025403784439,1.,0.866025403784439,1.,0.866025403784439,
1.,0.866025403784439,1.,0.866025403784439,1.,0.866025403784439,1.,0.866025403784439,
1.,0.866025403784439,1.,0.866025403784439,1.,0.866025403784439,1.,0.866025403784439,
1.,0.866025403784439,1.,0.866025403784439,1.,0.866025403784439,1.,0.866025403784439,
1.,0.866025403784439,1.,0.866025403784439,1.,0.866025403784439,1.,0.866025403784439,
1.,0.866025403784439,1.,0.866025403784439,1.,0.866025403784439,1.,0.866025403784439,
1.,0.866025403784439,1.,0.866025403784439,1.,0.866025403784439,1.,0.866025403784439,
1.,0.866025403784439,1.,0.866025403784439,1.,0.866025403784439,1.,0.866025403784439,
1.,0.866025403784439,1.,0.866025403784439,1.,0.866025403784439,1.,0.866025403784439,
1.,0.866025403784439,1.,0.866025403784439,1.,0.866025403784439,1.,0.866025403784439,
1.,0.866025403784439,1.,0.866025403784439,1.,0.866025403784439,1.,0.866025403784439,
1.,0.866025403784439,1.,0.866025403784439,1.,0.866025403784439,1.,0.866025403784439,
1.,0.866025403784439,1.,0.866025403784439,1.,0.866025403784439,1.,0.866025403784439,
1.,0.866025403784439,1.,0.866025403784439,1.,0.866025403784439,1.,0.866025403784439,
1.,0.866025403784439,1.,0.866025403784439,1.,0.866025403784439,1.,0.866025403784439,
1.,0.866025403784439,1.,0.866025403784439,1.,0.866025403784439,1.,0.866025403784439,
1.,0.866025403784439,1.,0.866025403784439,1.,0.866025403784439,1.,0.866025403784439,
1.,0.866025403784439,1.,0.866025403784439,1.,0.866025403784439,1.,0.866025403784439,
1.),(0.641165742156689,0.555265820743996,0.641165742156689,0.555265820743996,
0.641165742156689,0.555265820743996,0.641165742156689,0.555265820743996,
0.641165742156689,0.555265820743996,0.641165742156689,0.555265820743996,
0.641165742156689,0.555265820743996,0.641165742156689,0.555265820743996,
0.641165742156689,0.555265820743996,0.641165742156689,0.555265820743996,
0.641165742156689,0.555265820743996,0.641165742156689,0.555265820743996,
0.641165742156689,0.555265820743996,0.641165742156689,0.555265820743996,
0.641165742156689,0.555265820743996,0.641165742156689,0.555265820743996,
0.641165742156689,0.555265820743996,0.641165742156689,0.555265820743996,
0.641165742156689,0.555265820743996,0.641165742156689,0.555265820743996,
0.641165742156689,0.555265820743996,0.641165742156689,0.555265820743996,
0.641165742156689,0.555265820743996,0.641165742156689,0.555265820743996,
0.641165742156689,0.555265820743996,0.641165742156689,0.555265820743996,
0.641165742156689,0.555265820743996,0.641165742156689,0.555265820743996,
0.641165742156689,0.555265820743996,0.641165742156689,0.555265820743996,
0.641165742156689,0.555265820743996,0.641165742156689,0.555265820743996,
0.641165742156689,0.555265820743996,0.641165742156689,0.555265820743996,
0.641165742156689,0.555265820743996,0.641165742156689,0.555265820743996,
0.641165742156689,0.555265820743996,0.641165742156689,0.555265820743996,
0.641165742156689,0.555265820743996,0.641165742156689,0.555265820743996,
0.641165742156689,0.555265820743996,0.641165742156689,0.555265820743996,
0.641165742156689,0.555265820743996,0.641165742156689,0.555265820743996,
0.641165742156689,0.555265820743996,0.641165742156689,0.555265820743996,
0.641165742156689,0.555265820743996,0.641165742156689,0.555265820743996,
0.641165742156689,0.555265820743996,0.641165742156689,0.555265820743996,
0.641165742156689,0.555265820743996,0.641165742156689,0.555265820743996,
0.641165742156689,0.555265820743996,0.641165742156689,0.555265820743996,
0.641165742156689,0.555265820743996,0.641165742156689,0.555265820743996,
0.641165742156689,0.555265820743996,0.641165742156689,0.555265820743996,
0.641165742156689,0.555265820743996,0.641165742156689,0.555265820743996,
0.641165742156689,0.555265820743996,0.641165742156689,0.555265820743996,
0.641165742156689,0.555265820743996,0.641165742156689,0.555265820743996,
0.641165742156689,0.555265820743996,0.641165742156689,0.555265820743996,
0.641165742156689,0.555265820743996,0.641165742156689,0.555265820743996,
0.641165742156689,0.555265820743996,0.641165742156689,0.555265820743996,
0.641165742156689,0.555265820743996,0.641165742156689,0.555265820743996,
0.641165742156689,0.555265820743996,0.641165742156689,0.555265820743996,
0.641165742156689,0.555265820743996,0.641165742156689,0.555265820743996,
0.641165742156689,0.555265820743996,0.641165742156689,0.555265820743996,
0.641165742156689,0.555265820743996,0.641165742156689,0.555265820743996,
0.641165742156689,0.555265820743996,0.641165742156689,0.555265820743996,
0.641165742156689,0.555265820743996,0.641165742156689,0.555265820743996,
0.641165742156689,0.555265820743996,0.641165742156689,0.555265820743996,
0.641165742156689,0.555265820743996,0.641165742156689,0.555265820743996,
0.641165742156689,0.555265820743996,0.641165742156689,0.555265820743996,
0.641165742156689,0.555265820743996,0.641165742156689,0.555265820743996,
0.641165742156689,0.555265820743996,0.641165742156689,0.555265820743996,
0.641165742156689,0.555265820743996,0.641165742156689,0.555265820743996,
0.641165742156689,0.555265820743996,0.641165742156689,0.555265820743996,
0.641165742156689,0.555265820743996,0.641165742156689,0.555265820743996,
0.641165742156689,0.555265820743996,0.641165742156689,0.555265820743996,
0.641165742156689,0.555265820743996,0.641165742156689,0.555265820743996,
0.641165742156689,0.555265820743996,0.641165742156689,0.555265820743996,
0.641165742156689,0.555265820743996,0.641165742156689,0.555265820743996,
0.641165742156689,0.555265820743996,0.641165742156689,0.555265820743996,
0.641165742156689,0.555265820743996,0.641165742156689,0.555265820743996,
0.641165742156689,0.555265820743996,0.641165742156689,0.555265820743996,
0.641165742156689,0.555265820743996,0.641165742156689,0.555265820743996,
0.641165742156689,0.555265820743996,0.641165742156689,0.555265820743996,
0.641165742156689,0.555265820743996,0.641165742156689,0.555265820743996,
0.641165742156689,0.555265820743996,0.641165742156689,0.555265820743996,
0.641165742156689,0.555265820743996,0.641165742156689,0.555265820743996,
0.641165742156689,0.555265820743996,0.641165742156689,0.555265820743996,
0.641165742156689,0.555265820743996,0.641165742156689,0.555265820743996,
0.641165742156689,0.555265820743996,0.641165742156689,0.555265820743996,
0.641165742156689,0.555265820743996,0.641165742156689,0.555265820743996,
0.641165742156689,0.555265820743996,0.641165742156689,0.555265820743996,
0.641165742156689,0.555265820743996,0.641165742156689,0.555265820743996,
0.641165742156689,0.555265820743996,0.641165742156689,0.555265820743996,
0.641165742156689,0.555265820743996,0.641165742156689,0.555265820743996,
0.641165742156689,0.555265820743996,0.641165742156689,0.555265820743996,
0.641165742156689,0.555265820743996,0.641165742156689,0.555265820743996,
0.641165742156689,0.555265820743996,0.641165742156689,0.555265820743996,
0.641165742156689,0.555265820743996,0.641165742156689,0.555265820743996,
0.641165742156689,0.555265820743996,0.641165742156689,0.555265820743996,
0.641165742156689,0.555265820743996,0.641165742156689,0.555265820743996,
0.641165742156689,0.555265820743996,0.641165742156689,0.555265820743996,
0.641165742156689,0.555265820743996,0.641165742156689,0.555265820743996,
0.641165742156689,0.555265820743996,0.641165742156689,0.555265820743996,
0.641165742156689,0.555265820743996,0.641165742156689,0.555265820743996,
0.641165742156689,0.555265820743996,0.641165742156689,0.555265820743996,
0.641165742156689,0.555265820743996,0.641165742156689,0.555265820743996,
0.641165742156689,0.555265820743996,0.641165742156689,0.555265820743996,
0.641165742156689,0.555265820743996,0.641165742156689,0.555265820743996,
0.641165742156689,0.555265820743996,0.641165742156689,0.555265820743996,
0.641165742156689,0.555265820743996,0.641165742156689,0.555265820743996,
0.641165742156689,0.555265820743996,0.641165742156689,0.555265820743996,
0.641165742156689,0.555265820743996,0.641165742156689,0.555265820743996,
0.641165742156689,0.555265820743996,0.641165742156689,0.555265820743996,
0.641165742156689,0.555265820743996,0.641165742156689,0.555265820743996,
0.641165742156689,0.555265820743996,0.641165742156689,0.555265820743996,
0.641165742156689,0.555265820743996,0.641165742156689,0.555265820743996,
0.641165742156689,0.555265820743996,0.641165742156689,0.555265820743996,
0.641165742156689,0.555265820743996,0.641165742156689,0.555265820743996,
0.641165742156689,0.555265820743996,0.641165742156689,0.555265820743996,
0.641165742156689,0.555265820743996,0.641165742156689,0.555265820743996,
0.641165742156689,0.555265820743996,0.641165742156689,0.555265820743996,
0.641165742156689,0.555265820743996,0.641165742156689,0.555265820743996,
0.641165742156689,0.555265820743996,0.641165742156689,0.555265820743996,
0.641165742156689,0.555265820743996,0.641165742156689,0.555265820743996,
0.641165742156689,0.555265820743996,0.641165742156689,0.555265820743996,
0.641165742156689,0.555265820743996,0.641165742156689,0.555265820743996,
0.641165742156689,0.555265820743996,0.641165742156689,0.555265820743996,
0.641165742156689,0.555265820743996,0.641165742156689,0.555265820743996,
0.641165742156689,0.555265820743996,0.641165742156689,0.555265820743996,
0.641165742156689,0.555265820743996,0.641165742156689,0.555265820743996,
0.641165742156689,0.555265820743996,0.641165742156689,0.555265820743996,
0.641165742156689,0.555265820743996,0.641165742156689,0.555265820743996,
0.641165742156689,0.555265820743996,0.641165742156689,0.555265820743996,
0.641165742156689,0.555265820743996,0.641165742156689,0.555265820743996,
0.641165742156689,0.555265820743996,0.641165742156689,0.555265820743996,
0.641165742156689,0.555265820743996,0.641165742156689,0.555265820743996,
0.641165742156689,0.555265820743996,0.641165742156689,0.555265820743996,
0.641165742156689,0.555265820743996,0.641165742156689,0.555265820743996,
0.641165742156689,0.555265820743996,0.641165742156689,0.555265820743996,
0.641165742156689,0.555265820743996,0.641165742156689,0.555265820743996,
0.641165742156689,0.555265820743996,0.641165742156689,0.555265820743996,
0.641165742156689,0.555265820743996,0.641165742156689,0.555265820743996,
0.641165742156689,0.555265820743996,0.641165742156689,0.555265820743996,
0.641165742156689,0.555265820743996,0.641165742156689,0.555265820743996,
0.641165742156689,0.555265820743996,0.641165742156689,0.555265820743996,
0.641165742156689,0.555265820743996,0.641165742156689,0.555265820743996,
0.641165742156689,0.555265820743996,0.641165742156689,0.555265820743996,
0.641165742156689,0.555265820743996,0.641165742156689,0.555265820743996,
0.641165742156689,0.555265820743996,0.641165742156689,0.555265820743996,
0.641165742156689,0.555265820743996,0.641165742156689,0.555265820743996,
0.641165742156689,0.555265820743996,0.641165742156689,0.555265820743996,
0.641165742156689,0.555265820743996,0.641165742156689,0.555265820743996,
0.641165742156689,0.555265820743996,0.641165742156689,0.555265820743996,
0.641165742156689,0.555265820743996,0.641165742156689,0.555265820743996,
0.641165742156689,0.555265820743996,0.641165742156689,0.555265820743996,
0.641165742156689,0.555265820743996,0.641165742156689,0.555265820743996,
0.641165742156689,0.555265820743996,0.641165742156689,0.555265820743996,
0.641165742156689,0.555265820743996,0.641165742156689,0.555265820743996,
0.641165742156689,0.555265820743996,0.641165742156689,0.555265820743996,
0.641165742156689,0.555265820743996,0.641165742156689,0.555265820743996,
0.641165742156689,0.555265820743996,0.641165742156689,0.555265820743996,
0.641165742156689,0.555265820743996,0.641165742156689,0.555265820743996,
0.641165742156689,0.555265820743996,0.641165742156689,0.555265820743996,
0.641165742156689,0.555265820743996,0.641165742156689,0.555265820743996,
0.641165742156689,0.555265820743996,0.641165742156689,0.555265820743996,
0.641165742156689,0.555265820743996,0.641165742156689,0.555265820743996,
0.641165742156689,0.555265820743996,0.641165742156689,0.555265820743996,
0.641165742156689,0.555265820743996,0.641165742156689,0.555265820743996,
0.641165742156689,0.555265820743996,0.641165742156689,0.555265820743996,
0.641165742156689,0.555265820743996,0.641165742156689,0.555265820743996,
0.641165742156689,0.555265820743996,0.641165742156689,0.555265820743996,
0.641165742156689,0.555265820743996,0.641165742156689,0.555265820743996,
0.641165742156689,0.555265820743996,0.641165742156689,0.555265820743996,
0.641165742156689,0.555265820743996,0.641165742156689,0.555265820743996,
0.641165742156689,0.555265820743996,0.641165742156689,0.555265820743996,
0.641165742156689,0.555265820743996,0.641165742156689,0.555265820743996,
0.641165742156689,0.555265820743996,0.641165742156689,0.555265820743996,
0.641165742156689,0.555265820743996,0.641165742156689,0.555265820743996,
0.641165742156689,0.555265820743996,0.641165742156689,0.555265820743996,
0.641165742156689,0.555265820743996,0.641165742156689,0.555265820743996,
0.641165742156689,0.555265820743996,0.641165742156689,0.555265820743996,
0.641165742156689,0.555265820743996,0.641165742156689,0.555265820743996,
0.641165742156689,0.555265820743996,0.641165742156689,0.555265820743996,
0.641165742156689,0.555265820743996,0.641165742156689,0.555265820743996,
0.641165742156689,0.555265820743996,0.641165742156689,0.555265820743996,
0.641165742156689,0.555265820743996,0.641165742156689,0.555265820743996,
0.641165742156689,0.555265820743996,0.641165742156689,0.555265820743996,
0.641165742156689,0.555265820743996,0.641165742156689,0.555265820743996,
0.641165742156689,0.555265820743996,0.641165742156689,0.555265820743996,
0.641165742156689,0.555265820743996,0.641165742156689,0.555265820743996,
0.641165742156689,0.555265820743996,0.641165742156689,0.555265820743996,
0.641165742156689,0.555265820743996,0.641165742156689,0.555265820743996,
0.641165742156689,0.555265820743996,0.641165742156689,0.555265820743996,
0.641165742156689,0.555265820743996,0.641165742156689,0.555265820743996,
0.641165742156689,0.555265820743996,0.641165742156689,0.555265820743996,
0.641165742156689,0.555265820743996,0.641165742156689,0.555265820743996,
0.641165742156689,0.555265820743996,0.641165742156689,0.555265820743996,
0.641165742156689,0.555265820743996,0.641165742156689,0.555265820743996,
0.641165742156689,0.555265820743996,0.641165742156689,0.555265820743996,
0.641165742156689,0.555265820743996,0.641165742156689,0.555265820743996,
0.641165742156689,0.555265820743996,0.641165742156689,0.555265820743996,
0.641165742156689,0.555265820743996,0.641165742156689,0.555265820743996,
0.641165742156689,0.555265820743996,0.641165742156689,0.555265820743996,
0.641165742156689,0.555265820743996,0.641165742156689,0.555265820743996,
0.641165742156689,0.555265820743996,0.641165742156689,0.555265820743996,
0.641165742156689,0.555265820743996,0.641165742156689,0.555265820743996,
0.641165742156689,0.555265820743996,0.641165742156689,0.555265820743996,
0.641165742156689,0.555265820743996,0.641165742156689,0.555265820743996,
0.641165742156689,0.555265820743996,0.641165742156689,0.555265820743996,
0.641165742156689,0.555265820743996,0.641165742156689,0.555265820743996,
0.641165742156689,0.555265820743996,0.641165742156689,0.555265820743996,
0.641165742156689,0.555265820743996,0.641165742156689,0.555265820743996,
0.641165742156689,0.555265820743996,0.641165742156689,0.555265820743996,
0.641165742156689,0.555265820743996,0.641165742156689,0.555265820743996,
0.641165742156689,0.555265820743996,0.641165742156689,0.555265820743996,
0.641165742156689,0.555265820743996,0.641165742156689,0.555265820743996,
0.641165742156689,0.555265820743996,0.641165742156689,0.555265820743996,
0.641165742156689,0.555265820743996,0.641165742156689,0.555265820743996,
0.641165742156689,0.555265820743996,0.641165742156689,0.555265820743996,
0.641165742156689,0.555265820743996,0.641165742156689,0.555265820743996,
0.641165742156689,0.555265820743996,0.641165742156689,0.555265820743996,
0.641165742156689,0.555265820743996,0.641165742156689,0.555265820743996,
0.641165742156689,0.555265820743996,0.641165742156689,0.555265820743996,
0.641165742156689,0.555265820743996,0.641165742156689,0.555265820743996,
0.641165742156689,0.555265820743996,0.641165742156689,0.555265820743996,
0.641165742156689,0.555265820743996,0.641165742156689,0.555265820743996,
0.641165742156689,0.555265820743996,0.641165742156689,0.555265820743996,
0.641165742156689,0.555265820743996,0.641165742156689,0.555265820743996,
0.641165742156689,0.555265820743996,0.641165742156689,0.555265820743996,
0.641165742156689,0.555265820743996,0.641165742156689,0.555265820743996,
0.641165742156689,0.555265820743996,0.641165742156689,0.555265820743996,
0.641165742156689,0.555265820743996,0.641165742156689,0.555265820743996,
0.641165742156689,0.555265820743996,0.641165742156689,0.555265820743996,
0.641165742156689,0.555265820743996,0.641165742156689,0.555265820743996,
0.641165742156689,0.555265820743996,0.641165742156689,0.555265820743996,
0.641165742156689,0.555265820743996,0.641165742156689,0.555265820743996,
0.641165742156689,0.555265820743996,0.641165742156689,0.555265820743996,
0.641165742156689,0.555265820743996,0.641165742156689,0.555265820743996,
0.641165742156689,0.555265820743996,0.641165742156689,0.555265820743996,
0.641165742156689,0.555265820743996,0.641165742156689,0.555265820743996,
0.641165742156689,0.555265820743996,0.641165742156689,0.555265820743996,
0.641165742156689,0.555265820743996,0.641165742156689,0.555265820743996,
0.641165742156689,0.555265820743996,0.641165742156689,0.555265820743996,
0.641165742156689,0.555265820743996,0.641165742156689,0.555265820743996,
0.641165742156689,0.555265820743996,0.641165742156689,0.555265820743996,
0.641165742156689,0.555265820743996,0.641165742156689,0.555265820743996,
0.641165742156689,0.555265820743996,0.641165742156689,0.555265820743996,
0.641165742156689,0.555265820743996,0.641165742156689,0.555265820743996,
0.641165742156689,0.555265820743996,0.641165742156689,0.555265820743996,
0.641165742156689,0.555265820743996,0.641165742156689,0.555265820743996,
0.641165742156689,0.555265820743996,0.641165742156689,0.555265820743996,
0.641165742156689,0.555265820743996,0.641165742156689,0.555265820743996,
0.641165742156689,0.555265820743996,0.641165742156689,0.555265820743996,
0.641165742156689,0.555265820743996,0.641165742156689,0.555265820743996,
0.641165742156689,0.555265820743996,0.641165742156689,0.555265820743996,
0.641165742156689,0.555265820743996,0.641165742156689,0.555265820743996,
0.641165742156689,0.555265820743996,0.641165742156689,0.555265820743996,
0.641165742156689,0.555265820743996,0.641165742156689,0.555265820743996,
0.641165742156689,0.555265820743996,0.641165742156689,0.555265820743996,
0.641165742156689,0.555265820743996,0.641165742156689,0.555265820743996,
0.641165742156689,0.555265820743996,0.641165742156689,0.555265820743996,
0.641165742156689,0.555265820743996,0.641165742156689,0.555265820743996,
0.641165742156689,0.555265820743996,0.641165742156689,0.555265820743996,
0.641165742156689,0.555265820743996,0.641165742156689,0.555265820743996,
0.641165742156689,0.555265820743996,0.641165742156689,0.555265820743996,
0.641165742156689,0.555265820743996,0.641165742156689,0.555265820743996,
0.641165742156689,0.555265820743996,0.641165742156689,0.555265820743996,
0.641165742156689),(0.641165742156689,0.555265820743996,0.641165742156689,
0.555265820743996,0.641165742156689,0.555265820743996,0.641165742156689,
0.555265820743996,0.641165742156689,0.555265820743996,0.641165742156689,
0.555265820743996,0.641165742156689,0.555265820743996,0.641165742156689,
0.555265820743996,0.641165742156689,0.555265820743996,0.641165742156689,
0.555265820743996,0.641165742156689,0.555265820743996,0.641165742156689,
0.555265820743996,0.641165742156689,0.555265820743996,0.641165742156689,
0.555265820743996,0.641165742156689,0.555265820743996,0.641165742156689,
0.555265820743996,0.641165742156689,0.555265820743996,0.641165742156689,
0.555265820743996,0.641165742156689,0.555265820743996,0.641165742156689,
0.555265820743996,0.641165742156689,0.555265820743996,0.641165742156689,
0.555265820743996,0.641165742156689,0.555265820743996,0.641165742156689,
0.555265820743996,0.641165742156689,0.555265820743996,0.641165742156689,
0.555265820743996,0.641165742156689,0.555265820743996,0.641165742156689,
0.555265820743996,0.641165742156689,0.555265820743996,0.641165742156689,
0.555265820743996,0.641165742156689,0.555265820743996,0.641165742156689,
0.555265820743996,0.641165742156689,0.555265820743996,0.641165742156689,
0.555265820743996,0.641165742156689,0.555265820743996,0.641165742156689,
0.555265820743996,0.641165742156689,0.555265820743996,0.641165742156689,
0.555265820743996,0.641165742156689,0.555265820743996,0.641165742156689,
0.555265820743996,0.641165742156689,0.555265820743996,0.641165742156689,
0.555265820743996,0.641165742156689,0.555265820743996,0.641165742156689,
0.555265820743996,0.641165742156689,0.555265820743996,0.641165742156689,
0.555265820743996,0.641165742156689,0.555265820743996,0.641165742156689,
0.555265820743996,0.641165742156689,0.555265820743996,0.641165742156689,
0.555265820743996,0.641165742156689,0.555265820743996,0.641165742156689,
0.555265820743996,0.641165742156689,0.555265820743996,0.641165742156689,
0.555265820743996,0.641165742156689,0.555265820743996,0.641165742156689,
0.555265820743996,0.641165742156689,0.555265820743996,0.641165742156689,
0.555265820743996,0.641165742156689,0.555265820743996,0.641165742156689,
0.555265820743996,0.641165742156689,0.555265820743996,0.641165742156689,
0.555265820743996,0.641165742156689,0.555265820743996,0.641165742156689,
0.555265820743996,0.641165742156689,0.555265820743996,0.641165742156689,
0.555265820743996,0.641165742156689,0.555265820743996,0.641165742156689,
0.555265820743996,0.641165742156689,0.555265820743996,0.641165742156689,
0.555265820743996,0.641165742156689,0.555265820743996,0.641165742156689,
0.555265820743996,0.641165742156689,0.555265820743996,0.641165742156689,
0.555265820743996,0.641165742156689,0.555265820743996,0.641165742156689,
0.555265820743996,0.641165742156689,0.555265820743996,0.641165742156689,
0.555265820743996,0.641165742156689,0.555265820743996,0.641165742156689,
0.555265820743996,0.641165742156689,0.555265820743996,0.641165742156689,
0.555265820743996,0.641165742156689,0.555265820743996,0.641165742156689,
0.555265820743996,0.641165742156689,0.555265820743996,0.641165742156689,
0.555265820743996,0.641165742156689,0.555265820743996,0.641165742156689,
0.555265820743996,0.641165742156689,0.555265820743996,0.641165742156689,
0.555265820743996,0.641165742156689,0.555265820743996,0.641165742156689,
0.555265820743996,0.641165742156689,0.555265820743996,0.641165742156689,
0.555265820743996,0.641165742156689,0.555265820743996,0.641165742156689,
0.555265820743996,0.641165742156689,0.555265820743996,0.641165742156689,
0.555265820743996,0.641165742156689,0.555265820743996,0.641165742156689,
0.555265820743996,0.641165742156689,0.555265820743996,0.641165742156689,
0.555265820743996,0.641165742156689,0.555265820743996,0.641165742156689,
0.555265820743996,0.641165742156689,0.555265820743996,0.641165742156689,
0.555265820743996,0.641165742156689,0.555265820743996,0.641165742156689,
0.555265820743996,0.641165742156689,0.555265820743996,0.641165742156689,
0.555265820743996,0.641165742156689,0.555265820743996,0.641165742156689,
0.555265820743996,0.641165742156689,0.555265820743996,0.641165742156689,
0.555265820743996,0.641165742156689,0.555265820743996,0.641165742156689,
0.555265820743996,0.641165742156689,0.555265820743996,0.641165742156689,
0.555265820743996,0.641165742156689,0.555265820743996,0.641165742156689,
0.555265820743996,0.641165742156689,0.555265820743996,0.641165742156689,
0.555265820743996,0.641165742156689,0.555265820743996,0.641165742156689,
0.555265820743996,0.641165742156689,0.555265820743996,0.641165742156689,
0.555265820743996,0.641165742156689,0.555265820743996,0.641165742156689,
0.555265820743996,0.641165742156689,0.555265820743996,0.641165742156689,
0.555265820743996,0.641165742156689,0.555265820743996,0.641165742156689,
0.555265820743996,0.641165742156689,0.555265820743996,0.641165742156689,
0.555265820743996,0.641165742156689,0.555265820743996,0.641165742156689,
0.555265820743996,0.641165742156689,0.555265820743996,0.641165742156689,
0.555265820743996,0.641165742156689,0.555265820743996,0.641165742156689,
0.555265820743996,0.641165742156689,0.555265820743996,0.641165742156689,
0.555265820743996,0.641165742156689,0.555265820743996,0.641165742156689,
0.555265820743996,0.641165742156689,0.555265820743996,0.641165742156689,
0.555265820743996,0.641165742156689,0.555265820743996,0.641165742156689,
0.555265820743996,0.641165742156689,0.555265820743996,0.641165742156689,
0.555265820743996,0.641165742156689,0.555265820743996,0.641165742156689,
0.555265820743996,0.641165742156689,0.555265820743996,0.641165742156689,
0.555265820743996,0.641165742156689,0.555265820743996,0.641165742156689,
0.555265820743996,0.641165742156689,0.555265820743996,0.641165742156689,
0.555265820743996,0.641165742156689,0.555265820743996,0.641165742156689,
0.555265820743996,0.641165742156689,0.555265820743996,0.641165742156689,
0.555265820743996,0.641165742156689,0.555265820743996,0.641165742156689,
0.555265820743996,0.641165742156689,0.555265820743996,0.641165742156689,
0.555265820743996,0.641165742156689,0.555265820743996,0.641165742156689,
0.555265820743996,0.641165742156689,0.555265820743996,0.641165742156689,
0.555265820743996,0.641165742156689,0.555265820743996,0.641165742156689,
0.555265820743996,0.641165742156689,0.555265820743996,0.641165742156689,
0.555265820743996,0.641165742156689,0.555265820743996,0.641165742156689,
0.555265820743996,0.641165742156689,0.555265820743996,0.641165742156689,
0.555265820743996,0.641165742156689,0.555265820743996,0.641165742156689,
0.555265820743996,0.641165742156689,0.555265820743996,0.641165742156689,
0.555265820743996,0.641165742156689,0.555265820743996,0.641165742156689,
0.555265820743996,0.641165742156689,0.555265820743996,0.641165742156689,
0.555265820743996,0.641165742156689,0.555265820743996,0.641165742156689,
0.555265820743996,0.641165742156689,0.555265820743996,0.641165742156689,
0.555265820743996,0.641165742156689,0.555265820743996,0.641165742156689,
0.555265820743996,0.641165742156689,0.555265820743996,0.641165742156689,
0.555265820743996,0.641165742156689,0.555265820743996,0.641165742156689,
0.555265820743996,0.641165742156689,0.555265820743996,0.641165742156689,
0.555265820743996,0.641165742156689,0.555265820743996,0.641165742156689,
0.555265820743996,0.641165742156689,0.555265820743996,0.641165742156689,
0.555265820743996,0.641165742156689,0.555265820743996,0.641165742156689,
0.555265820743996,0.641165742156689,0.555265820743996,0.641165742156689,
0.555265820743996,0.641165742156689,0.555265820743996,0.641165742156689,
0.555265820743996,0.641165742156689,0.555265820743996,0.641165742156689,
0.555265820743996,0.641165742156689,0.555265820743996,0.641165742156689,
0.555265820743996,0.641165742156689,0.555265820743996,0.641165742156689,
0.555265820743996,0.641165742156689,0.555265820743996,0.641165742156689,
0.555265820743996,0.641165742156689,0.555265820743996,0.641165742156689,
0.555265820743996,0.641165742156689,0.555265820743996,0.641165742156689,
0.555265820743996,0.641165742156689,0.555265820743996,0.641165742156689,
0.555265820743996,0.641165742156689,0.555265820743996,0.641165742156689,
0.555265820743996,0.641165742156689,0.555265820743996,0.641165742156689,
0.555265820743996,0.641165742156689,0.555265820743996,0.641165742156689,
0.555265820743996,0.641165742156689,0.555265820743996,0.641165742156689,
0.555265820743996,0.641165742156689,0.555265820743996,0.641165742156689,
0.555265820743996,0.641165742156689,0.555265820743996,0.641165742156689,
0.555265820743996,0.641165742156689,0.555265820743996,0.641165742156689,
0.555265820743996,0.641165742156689,0.555265820743996,0.641165742156689,
0.555265820743996,0.641165742156689,0.555265820743996,0.641165742156689,
0.555265820743996,0.641165742156689,0.555265820743996,0.641165742156689,
0.555265820743996,0.641165742156689,0.555265820743996,0.641165742156689,
0.555265820743996,0.641165742156689,0.555265820743996,0.641165742156689,
0.555265820743996,0.641165742156689,0.555265820743996,0.641165742156689,
0.555265820743996,0.641165742156689,0.555265820743996,0.641165742156689,
0.555265820743996,0.641165742156689,0.555265820743996,0.641165742156689,
0.555265820743996,0.641165742156689,0.555265820743996,0.641165742156689,
0.555265820743996,0.641165742156689,0.555265820743996,0.641165742156689,
0.555265820743996,0.641165742156689,0.555265820743996,0.641165742156689,
0.555265820743996,0.641165742156689,0.555265820743996,0.641165742156689,
0.555265820743996,0.641165742156689,0.555265820743996,0.641165742156689,
0.555265820743996,0.641165742156689,0.555265820743996,0.641165742156689,
0.555265820743996,0.641165742156689,0.555265820743996,0.641165742156689,
0.555265820743996,0.641165742156689,0.555265820743996,0.641165742156689,
0.555265820743996,0.641165742156689,0.555265820743996,0.641165742156689,
0.555265820743996,0.641165742156689,0.555265820743996,0.641165742156689,
0.555265820743996,0.641165742156689,0.555265820743996,0.641165742156689,
0.555265820743996,0.641165742156689,0.555265820743996,0.641165742156689,
0.555265820743996,0.641165742156689,0.555265820743996,0.641165742156689,
0.555265820743996,0.641165742156689,0.555265820743996,0.641165742156689,
0.555265820743996,0.641165742156689,0.555265820743996,0.641165742156689,
0.555265820743996,0.641165742156689,0.555265820743996,0.641165742156689,
0.555265820743996,0.641165742156689,0.555265820743996,0.641165742156689,
0.555265820743996,0.641165742156689,0.555265820743996,0.641165742156689,
0.555265820743996,0.641165742156689,0.555265820743996,0.641165742156689,
0.555265820743996,0.641165742156689,0.555265820743996,0.641165742156689,
0.555265820743996,0.641165742156689,0.555265820743996,0.641165742156689,
0.555265820743996,0.641165742156689,0.555265820743996,0.641165742156689,
0.555265820743996,0.641165742156689,0.555265820743996,0.641165742156689,
0.555265820743996,0.641165742156689,0.555265820743996,0.641165742156689,
0.555265820743996,0.641165742156689,0.555265820743996,0.641165742156689,
0.555265820743996,0.641165742156689,0.555265820743996,0.641165742156689,
0.555265820743996,0.641165742156689,0.555265820743996,0.641165742156689,
0.555265820743996,0.641165742156689,0.555265820743996,0.641165742156689,
0.555265820743996,0.641165742156689,0.555265820743996,0.641165742156689,
0.555265820743996,0.641165742156689,0.555265820743996,0.641165742156689,
0.555265820743996,0.641165742156689,0.555265820743996,0.641165742156689,
0.555265820743996,0.641165742156689,0.555265820743996,0.641165742156689,
0.555265820743996,0.641165742156689,0.555265820743996,0.641165742156689,
0.555265820743996,0.641165742156689,0.555265820743996,0.641165742156689,
0.555265820743996,0.641165742156689,0.555265820743996,0.641165742156689,
0.555265820743996,0.641165742156689,0.555265820743996,0.641165742156689,
0.555265820743996,0.641165742156689,0.555265820743996,0.641165742156689,
0.555265820743996,0.641165742156689,0.555265820743996,0.641165742156689,
0.555265820743996,0.641165742156689,0.555265820743996,0.641165742156689,
0.555265820743996,0.641165742156689,0.555265820743996,0.641165742156689,
0.555265820743996,0.641165742156689,0.555265820743996,0.641165742156689,
0.555265820743996,0.641165742156689,0.555265820743996,0.641165742156689,
0.555265820743996,0.641165742156689,0.555265820743996,0.641165742156689,
0.555265820743996,0.641165742156689,0.555265820743996,0.641165742156689,
0.555265820743996,0.641165742156689,0.555265820743996,0.641165742156689,
0.555265820743996,0.641165742156689,0.555265820743996,0.641165742156689,
0.555265820743996,0.641165742156689,0.555265820743996,0.641165742156689,
0.555265820743996,0.641165742156689,0.555265820743996,0.641165742156689,
0.555265820743996,0.641165742156689,0.555265820743996,0.641165742156689,
0.555265820743996,0.641165742156689,0.555265820743996,0.641165742156689,
0.555265820743996,0.641165742156689,0.555265820743996,0.641165742156689,
0.555265820743996,0.641165742156689,0.555265820743996,0.641165742156689,
0.555265820743996,0.641165742156689,0.555265820743996,0.641165742156689,
0.555265820743996,0.641165742156689,0.555265820743996,0.641165742156689,
0.555265820743996,0.641165742156689,0.555265820743996,0.641165742156689,
0.555265820743996,0.641165742156689,0.555265820743996,0.641165742156689,
0.555265820743996,0.641165742156689,0.555265820743996,0.641165742156689,
0.555265820743996,0.641165742156689,0.555265820743996,0.641165742156689,
0.555265820743996,0.641165742156689,0.555265820743996,0.641165742156689,
0.555265820743996,0.641165742156689,0.555265820743996,0.641165742156689,
0.555265820743996,0.641165742156689,0.555265820743996,0.641165742156689,
0.555265820743996,0.641165742156689,0.555265820743996,0.641165742156689,
0.555265820743996,0.641165742156689,0.555265820743996,0.641165742156689,
0.555265820743996,0.641165742156689,0.555265820743996,0.641165742156689,
0.555265820743996,0.641165742156689,0.555265820743996,0.641165742156689,
0.555265820743996,0.641165742156689,0.555265820743996,0.641165742156689,
0.555265820743996,0.641165742156689,0.555265820743996,0.641165742156689,
0.555265820743996,0.641165742156689,0.555265820743996,0.641165742156689,
0.555265820743996,0.641165742156689,0.555265820743996,0.641165742156689,
0.555265820743996,0.641165742156689,0.555265820743996,0.641165742156689,
0.555265820743996,0.641165742156689,0.555265820743996,0.641165742156689,
0.555265820743996,0.641165742156689,0.555265820743996,0.641165742156689,
0.555265820743996,0.641165742156689,0.555265820743996,0.641165742156689,
0.555265820743996,0.641165742156689,0.555265820743996,0.641165742156689,
0.555265820743996,0.641165742156689,0.555265820743996,0.641165742156689,
0.555265820743996,0.641165742156689,0.555265820743996,0.641165742156689,
0.555265820743996,0.641165742156689,0.555265820743996,0.641165742156689,
0.555265820743996,0.641165742156689,0.555265820743996,0.641165742156689,
0.555265820743996,0.641165742156689,0.555265820743996,0.641165742156689,
0.555265820743996,0.641165742156689,0.555265820743996,0.641165742156689,
0.555265820743996,0.641165742156689,0.555265820743996,0.641165742156689,
0.555265820743996,0.641165742156689,0.555265820743996,0.641165742156689,
0.555265820743996,0.641165742156689,0.555265820743996,0.641165742156689,
0.555265820743996,0.641165742156689,0.555265820743996,0.641165742156689,
0.555265820743996,0.641165742156689,0.555265820743996,0.641165742156689,
0.555265820743996,0.641165742156689,0.555265820743996,0.641165742156689,
0.555265820743996,0.641165742156689,0.555265820743996,0.641165742156689,
0.555265820743996,0.641165742156689,0.555265820743996,0.641165742156689,
0.555265820743996,0.641165742156689,0.555265820743996,0.641165742156689,
0.555265820743996,0.641165742156689,0.555265820743996,0.641165742156689,
0.555265820743996,0.641165742156689,0.555265820743996,0.641165742156689,
0.555265820743996,0.641165742156689,0.555265820743996,0.641165742156689,
0.555265820743996,0.641165742156689,0.555265820743996,0.641165742156689,
0.555265820743996,0.641165742156689,0.555265820743996,0.641165742156689,
0.555265820743996,0.641165742156689,0.555265820743996,0.641165742156689,
0.555265820743996,0.641165742156689,0.555265820743996,0.641165742156689,
0.555265820743996,0.641165742156689,0.555265820743996,0.641165742156689,
0.555265820743996,0.641165742156689,0.555265820743996,0.641165742156689,
0.555265820743996,0.641165742156689,0.555265820743996,0.641165742156689,
0.555265820743996,0.641165742156689,0.555265820743996,0.641165742156689,
0.555265820743996,0.641165742156689,0.555265820743996,0.641165742156689,
0.555265820743996,0.641165742156689,0.555265820743996,0.641165742156689,
0.555265820743996,0.641165742156689,0.555265820743996,0.641165742156689,
0.555265820743996,0.641165742156689,0.555265820743996,0.641165742156689,
0.555265820743996,0.641165742156689,0.555265820743996,0.641165742156689,
0.555265820743996,0.641165742156689,0.555265820743996,0.641165742156689,
0.555265820743996,0.641165742156689,0.555265820743996,0.641165742156689,
0.555265820743996,0.641165742156689,0.555265820743996,0.641165742156689,
0.555265820743996,0.641165742156689,0.555265820743996,0.641165742156689,
0.555265820743996,0.641165742156689,0.555265820743996,0.641165742156689,
0.555265820743996,0.641165742156689,0.555265820743996,0.641165742156689,
0.555265820743996,0.641165742156689,0.555265820743996,0.641165742156689,
0.555265820743996,0.641165742156689,0.555265820743996,0.641165742156689,
0.555265820743996,0.641165742156689,0.555265820743996,0.641165742156689,
0.555265820743996,0.641165742156689,0.555265820743996,0.641165742156689,
0.555265820743996,0.641165742156689,0.555265820743996,0.641165742156689,
0.555265820743996,0.641165742156689,0.555265820743996,0.641165742156689,
0.555265820743996,0.641165742156689),(1.,0.866025403784439,1.,0.866025403784439,
1.,0.866025403784439,1.,0.866025403784439,1.,0.866025403784439,1.,0.866025403784439,
1.,0.866025403784439,1.,0.866025403784439,1.,0.866025403784439,1.,0.866025403784439,
1.,0.866025403784439,1.,0.866025403784439,1.,0.866025403784439,1.,0.866025403784439,
1.,0.866025403784439,1.,0.866025403784439,1.,0.866025403784439,1.,0.866025403784439,
1.,0.866025403784439,1.,0.866025403784439,1.,0.866025403784439,1.,0.866025403784439,
1.,0.866025403784439,1.,0.866025403784439,1.,0.866025403784439,1.,0.866025403784439,
1.,0.866025403784439,1.,0.866025403784439,1.,0.866025403784439,1.,0.866025403784439,
1.,0.866025403784439,1.,0.866025403784439,1.,0.866025403784439,1.,0.866025403784439,
1.,0.866025403784439,1.,0.866025403784439,1.,0.866025403784439,1.,0.866025403784439,
1.,0.866025403784439,1.,0.866025403784439,1.,0.866025403784439,1.,0.866025403784439,
1.,0.866025403784439,1.,0.866025403784439,1.,0.866025403784439,1.,0.866025403784439,
1.,0.866025403784439,1.,0.866025403784439,1.,0.866025403784439,1.,0.866025403784439,
1.,0.866025403784439,1.,0.866025403784439,1.,0.866025403784439,1.,0.866025403784439,
1.,0.866025403784439,1.,0.866025403784439,1.,0.866025403784439,1.,0.866025403784439,
1.,0.866025403784439,1.,0.866025403784439,1.,0.866025403784439,1.,0.866025403784439,
1.,0.866025403784439,1.,0.866025403784439,1.,0.866025403784439,1.,0.866025403784439,
1.,0.866025403784439,1.,0.866025403784439,1.,0.866025403784439,1.,0.866025403784439,
1.,0.866025403784439,1.,0.866025403784439,1.,0.866025403784439,1.,0.866025403784439,
1.,0.866025403784439,1.,0.866025403784439,1.,0.866025403784439,1.,0.866025403784439,
1.,0.866025403784439,1.,0.866025403784439,1.,0.866025403784439,1.,0.866025403784439,
1.,0.866025403784439,1.,0.866025403784439,1.,0.866025403784439,1.,0.866025403784439,
1.,0.866025403784439,1.,0.866025403784439,1.,0.866025403784439,1.,0.866025403784439,
1.,0.866025403784439,1.,0.866025403784439,1.,0.866025403784439,1.,0.866025403784439,
1.,0.866025403784439,1.,0.866025403784439,1.,0.866025403784439,1.,0.866025403784439,
1.,0.866025403784439,1.,0.866025403784439,1.,0.866025403784439,1.,0.866025403784439,
1.,0.866025403784439,1.,0.866025403784439,1.,0.866025403784439,1.,0.866025403784439,
1.,0.866025403784439,1.,0.866025403784439,1.,0.866025403784439,1.,0.866025403784439,
1.,0.866025403784439,1.,0.866025403784439,1.,0.866025403784439,1.,0.866025403784439,
1.,0.866025403784439,1.,0.866025403784439,1.,0.866025403784439,1.,0.866025403784439,
1.,0.866025403784439,1.,0.866025403784439,1.,0.866025403784439,1.,0.866025403784439,
1.,0.866025403784439,1.,0.866025403784439,1.,0.866025403784439,1.,0.866025403784439,
1.,0.866025403784439,1.,0.866025403784439,1.,0.866025403784439,1.,0.866025403784439,
1.,0.866025403784439,1.,0.866025403784439,1.,0.866025403784439,1.,0.866025403784439,
1.,0.866025403784439,1.,0.866025403784439,1.,0.866025403784439,1.,0.866025403784439,
1.,0.866025403784439,1.,0.866025403784439,1.,0.866025403784439,1.,0.866025403784439,
1.,0.866025403784439,1.,0.866025403784439,1.,0.866025403784439,1.,0.866025403784439,
1.,0.866025403784439,1.,0.866025403784439,1.,0.866025403784439,1.,0.866025403784439,
1.,0.866025403784439,1.,0.866025403784439,1.,0.866025403784439,1.,0.866025403784439,
1.,0.866025403784439,1.,0.866025403784439,1.,0.866025403784439,1.,0.866025403784439,
1.,0.866025403784439,1.,0.866025403784439,1.,0.866025403784439,1.,0.866025403784439,
1.,0.866025403784439,1.,0.866025403784439,1.,0.866025403784439,1.,0.866025403784439,
1.,0.866025403784439,1.,0.866025403784439,1.,0.866025403784439,1.,0.866025403784439,
1.,0.866025403784439,1.,0.866025403784439,1.,0.866025403784439,1.,0.866025403784439,
1.,0.866025403784439,1.,0.866025403784439,1.,0.866025403784439,1.,0.866025403784439,
1.,0.866025403784439,1.,0.866025403784439,1.,0.866025403784439,1.,0.866025403784439,
1.,0.866025403784439,1.,0.866025403784439,1.,0.866025403784439,1.,0.866025403784439,
1.,0.866025403784439,1.,0.866025403784439,1.,0.866025403784439,1.,0.866025403784439,
1.,0.866025403784439,1.,0.866025403784439,1.,0.866025403784439,1.,0.866025403784439,
1.,0.866025403784439,1.,0.866025403784439,1.,0.866025403784439,1.,0.866025403784439,
1.,0.866025403784439,1.,0.866025403784439,1.,0.866025403784439,1.,0.866025403784439,
1.,0.866025403784439,1.,0.866025403784439,1.,0.866025403784439,1.,0.866025403784439,
1.,0.866025403784439,1.,0.866025403784439,1.,0.866025403784439,1.,0.866025403784439,
1.,0.866025403784439,1.,0.866025403784439,1.,0.866025403784439,1.,0.866025403784439,
1.,0.866025403784439,1.,0.866025403784439,1.,0.866025403784439,1.,0.866025403784439,
1.,0.866025403784439,1.,0.866025403784439,1.,0.866025403784439,1.,0.866025403784439,
1.,0.866025403784439,1.,0.866025403784439,1.,0.866025403784439,1.,0.866025403784439,
1.,0.866025403784439,1.,0.866025403784439,1.,0.866025403784439,1.,0.866025403784439,
1.,0.866025403784439,1.,0.866025403784439,1.,0.866025403784439,1.,0.866025403784439,
1.,0.866025403784439,1.,0.866025403784439,1.,0.866025403784439,1.,0.866025403784439,
1.,0.866025403784439,1.,0.866025403784439,1.,0.866025403784439,1.,0.866025403784439,
1.,0.866025403784439,1.,0.866025403784439,1.,0.866025403784439,1.,0.866025403784439,
1.,0.866025403784439,1.,0.866025403784439,1.,0.866025403784439,1.,0.866025403784439,
1.,0.866025403784439,1.,0.866025403784439,1.,0.866025403784439,1.,0.866025403784439,
1.,0.866025403784439,1.,0.866025403784439,1.,0.866025403784439,1.,0.866025403784439,
1.,0.866025403784439,1.,0.866025403784439,1.,0.866025403784439,1.,0.866025403784439,
1.,0.866025403784439,1.,0.866025403784439,1.,0.866025403784439,1.,0.866025403784439,
1.,0.866025403784439,1.,0.866025403784439,1.,0.866025403784439,1.,0.866025403784439,
1.,0.866025403784439,1.,0.866025403784439,1.,0.866025403784439,1.,0.866025403784439,
1.,0.866025403784439,1.,0.866025403784439,1.,0.866025403784439,1.,0.866025403784439,
1.,0.866025403784439,1.,0.866025403784439,1.,0.866025403784439,1.,0.866025403784439,
1.,0.866025403784439,1.,0.866025403784439,1.,0.866025403784439,1.,0.866025403784439,
1.,0.866025403784439,1.,0.866025403784439,1.,0.866025403784439,1.,0.866025403784439,
1.,0.866025403784439,1.,0.866025403784439,1.,0.866025403784439,1.,0.866025403784439,
1.,0.866025403784439,1.,0.866025403784439,1.,0.866025403784439,1.,0.866025403784439,
1.,0.866025403784439,1.,0.866025403784439,1.,0.866025403784439,1.,0.866025403784439,
1.,0.866025403784439,1.,0.866025403784439,1.,0.866025403784439,1.,0.866025403784439,
1.,0.866025403784439,1.,0.866025403784439,1.,0.866025403784439,1.,0.866025403784439,
1.,0.866025403784439,1.,0.866025403784439,1.,0.866025403784439,1.,0.866025403784439,
1.,0.866025403784439,1.,0.866025403784439,1.,0.866025403784439,1.,0.866025403784439,
1.,0.866025403784439,1.,0.866025403784439,1.,0.866025403784439,1.,0.866025403784439,
1.,0.866025403784439,1.,0.866025403784439,1.,0.866025403784439,1.,0.866025403784439,
1.,0.866025403784439,1.,0.866025403784439,1.,0.866025403784439,1.,0.866025403784439,
1.,0.866025403784439,1.,0.866025403784439,1.,0.866025403784439,1.,0.866025403784439,
1.,0.866025403784439,1.,0.866025403784439,1.,0.866025403784439,1.,0.866025403784439,
1.,0.866025403784439,1.,0.866025403784439,1.,0.866025403784439,1.,0.866025403784439,
1.,0.866025403784439,1.,0.866025403784439,1.,0.866025403784439,1.,0.866025403784439,
1.,0.866025403784439,1.,0.866025403784439,1.,0.866025403784439,1.,0.866025403784439,
1.,0.866025403784439,1.,0.866025403784439,1.,0.866025403784439,1.,0.866025403784439,
1.,0.866025403784439,1.,0.866025403784439,1.,0.866025403784439,1.,0.866025403784439,
1.,0.866025403784439,1.,0.866025403784439,1.,0.866025403784439,1.,0.866025403784439,
1.,0.866025403784439,1.,0.866025403784439,1.,0.866025403784439,1.,0.866025403784439,
1.,0.866025403784439,1.,0.866025403784439,1.,0.866025403784439,1.,0.866025403784439,
1.,0.866025403784439,1.,0.866025403784439,1.,0.866025403784439,1.,0.866025403784439,
1.,0.866025403784439,1.,0.866025403784439,1.,0.866025403784439,1.,0.866025403784439,
1.,0.866025403784439,1.,0.866025403784439,1.,0.866025403784439,1.,0.866025403784439,
1.,0.866025403784439,1.,0.866025403784439,1.,0.866025403784439,1.,0.866025403784439,
1.,0.866025403784439,1.,0.866025403784439,1.,0.866025403784439,1.,0.866025403784439,
1.,0.866025403784439,1.,0.866025403784439,1.,0.866025403784439,1.,0.866025403784439,
1.,0.866025403784439,1.,0.866025403784439,1.,0.866025403784439,1.,0.866025403784439,
1.,0.866025403784439,1.,0.866025403784439,1.,0.866025403784439,1.,0.866025403784439,
1.,0.866025403784439,1.,0.866025403784439,1.,0.866025403784439,1.,0.866025403784439,
1.,0.866025403784439,1.,0.866025403784439,1.,0.866025403784439,1.,0.866025403784439,
1.,0.866025403784439,1.,0.866025403784439,1.,0.866025403784439,1.,0.866025403784439,
1.,0.866025403784439,1.,0.866025403784439,1.,0.866025403784439,1.,0.866025403784439,
1.,0.866025403784439,1.,0.866025403784439,1.,0.866025403784439,1.,0.866025403784439,
1.,0.866025403784439,1.,0.866025403784439,1.,0.866025403784439,1.,0.866025403784439,
1.,0.866025403784439,1.,0.866025403784439,1.,0.866025403784439,1.,0.866025403784439,
1.,0.866025403784439,1.,0.866025403784439,1.,0.866025403784439,1.,0.866025403784439,
1.,0.866025403784439,1.,0.866025403784439,1.,0.866025403784439,1.,0.866025403784439,
1.,0.866025403784439,1.,0.866025403784439,1.,0.866025403784439,1.,0.866025403784439,
1.,0.866025403784439,1.,0.866025403784439,1.,0.866025403784439,1.,0.866025403784439,
1.,0.866025403784439,1.,0.866025403784439,1.,0.866025403784439,1.,0.866025403784439,
1.,0.866025403784439,1.,0.866025403784439,1.,0.866025403784439,1.,0.866025403784439,
1.,0.866025403784439,1.,0.866025403784439,1.,0.866025403784439,1.,0.866025403784439,
1.,0.866025403784439,1.,0.866025403784439,1.,0.866025403784439,1.,0.866025403784439,
1.,0.866025403784439,1.,0.866025403784439,1.,0.866025403784439,1.,0.866025403784439,
1.,0.866025403784439,1.,0.866025403784439,1.,0.866025403784439,1.,0.866025403784439,
1.,0.866025403784439,1.,0.866025403784439,1.,0.866025403784439,1.,0.866025403784439,
1.,0.866025403784439,1.,0.866025403784439,1.,0.866025403784439,1.,0.866025403784439,
1.,0.866025403784439,1.,0.866025403784439,1.,0.866025403784439,1.,0.866025403784439,
1.,0.866025403784439,1.,0.866025403784439,1.,0.866025403784439,1.,0.866025403784439,
1.)))
REPRESENTATION_ITEM('')
SURFACE()
);
#180=(
BOUNDED_SURFACE()
B_SPLINE_SURFACE(1,2,((#37476,#37477,#37478,#37479,#37480,#37481,#37482,
#37483,#37484,#37485,#37486,#37487,#37488,#37489,#37490,#37491,#37492,#37493,
#37494,#37495,#37496,#37497,#37498,#37499,#37500,#37501,#37502,#37503,#37504,
#37505,#37506,#37507,#37508,#37509,#37510,#37511,#37512,#37513,#37514,#37515,
#37516,#37517,#37518,#37519,#37520,#37521,#37522,#37523,#37524,#37525,#37526,
#37527,#37528,#37529,#37530,#37531,#37532,#37533,#37534,#37535,#37536,#37537,
#37538,#37539,#37540,#37541,#37542,#37543,#37544,#37545,#37546,#37547,#37548,
#37549,#37550,#37551,#37552,#37553,#37554,#37555,#37556,#37557,#37558,#37559,
#37560,#37561,#37562,#37563,#37564,#37565,#37566,#37567,#37568,#37569,#37570,
#37571,#37572,#37573,#37574,#37575,#37576,#37577,#37578,#37579,#37580,#37581,
#37582,#37583,#37584,#37585,#37586,#37587,#37588,#37589,#37590,#37591,#37592,
#37593,#37594,#37595,#37596,#37597,#37598,#37599,#37600,#37601,#37602,#37603,
#37604,#37605,#37606,#37607,#37608,#37609,#37610,#37611,#37612,#37613,#37614,
#37615,#37616,#37617,#37618,#37619,#37620,#37621,#37622,#37623,#37624,#37625,
#37626,#37627,#37628,#37629,#37630,#37631,#37632,#37633,#37634,#37635,#37636,
#37637,#37638,#37639,#37640,#37641,#37642,#37643,#37644,#37645,#37646,#37647,
#37648,#37649,#37650,#37651,#37652,#37653,#37654,#37655,#37656,#37657,#37658,
#37659,#37660,#37661,#37662,#37663,#37664,#37665,#37666,#37667,#37668,#37669,
#37670,#37671,#37672,#37673,#37674,#37675,#37676,#37677,#37678,#37679,#37680,
#37681,#37682,#37683,#37684,#37685,#37686,#37687,#37688,#37689,#37690,#37691,
#37692,#37693,#37694,#37695,#37696,#37697,#37698,#37699,#37700,#37701,#37702,
#37703,#37704,#37705,#37706,#37707,#37708,#37709,#37710,#37711,#37712,#37713,
#37714,#37715,#37716,#37717,#37718,#37719,#37720,#37721,#37722,#37723,#37724,
#37725,#37726,#37727,#37728,#37729,#37730,#37731,#37732,#37733,#37734,#37735,
#37736,#37737,#37738,#37739,#37740,#37741,#37742,#37743,#37744,#37745,#37746,
#37747,#37748,#37749,#37750,#37751,#37752,#37753,#37754,#37755,#37756,#37757,
#37758,#37759,#37760,#37761,#37762,#37763,#37764,#37765,#37766,#37767,#37768,
#37769,#37770,#37771,#37772,#37773,#37774,#37775,#37776,#37777,#37778,#37779,
#37780,#37781,#37782,#37783,#37784,#37785,#37786,#37787,#37788,#37789,#37790,
#37791,#37792,#37793,#37794,#37795,#37796,#37797,#37798,#37799,#37800,#37801,
#37802,#37803,#37804,#37805,#37806,#37807,#37808,#37809,#37810,#37811,#37812,
#37813,#37814,#37815,#37816,#37817,#37818,#37819,#37820,#37821,#37822,#37823,
#37824,#37825,#37826,#37827,#37828,#37829,#37830,#37831,#37832,#37833,#37834,
#37835,#37836,#37837,#37838,#37839,#37840,#37841,#37842,#37843,#37844,#37845,
#37846,#37847,#37848,#37849,#37850,#37851,#37852,#37853,#37854,#37855,#37856,
#37857,#37858,#37859,#37860,#37861,#37862,#37863,#37864,#37865,#37866,#37867,
#37868,#37869,#37870,#37871,#37872,#37873,#37874,#37875,#37876,#37877,#37878,
#37879,#37880,#37881,#37882,#37883,#37884,#37885,#37886,#37887,#37888,#37889,
#37890,#37891,#37892,#37893,#37894,#37895,#37896,#37897,#37898,#37899,#37900,
#37901,#37902,#37903,#37904,#37905,#37906,#37907,#37908,#37909,#37910,#37911,
#37912,#37913,#37914,#37915,#37916,#37917,#37918,#37919,#37920,#37921,#37922,
#37923,#37924,#37925,#37926,#37927,#37928,#37929,#37930,#37931,#37932,#37933,
#37934,#37935,#37936,#37937,#37938,#37939,#37940,#37941,#37942,#37943,#37944,
#37945,#37946,#37947,#37948,#37949,#37950,#37951,#37952,#37953,#37954,#37955,
#37956,#37957,#37958,#37959,#37960,#37961,#37962,#37963,#37964,#37965,#37966,
#37967,#37968,#37969,#37970,#37971,#37972,#37973,#37974,#37975,#37976,#37977,
#37978,#37979,#37980,#37981,#37982,#37983,#37984,#37985,#37986,#37987,#37988,
#37989,#37990,#37991,#37992,#37993,#37994,#37995,#37996,#37997,#37998,#37999,
#38000,#38001,#38002,#38003,#38004,#38005,#38006,#38007,#38008,#38009,#38010,
#38011,#38012,#38013,#38014,#38015,#38016,#38017,#38018,#38019,#38020,#38021,
#38022,#38023,#38024,#38025,#38026,#38027,#38028,#38029,#38030,#38031,#38032,
#38033,#38034,#38035,#38036,#38037,#38038,#38039,#38040,#38041,#38042,#38043,
#38044,#38045,#38046,#38047,#38048,#38049,#38050,#38051,#38052,#38053,#38054,
#38055,#38056,#38057,#38058,#38059,#38060,#38061,#38062,#38063,#38064,#38065,
#38066,#38067,#38068,#38069,#38070,#38071,#38072,#38073,#38074,#38075,#38076,
#38077,#38078,#38079,#38080,#38081,#38082,#38083,#38084,#38085,#38086,#38087,
#38088,#38089,#38090,#38091,#38092,#38093,#38094,#38095,#38096,#38097,#38098,
#38099,#38100,#38101,#38102,#38103,#38104,#38105,#38106,#38107,#38108,#38109,
#38110,#38111,#38112,#38113,#38114,#38115,#38116,#38117,#38118,#38119,#38120,
#38121,#38122,#38123,#38124,#38125,#38126,#38127,#38128,#38129,#38130,#38131,
#38132,#38133,#38134,#38135,#38136,#38137,#38138,#38139,#38140,#38141,#38142,
#38143,#38144,#38145,#38146,#38147,#38148,#38149,#38150,#38151,#38152,#38153,
#38154,#38155,#38156,#38157,#38158,#38159,#38160,#38161,#38162,#38163,#38164,
#38165,#38166,#38167,#38168,#38169,#38170,#38171,#38172,#38173,#38174,#38175,
#38176,#38177,#38178,#38179,#38180,#38181,#38182,#38183,#38184,#38185,#38186,
#38187,#38188,#38189,#38190,#38191,#38192,#38193,#38194,#38195,#38196,#38197,
#38198,#38199,#38200,#38201,#38202,#38203,#38204,#38205,#38206,#38207,#38208,
#38209,#38210,#38211,#38212,#38213,#38214,#38215,#38216,#38217,#38218,#38219,
#38220,#38221,#38222,#38223,#38224,#38225,#38226,#38227,#38228,#38229,#38230,
#38231,#38232,#38233,#38234,#38235,#38236,#38237,#38238,#38239,#38240,#38241,
#38242,#38243,#38244,#38245,#38246,#38247,#38248,#38249,#38250,#38251,#38252,
#38253,#38254,#38255,#38256,#38257,#38258,#38259,#38260,#38261,#38262,#38263,
#38264,#38265,#38266,#38267,#38268,#38269,#38270,#38271,#38272,#38273,#38274,
#38275,#38276,#38277,#38278,#38279,#38280,#38281,#38282,#38283,#38284,#38285,
#38286,#38287,#38288,#38289,#38290,#38291,#38292,#38293,#38294,#38295,#38296,
#38297,#38298,#38299,#38300,#38301,#38302,#38303,#38304,#38305,#38306,#38307,
#38308,#38309,#38310,#38311,#38312,#38313,#38314,#38315,#38316,#38317,#38318,
#38319,#38320,#38321,#38322,#38323,#38324,#38325,#38326,#38327,#38328,#38329,
#38330,#38331,#38332,#38333,#38334,#38335,#38336,#38337,#38338,#38339,#38340,
#38341,#38342,#38343,#38344,#38345,#38346,#38347,#38348,#38349,#38350,#38351,
#38352,#38353,#38354,#38355,#38356,#38357,#38358,#38359,#38360,#38361,#38362,
#38363,#38364,#38365,#38366,#38367,#38368,#38369,#38370,#38371,#38372,#38373,
#38374,#38375,#38376,#38377,#38378,#38379,#38380,#38381,#38382,#38383,#38384,
#38385,#38386,#38387,#38388,#38389,#38390,#38391,#38392,#38393,#38394,#38395,
#38396,#38397,#38398,#38399,#38400,#38401,#38402,#38403,#38404,#38405,#38406,
#38407,#38408,#38409,#38410,#38411,#38412,#38413,#38414,#38415,#38416,#38417,
#38418,#38419,#38420,#38421,#38422,#38423,#38424,#38425,#38426,#38427,#38428,
#38429,#38430,#38431,#38432,#38433,#38434,#38435,#38436,#38437,#38438,#38439,
#38440,#38441,#38442,#38443,#38444,#38445,#38446,#38447,#38448),(#38449,
#38450,#38451,#38452,#38453,#38454,#38455,#38456,#38457,#38458,#38459,#38460,
#38461,#38462,#38463,#38464,#38465,#38466,#38467,#38468,#38469,#38470,#38471,
#38472,#38473,#38474,#38475,#38476,#38477,#38478,#38479,#38480,#38481,#38482,
#38483,#38484,#38485,#38486,#38487,#38488,#38489,#38490,#38491,#38492,#38493,
#38494,#38495,#38496,#38497,#38498,#38499,#38500,#38501,#38502,#38503,#38504,
#38505,#38506,#38507,#38508,#38509,#38510,#38511,#38512,#38513,#38514,#38515,
#38516,#38517,#38518,#38519,#38520,#38521,#38522,#38523,#38524,#38525,#38526,
#38527,#38528,#38529,#38530,#38531,#38532,#38533,#38534,#38535,#38536,#38537,
#38538,#38539,#38540,#38541,#38542,#38543,#38544,#38545,#38546,#38547,#38548,
#38549,#38550,#38551,#38552,#38553,#38554,#38555,#38556,#38557,#38558,#38559,
#38560,#38561,#38562,#38563,#38564,#38565,#38566,#38567,#38568,#38569,#38570,
#38571,#38572,#38573,#38574,#38575,#38576,#38577,#38578,#38579,#38580,#38581,
#38582,#38583,#38584,#38585,#38586,#38587,#38588,#38589,#38590,#38591,#38592,
#38593,#38594,#38595,#38596,#38597,#38598,#38599,#38600,#38601,#38602,#38603,
#38604,#38605,#38606,#38607,#38608,#38609,#38610,#38611,#38612,#38613,#38614,
#38615,#38616,#38617,#38618,#38619,#38620,#38621,#38622,#38623,#38624,#38625,
#38626,#38627,#38628,#38629,#38630,#38631,#38632,#38633,#38634,#38635,#38636,
#38637,#38638,#38639,#38640,#38641,#38642,#38643,#38644,#38645,#38646,#38647,
#38648,#38649,#38650,#38651,#38652,#38653,#38654,#38655,#38656,#38657,#38658,
#38659,#38660,#38661,#38662,#38663,#38664,#38665,#38666,#38667,#38668,#38669,
#38670,#38671,#38672,#38673,#38674,#38675,#38676,#38677,#38678,#38679,#38680,
#38681,#38682,#38683,#38684,#38685,#38686,#38687,#38688,#38689,#38690,#38691,
#38692,#38693,#38694,#38695,#38696,#38697,#38698,#38699,#38700,#38701,#38702,
#38703,#38704,#38705,#38706,#38707,#38708,#38709,#38710,#38711,#38712,#38713,
#38714,#38715,#38716,#38717,#38718,#38719,#38720,#38721,#38722,#38723,#38724,
#38725,#38726,#38727,#38728,#38729,#38730,#38731,#38732,#38733,#38734,#38735,
#38736,#38737,#38738,#38739,#38740,#38741,#38742,#38743,#38744,#38745,#38746,
#38747,#38748,#38749,#38750,#38751,#38752,#38753,#38754,#38755,#38756,#38757,
#38758,#38759,#38760,#38761,#38762,#38763,#38764,#38765,#38766,#38767,#38768,
#38769,#38770,#38771,#38772,#38773,#38774,#38775,#38776,#38777,#38778,#38779,
#38780,#38781,#38782,#38783,#38784,#38785,#38786,#38787,#38788,#38789,#38790,
#38791,#38792,#38793,#38794,#38795,#38796,#38797,#38798,#38799,#38800,#38801,
#38802,#38803,#38804,#38805,#38806,#38807,#38808,#38809,#38810,#38811,#38812,
#38813,#38814,#38815,#38816,#38817,#38818,#38819,#38820,#38821,#38822,#38823,
#38824,#38825,#38826,#38827,#38828,#38829,#38830,#38831,#38832,#38833,#38834,
#38835,#38836,#38837,#38838,#38839,#38840,#38841,#38842,#38843,#38844,#38845,
#38846,#38847,#38848,#38849,#38850,#38851,#38852,#38853,#38854,#38855,#38856,
#38857,#38858,#38859,#38860,#38861,#38862,#38863,#38864,#38865,#38866,#38867,
#38868,#38869,#38870,#38871,#38872,#38873,#38874,#38875,#38876,#38877,#38878,
#38879,#38880,#38881,#38882,#38883,#38884,#38885,#38886,#38887,#38888,#38889,
#38890,#38891,#38892,#38893,#38894,#38895,#38896,#38897,#38898,#38899,#38900,
#38901,#38902,#38903,#38904,#38905,#38906,#38907,#38908,#38909,#38910,#38911,
#38912,#38913,#38914,#38915,#38916,#38917,#38918,#38919,#38920,#38921,#38922,
#38923,#38924,#38925,#38926,#38927,#38928,#38929,#38930,#38931,#38932,#38933,
#38934,#38935,#38936,#38937,#38938,#38939,#38940,#38941,#38942,#38943,#38944,
#38945,#38946,#38947,#38948,#38949,#38950,#38951,#38952,#38953,#38954,#38955,
#38956,#38957,#38958,#38959,#38960,#38961,#38962,#38963,#38964,#38965,#38966,
#38967,#38968,#38969,#38970,#38971,#38972,#38973,#38974,#38975,#38976,#38977,
#38978,#38979,#38980,#38981,#38982,#38983,#38984,#38985,#38986,#38987,#38988,
#38989,#38990,#38991,#38992,#38993,#38994,#38995,#38996,#38997,#38998,#38999,
#39000,#39001,#39002,#39003,#39004,#39005,#39006,#39007,#39008,#39009,#39010,
#39011,#39012,#39013,#39014,#39015,#39016,#39017,#39018,#39019,#39020,#39021,
#39022,#39023,#39024,#39025,#39026,#39027,#39028,#39029,#39030,#39031,#39032,
#39033,#39034,#39035,#39036,#39037,#39038,#39039,#39040,#39041,#39042,#39043,
#39044,#39045,#39046,#39047,#39048,#39049,#39050,#39051,#39052,#39053,#39054,
#39055,#39056,#39057,#39058,#39059,#39060,#39061,#39062,#39063,#39064,#39065,
#39066,#39067,#39068,#39069,#39070,#39071,#39072,#39073,#39074,#39075,#39076,
#39077,#39078,#39079,#39080,#39081,#39082,#39083,#39084,#39085,#39086,#39087,
#39088,#39089,#39090,#39091,#39092,#39093,#39094,#39095,#39096,#39097,#39098,
#39099,#39100,#39101,#39102,#39103,#39104,#39105,#39106,#39107,#39108,#39109,
#39110,#39111,#39112,#39113,#39114,#39115,#39116,#39117,#39118,#39119,#39120,
#39121,#39122,#39123,#39124,#39125,#39126,#39127,#39128,#39129,#39130,#39131,
#39132,#39133,#39134,#39135,#39136,#39137,#39138,#39139,#39140,#39141,#39142,
#39143,#39144,#39145,#39146,#39147,#39148,#39149,#39150,#39151,#39152,#39153,
#39154,#39155,#39156,#39157,#39158,#39159,#39160,#39161,#39162,#39163,#39164,
#39165,#39166,#39167,#39168,#39169,#39170,#39171,#39172,#39173,#39174,#39175,
#39176,#39177,#39178,#39179,#39180,#39181,#39182,#39183,#39184,#39185,#39186,
#39187,#39188,#39189,#39190,#39191,#39192,#39193,#39194,#39195,#39196,#39197,
#39198,#39199,#39200,#39201,#39202,#39203,#39204,#39205,#39206,#39207,#39208,
#39209,#39210,#39211,#39212,#39213,#39214,#39215,#39216,#39217,#39218,#39219,
#39220,#39221,#39222,#39223,#39224,#39225,#39226,#39227,#39228,#39229,#39230,
#39231,#39232,#39233,#39234,#39235,#39236,#39237,#39238,#39239,#39240,#39241,
#39242,#39243,#39244,#39245,#39246,#39247,#39248,#39249,#39250,#39251,#39252,
#39253,#39254,#39255,#39256,#39257,#39258,#39259,#39260,#39261,#39262,#39263,
#39264,#39265,#39266,#39267,#39268,#39269,#39270,#39271,#39272,#39273,#39274,
#39275,#39276,#39277,#39278,#39279,#39280,#39281,#39282,#39283,#39284,#39285,
#39286,#39287,#39288,#39289,#39290,#39291,#39292,#39293,#39294,#39295,#39296,
#39297,#39298,#39299,#39300,#39301,#39302,#39303,#39304,#39305,#39306,#39307,
#39308,#39309,#39310,#39311,#39312,#39313,#39314,#39315,#39316,#39317,#39318,
#39319,#39320,#39321,#39322,#39323,#39324,#39325,#39326,#39327,#39328,#39329,
#39330,#39331,#39332,#39333,#39334,#39335,#39336,#39337,#39338,#39339,#39340,
#39341,#39342,#39343,#39344,#39345,#39346,#39347,#39348,#39349,#39350,#39351,
#39352,#39353,#39354,#39355,#39356,#39357,#39358,#39359,#39360,#39361,#39362,
#39363,#39364,#39365,#39366,#39367,#39368,#39369,#39370,#39371,#39372,#39373,
#39374,#39375,#39376,#39377,#39378,#39379,#39380,#39381,#39382,#39383,#39384,
#39385,#39386,#39387,#39388,#39389,#39390,#39391,#39392,#39393,#39394,#39395,
#39396,#39397,#39398,#39399,#39400,#39401,#39402,#39403,#39404,#39405,#39406,
#39407,#39408,#39409,#39410,#39411,#39412,#39413,#39414,#39415,#39416,#39417,
#39418,#39419,#39420,#39421)),.UNSPECIFIED.,.F.,.F.,.F.)
B_SPLINE_SURFACE_WITH_KNOTS((2,2),(3,2,2,2,2,2,2,2,2,2,2,2,2,2,2,2,2,2,
2,2,2,2,2,2,2,2,2,2,2,2,2,2,2,2,2,2,2,2,2,2,2,2,2,2,2,2,2,2,2,2,2,2,2,2,
2,2,2,2,2,2,2,2,2,2,2,2,2,2,2,2,2,2,2,2,2,2,2,2,2,2,2,2,2,2,2,2,2,2,2,2,
2,2,2,2,2,2,2,2,2,2,2,2,2,2,2,2,2,2,2,2,2,2,2,2,2,2,2,2,2,2,2,2,2,2,2,2,
2,2,2,2,2,2,2,2,2,2,2,2,2,2,2,2,2,2,2,2,2,2,2,2,2,2,2,2,2,2,2,2,2,2,2,2,
2,2,2,2,2,2,2,2,2,2,2,2,2,2,2,2,2,2,2,2,2,2,2,2,2,2,2,2,2,2,2,2,2,2,2,2,
2,2,2,2,2,2,2,2,2,2,2,2,2,2,2,2,2,2,2,2,2,2,2,2,2,2,2,2,2,2,2,2,2,2,2,2,
2,2,2,2,2,2,2,2,2,2,2,2,2,2,2,2,2,2,2,2,2,2,2,2,2,2,2,2,2,2,2,2,2,2,2,2,
2,2,2,2,2,2,2,2,2,2,2,2,2,2,2,2,2,2,2,2,2,2,2,2,2,2,2,2,2,2,2,2,2,2,2,2,
2,2,2,2,2,2,2,2,2,2,2,2,2,2,2,2,2,2,2,2,2,2,2,2,2,2,2,2,2,2,2,2,2,2,2,2,
2,2,2,2,2,2,2,2,2,2,2,2,2,2,2,2,2,2,2,2,2,2,2,2,2,2,2,2,2,2,2,2,2,2,2,2,
2,2,2,2,2,2,2,2,2,2,2,2,2,2,2,2,2,2,2,2,2,2,2,2,2,2,2,2,2,2,2,2,2,2,2,2,
2,2,2,2,2,2,2,2,2,2,2,2,2,2,2,2,2,2,2,2,2,2,2,2,2,2,2,2,2,2,2,2,2,2,2,2,
2,2,2,2,2,2,2,2,2,2,2,2,2,2,2,2,2,2,2,2,2,2,2,2,2,2,2,2,2,2,2,2,2,2,2,2,
3),(0.,1.),(0.,0.00205761316872428,0.00411522633744856,0.00617283950617284,
0.00823045267489712,0.0102880658436214,0.0123456790123457,0.01440329218107,
0.0164609053497942,0.0185185185185185,0.0205761316872428,0.0226337448559671,
0.0246913580246914,0.0267489711934156,0.0288065843621399,0.0308641975308642,
0.0329218106995885,0.0349794238683128,0.037037037037037,0.0390946502057613,
0.0411522633744856,0.0432098765432099,0.0452674897119342,0.0473251028806584,
0.0493827160493827,0.051440329218107,0.0534979423868313,0.0555555555555556,
0.0576131687242798,0.0596707818930041,0.0617283950617284,0.0637860082304527,
0.065843621399177,0.0679012345679012,0.0699588477366255,0.0720164609053498,
0.0740740740740741,0.0761316872427984,0.0781893004115226,0.0802469135802469,
0.0823045267489712,0.0843621399176955,0.0864197530864197,0.088477366255144,
0.0905349794238683,0.0925925925925926,0.0946502057613169,0.0967078189300412,
0.0987654320987654,0.10082304526749,0.102880658436214,0.104938271604938,
0.106995884773663,0.109053497942387,0.111111111111111,0.113168724279835,
0.11522633744856,0.117283950617284,0.119341563786008,0.121399176954733,
0.123456790123457,0.125514403292181,0.127572016460905,0.12962962962963,
0.131687242798354,0.133744855967078,0.135802469135802,0.137860082304527,
0.139917695473251,0.141975308641975,0.1440329218107,0.146090534979424,0.148148148148148,
0.150205761316872,0.152263374485597,0.154320987654321,0.156378600823045,
0.15843621399177,0.160493827160494,0.162551440329218,0.164609053497942,
0.166666666666667,0.168724279835391,0.170781893004115,0.172839506172839,
0.174897119341564,0.176954732510288,0.179012345679012,0.181069958847737,
0.183127572016461,0.185185185185185,0.187242798353909,0.189300411522634,
0.191358024691358,0.193415637860082,0.195473251028807,0.197530864197531,
0.199588477366255,0.201646090534979,0.203703703703704,0.205761316872428,
0.207818930041152,0.209876543209877,0.211934156378601,0.213991769547325,
0.216049382716049,0.218106995884774,0.220164609053498,0.222222222222222,
0.224279835390947,0.226337448559671,0.228395061728395,0.230452674897119,
0.232510288065844,0.234567901234568,0.236625514403292,0.238683127572016,
0.240740740740741,0.242798353909465,0.244855967078189,0.246913580246914,
0.248971193415638,0.251028806584362,0.253086419753086,0.255144032921811,
0.257201646090535,0.259259259259259,0.261316872427984,0.263374485596708,
0.265432098765432,0.267489711934156,0.269547325102881,0.271604938271605,
0.273662551440329,0.275720164609054,0.277777777777778,0.279835390946502,
0.281893004115226,0.283950617283951,0.286008230452675,0.288065843621399,
0.290123456790123,0.292181069958848,0.294238683127572,0.296296296296296,
0.298353909465021,0.300411522633745,0.302469135802469,0.304526748971193,
0.306584362139918,0.308641975308642,0.310699588477366,0.312757201646091,
0.314814814814815,0.316872427983539,0.318930041152263,0.320987654320988,
0.323045267489712,0.325102880658436,0.327160493827161,0.329218106995885,
0.331275720164609,0.333333333333333,0.335390946502058,0.337448559670782,
0.339506172839506,0.34156378600823,0.343621399176955,0.345679012345679,
0.347736625514403,0.349794238683128,0.351851851851852,0.353909465020576,
0.3559670781893,0.358024691358025,0.360082304526749,0.362139917695473,0.364197530864198,
0.366255144032922,0.368312757201646,0.37037037037037,0.372427983539095,
0.374485596707819,0.376543209876543,0.378600823045267,0.380658436213992,
0.382716049382716,0.38477366255144,0.386831275720165,0.388888888888889,
0.390946502057613,0.393004115226337,0.395061728395062,0.397119341563786,
0.39917695473251,0.401234567901235,0.403292181069959,0.405349794238683,
0.407407407407407,0.409465020576132,0.411522633744856,0.41358024691358,
0.415637860082305,0.417695473251029,0.419753086419753,0.421810699588477,
0.423868312757202,0.425925925925926,0.42798353909465,0.430041152263374,
0.432098765432099,0.434156378600823,0.436213991769547,0.438271604938272,
0.440329218106996,0.44238683127572,0.444444444444444,0.446502057613169,
0.448559670781893,0.450617283950617,0.452674897119342,0.454732510288066,
0.45679012345679,0.458847736625514,0.460905349794239,0.462962962962963,
0.465020576131687,0.467078189300412,0.469135802469136,0.47119341563786,
0.473251028806584,0.475308641975309,0.477366255144033,0.479423868312757,
0.481481481481481,0.483539094650206,0.48559670781893,0.487654320987654,
0.489711934156379,0.491769547325103,0.493827160493827,0.495884773662551,
0.497942386831276,0.5,0.502057613168724,0.504115226337449,0.506172839506173,
0.508230452674897,0.510288065843621,0.512345679012346,0.51440329218107,
0.516460905349794,0.518518518518518,0.520576131687243,0.522633744855967,
0.524691358024691,0.526748971193416,0.52880658436214,0.530864197530864,
0.532921810699588,0.534979423868313,0.537037037037037,0.539094650205761,
0.541152263374486,0.54320987654321,0.545267489711934,0.547325102880658,
0.549382716049383,0.551440329218107,0.553497942386831,0.555555555555556,
0.55761316872428,0.559670781893004,0.561728395061728,0.563786008230453,
0.565843621399177,0.567901234567901,0.569958847736626,0.57201646090535,
0.574074074074074,0.576131687242798,0.578189300411523,0.580246913580247,
0.582304526748971,0.584362139917695,0.58641975308642,0.588477366255144,
0.590534979423868,0.592592592592593,0.594650205761317,0.596707818930041,
0.598765432098765,0.60082304526749,0.602880658436214,0.604938271604938,
0.606995884773663,0.609053497942387,0.611111111111111,0.613168724279835,
0.61522633744856,0.617283950617284,0.619341563786008,0.621399176954732,
0.623456790123457,0.625514403292181,0.627572016460905,0.62962962962963,
0.631687242798354,0.633744855967078,0.635802469135803,0.637860082304527,
0.639917695473251,0.641975308641975,0.6440329218107,0.646090534979424,0.648148148148148,
0.650205761316872,0.652263374485597,0.654320987654321,0.656378600823045,
0.65843621399177,0.660493827160494,0.662551440329218,0.664609053497942,
0.666666666666667,0.668724279835391,0.670781893004115,0.672839506172839,
0.674897119341564,0.676954732510288,0.679012345679012,0.681069958847737,
0.683127572016461,0.685185185185185,0.687242798353909,0.689300411522634,
0.691358024691358,0.693415637860082,0.695473251028807,0.697530864197531,
0.699588477366255,0.701646090534979,0.703703703703704,0.705761316872428,
0.707818930041152,0.709876543209877,0.711934156378601,0.713991769547325,
0.716049382716049,0.718106995884774,0.720164609053498,0.722222222222222,
0.724279835390947,0.726337448559671,0.728395061728395,0.730452674897119,
0.732510288065844,0.734567901234568,0.736625514403292,0.738683127572016,
0.740740740740741,0.742798353909465,0.744855967078189,0.746913580246914,
0.748971193415638,0.751028806584362,0.753086419753086,0.755144032921811,
0.757201646090535,0.759259259259259,0.761316872427984,0.763374485596708,
0.765432098765432,0.767489711934156,0.769547325102881,0.771604938271605,
0.773662551440329,0.775720164609053,0.777777777777778,0.779835390946502,
0.781893004115226,0.783950617283951,0.786008230452675,0.788065843621399,
0.790123456790123,0.792181069958848,0.794238683127572,0.796296296296296,
0.798353909465021,0.800411522633745,0.802469135802469,0.804526748971193,
0.806584362139918,0.808641975308642,0.810699588477366,0.812757201646091,
0.814814814814815,0.816872427983539,0.818930041152263,0.820987654320988,
0.823045267489712,0.825102880658436,0.827160493827161,0.829218106995885,
0.831275720164609,0.833333333333333,0.835390946502058,0.837448559670782,
0.839506172839506,0.84156378600823,0.843621399176955,0.845679012345679,
0.847736625514403,0.849794238683128,0.851851851851852,0.853909465020576,
0.8559670781893,0.858024691358025,0.860082304526749,0.862139917695473,0.864197530864197,
0.866255144032922,0.868312757201646,0.87037037037037,0.872427983539095,
0.874485596707819,0.876543209876543,0.878600823045268,0.880658436213992,
0.882716049382716,0.88477366255144,0.886831275720165,0.888888888888889,
0.890946502057613,0.893004115226337,0.895061728395062,0.897119341563786,
0.89917695473251,0.901234567901235,0.903292181069959,0.905349794238683,
0.907407407407407,0.909465020576132,0.911522633744856,0.91358024691358,
0.915637860082305,0.917695473251029,0.919753086419753,0.921810699588477,
0.923868312757202,0.925925925925926,0.92798353909465,0.930041152263374,
0.932098765432099,0.934156378600823,0.936213991769547,0.938271604938272,
0.940329218106996,0.94238683127572,0.944444444444444,0.946502057613169,
0.948559670781893,0.950617283950617,0.952674897119342,0.954732510288066,
0.95679012345679,0.958847736625514,0.960905349794239,0.962962962962963,
0.965020576131687,0.967078189300412,0.969135802469136,0.97119341563786,
0.973251028806584,0.975308641975309,0.977366255144033,0.979423868312757,
0.981481481481482,0.983539094650206,0.98559670781893,0.987654320987654,
0.989711934156379,0.991769547325103,0.993827160493827,0.995884773662551,
0.997942386831276,1.),.UNSPECIFIED.)
GEOMETRIC_REPRESENTATION_ITEM()
RATIONAL_B_SPLINE_SURFACE(((1.,0.866025403784439,1.,0.866025403784439,1.,
0.866025403784439,1.,0.866025403784439,1.,0.866025403784439,1.,0.866025403784439,
1.,0.866025403784439,1.,0.866025403784439,1.,0.866025403784439,1.,0.866025403784439,
1.,0.866025403784439,1.,0.866025403784439,1.,0.866025403784439,1.,0.866025403784439,
1.,0.866025403784439,1.,0.866025403784439,1.,0.866025403784439,1.,0.866025403784439,
1.,0.866025403784439,1.,0.866025403784439,1.,0.866025403784439,1.,0.866025403784439,
1.,0.866025403784439,1.,0.866025403784439,1.,0.866025403784439,1.,0.866025403784439,
1.,0.866025403784439,1.,0.866025403784439,1.,0.866025403784439,1.,0.866025403784439,
1.,0.866025403784439,1.,0.866025403784439,1.,0.866025403784439,1.,0.866025403784439,
1.,0.866025403784439,1.,0.866025403784439,1.,0.866025403784439,1.,0.866025403784439,
1.,0.866025403784439,1.,0.866025403784439,1.,0.866025403784439,1.,0.866025403784439,
1.,0.866025403784439,1.,0.866025403784439,1.,0.866025403784439,1.,0.866025403784439,
1.,0.866025403784439,1.,0.866025403784439,1.,0.866025403784439,1.,0.866025403784439,
1.,0.866025403784439,1.,0.866025403784439,1.,0.866025403784439,1.,0.866025403784439,
1.,0.866025403784439,1.,0.866025403784439,1.,0.866025403784439,1.,0.866025403784439,
1.,0.866025403784439,1.,0.866025403784439,1.,0.866025403784439,1.,0.866025403784439,
1.,0.866025403784439,1.,0.866025403784439,1.,0.866025403784439,1.,0.866025403784439,
1.,0.866025403784439,1.,0.866025403784439,1.,0.866025403784439,1.,0.866025403784439,
1.,0.866025403784439,1.,0.866025403784439,1.,0.866025403784439,1.,0.866025403784439,
1.,0.866025403784439,1.,0.866025403784439,1.,0.866025403784439,1.,0.866025403784439,
1.,0.866025403784439,1.,0.866025403784439,1.,0.866025403784439,1.,0.866025403784439,
1.,0.866025403784439,1.,0.866025403784439,1.,0.866025403784439,1.,0.866025403784439,
1.,0.866025403784439,1.,0.866025403784439,1.,0.866025403784439,1.,0.866025403784439,
1.,0.866025403784439,1.,0.866025403784439,1.,0.866025403784439,1.,0.866025403784439,
1.,0.866025403784439,1.,0.866025403784439,1.,0.866025403784439,1.,0.866025403784439,
1.,0.866025403784439,1.,0.866025403784439,1.,0.866025403784439,1.,0.866025403784439,
1.,0.866025403784439,1.,0.866025403784439,1.,0.866025403784439,1.,0.866025403784439,
1.,0.866025403784439,1.,0.866025403784439,1.,0.866025403784439,1.,0.866025403784439,
1.,0.866025403784439,1.,0.866025403784439,1.,0.866025403784439,1.,0.866025403784439,
1.,0.866025403784439,1.,0.866025403784439,1.,0.866025403784439,1.,0.866025403784439,
1.,0.866025403784439,1.,0.866025403784439,1.,0.866025403784439,1.,0.866025403784439,
1.,0.866025403784439,1.,0.866025403784439,1.,0.866025403784439,1.,0.866025403784439,
1.,0.866025403784439,1.,0.866025403784439,1.,0.866025403784439,1.,0.866025403784439,
1.,0.866025403784439,1.,0.866025403784439,1.,0.866025403784439,1.,0.866025403784439,
1.,0.866025403784439,1.,0.866025403784439,1.,0.866025403784439,1.,0.866025403784439,
1.,0.866025403784439,1.,0.866025403784439,1.,0.866025403784439,1.,0.866025403784439,
1.,0.866025403784439,1.,0.866025403784439,1.,0.866025403784439,1.,0.866025403784439,
1.,0.866025403784439,1.,0.866025403784439,1.,0.866025403784439,1.,0.866025403784439,
1.,0.866025403784439,1.,0.866025403784439,1.,0.866025403784439,1.,0.866025403784439,
1.,0.866025403784439,1.,0.866025403784439,1.,0.866025403784439,1.,0.866025403784439,
1.,0.866025403784439,1.,0.866025403784439,1.,0.866025403784439,1.,0.866025403784439,
1.,0.866025403784439,1.,0.866025403784439,1.,0.866025403784439,1.,0.866025403784439,
1.,0.866025403784439,1.,0.866025403784439,1.,0.866025403784439,1.,0.866025403784439,
1.,0.866025403784439,1.,0.866025403784439,1.,0.866025403784439,1.,0.866025403784439,
1.,0.866025403784439,1.,0.866025403784439,1.,0.866025403784439,1.,0.866025403784439,
1.,0.866025403784439,1.,0.866025403784439,1.,0.866025403784439,1.,0.866025403784439,
1.,0.866025403784439,1.,0.866025403784439,1.,0.866025403784439,1.,0.866025403784439,
1.,0.866025403784439,1.,0.866025403784439,1.,0.866025403784439,1.,0.866025403784439,
1.,0.866025403784439,1.,0.866025403784439,1.,0.866025403784439,1.,0.866025403784439,
1.,0.866025403784439,1.,0.866025403784439,1.,0.866025403784439,1.,0.866025403784439,
1.,0.866025403784439,1.,0.866025403784439,1.,0.866025403784439,1.,0.866025403784439,
1.,0.866025403784439,1.,0.866025403784439,1.,0.866025403784439,1.,0.866025403784439,
1.,0.866025403784439,1.,0.866025403784439,1.,0.866025403784439,1.,0.866025403784439,
1.,0.866025403784439,1.,0.866025403784439,1.,0.866025403784439,1.,0.866025403784439,
1.,0.866025403784439,1.,0.866025403784439,1.,0.866025403784439,1.,0.866025403784439,
1.,0.866025403784439,1.,0.866025403784439,1.,0.866025403784439,1.,0.866025403784439,
1.,0.866025403784439,1.,0.866025403784439,1.,0.866025403784439,1.,0.866025403784439,
1.,0.866025403784439,1.,0.866025403784439,1.,0.866025403784439,1.,0.866025403784439,
1.,0.866025403784439,1.,0.866025403784439,1.,0.866025403784439,1.,0.866025403784439,
1.,0.866025403784439,1.,0.866025403784439,1.,0.866025403784439,1.,0.866025403784439,
1.,0.866025403784439,1.,0.866025403784439,1.,0.866025403784439,1.,0.866025403784439,
1.,0.866025403784439,1.,0.866025403784439,1.,0.866025403784439,1.,0.866025403784439,
1.,0.866025403784439,1.,0.866025403784439,1.,0.866025403784439,1.,0.866025403784439,
1.,0.866025403784439,1.,0.866025403784439,1.,0.866025403784439,1.,0.866025403784439,
1.,0.866025403784439,1.,0.866025403784439,1.,0.866025403784439,1.,0.866025403784439,
1.,0.866025403784439,1.,0.866025403784439,1.,0.866025403784439,1.,0.866025403784439,
1.,0.866025403784439,1.,0.866025403784439,1.,0.866025403784439,1.,0.866025403784439,
1.,0.866025403784439,1.,0.866025403784439,1.,0.866025403784439,1.,0.866025403784439,
1.,0.866025403784439,1.,0.866025403784439,1.,0.866025403784439,1.,0.866025403784439,
1.,0.866025403784439,1.,0.866025403784439,1.,0.866025403784439,1.,0.866025403784439,
1.,0.866025403784439,1.,0.866025403784439,1.,0.866025403784439,1.,0.866025403784439,
1.,0.866025403784439,1.,0.866025403784439,1.,0.866025403784439,1.,0.866025403784439,
1.,0.866025403784439,1.,0.866025403784439,1.,0.866025403784439,1.,0.866025403784439,
1.,0.866025403784439,1.,0.866025403784439,1.,0.866025403784439,1.,0.866025403784439,
1.,0.866025403784439,1.,0.866025403784439,1.,0.866025403784439,1.,0.866025403784439,
1.,0.866025403784439,1.,0.866025403784439,1.,0.866025403784439,1.,0.866025403784439,
1.,0.866025403784439,1.,0.866025403784439,1.,0.866025403784439,1.,0.866025403784439,
1.,0.866025403784439,1.,0.866025403784439,1.,0.866025403784439,1.,0.866025403784439,
1.,0.866025403784439,1.,0.866025403784439,1.,0.866025403784439,1.,0.866025403784439,
1.,0.866025403784439,1.,0.866025403784439,1.,0.866025403784439,1.,0.866025403784439,
1.,0.866025403784439,1.,0.866025403784439,1.,0.866025403784439,1.,0.866025403784439,
1.,0.866025403784439,1.,0.866025403784439,1.,0.866025403784439,1.,0.866025403784439,
1.,0.866025403784439,1.,0.866025403784439,1.,0.866025403784439,1.,0.866025403784439,
1.,0.866025403784439,1.,0.866025403784439,1.,0.866025403784439,1.,0.866025403784439,
1.,0.866025403784439,1.,0.866025403784439,1.,0.866025403784439,1.,0.866025403784439,
1.,0.866025403784439,1.,0.866025403784439,1.,0.866025403784439,1.,0.866025403784439,
1.,0.866025403784439,1.,0.866025403784439,1.,0.866025403784439,1.,0.866025403784439,
1.,0.866025403784439,1.,0.866025403784439,1.,0.866025403784439,1.,0.866025403784439,
1.,0.866025403784439,1.,0.866025403784439,1.,0.866025403784439,1.,0.866025403784439,
1.,0.866025403784439,1.,0.866025403784439,1.,0.866025403784439,1.,0.866025403784439,
1.,0.866025403784439,1.,0.866025403784439,1.,0.866025403784439,1.,0.866025403784439,
1.,0.866025403784439,1.,0.866025403784439,1.,0.866025403784439,1.,0.866025403784439,
1.,0.866025403784439,1.,0.866025403784439,1.,0.866025403784439,1.,0.866025403784439,
1.,0.866025403784439,1.,0.866025403784439,1.,0.866025403784439,1.,0.866025403784439,
1.,0.866025403784439,1.,0.866025403784439,1.,0.866025403784439,1.,0.866025403784439,
1.,0.866025403784439,1.,0.866025403784439,1.,0.866025403784439,1.,0.866025403784439,
1.,0.866025403784439,1.,0.866025403784439,1.,0.866025403784439,1.,0.866025403784439,
1.,0.866025403784439,1.,0.866025403784439,1.,0.866025403784439,1.,0.866025403784439,
1.,0.866025403784439,1.,0.866025403784439,1.,0.866025403784439,1.,0.866025403784439,
1.,0.866025403784439,1.,0.866025403784439,1.,0.866025403784439,1.,0.866025403784439,
1.,0.866025403784439,1.,0.866025403784439,1.,0.866025403784439,1.,0.866025403784439,
1.,0.866025403784439,1.,0.866025403784439,1.,0.866025403784439,1.,0.866025403784439,
1.,0.866025403784439,1.,0.866025403784439,1.,0.866025403784439,1.,0.866025403784439,
1.,0.866025403784439,1.,0.866025403784439,1.,0.866025403784439,1.,0.866025403784439,
1.,0.866025403784439,1.,0.866025403784439,1.,0.866025403784439,1.,0.866025403784439,
1.,0.866025403784439,1.,0.866025403784439,1.,0.866025403784439,1.,0.866025403784439,
1.,0.866025403784439,1.,0.866025403784439,1.,0.866025403784439,1.,0.866025403784439,
1.,0.866025403784439,1.,0.866025403784439,1.,0.866025403784439,1.,0.866025403784439,
1.,0.866025403784439,1.,0.866025403784439,1.,0.866025403784439,1.,0.866025403784439,
1.,0.866025403784439,1.,0.866025403784439,1.,0.866025403784439,1.,0.866025403784439,
1.,0.866025403784439,1.,0.866025403784439,1.,0.866025403784439,1.,0.866025403784439,
1.,0.866025403784439,1.,0.866025403784439,1.,0.866025403784439,1.,0.866025403784439,
1.,0.866025403784439,1.,0.866025403784439,1.,0.866025403784439,1.,0.866025403784439,
1.,0.866025403784439,1.,0.866025403784439,1.,0.866025403784439,1.,0.866025403784439,
1.,0.866025403784439,1.,0.866025403784439,1.,0.866025403784439,1.,0.866025403784439,
1.,0.866025403784439,1.,0.866025403784439,1.,0.866025403784439,1.,0.866025403784439,
1.,0.866025403784439,1.,0.866025403784439,1.,0.866025403784439,1.,0.866025403784439,
1.,0.866025403784439,1.,0.866025403784439,1.,0.866025403784439,1.,0.866025403784439,
1.,0.866025403784439,1.,0.866025403784439,1.,0.866025403784439,1.,0.866025403784439,
1.,0.866025403784439,1.,0.866025403784439,1.,0.866025403784439,1.,0.866025403784439,
1.,0.866025403784439,1.,0.866025403784439,1.,0.866025403784439,1.,0.866025403784439,
1.,0.866025403784439,1.,0.866025403784439,1.,0.866025403784439,1.,0.866025403784439,
1.),(1.,0.866025403784439,1.,0.866025403784439,1.,0.866025403784439,1.,
0.866025403784439,1.,0.866025403784439,1.,0.866025403784439,1.,0.866025403784439,
1.,0.866025403784439,1.,0.866025403784439,1.,0.866025403784439,1.,0.866025403784439,
1.,0.866025403784439,1.,0.866025403784439,1.,0.866025403784439,1.,0.866025403784439,
1.,0.866025403784439,1.,0.866025403784439,1.,0.866025403784439,1.,0.866025403784439,
1.,0.866025403784439,1.,0.866025403784439,1.,0.866025403784439,1.,0.866025403784439,
1.,0.866025403784439,1.,0.866025403784439,1.,0.866025403784439,1.,0.866025403784439,
1.,0.866025403784439,1.,0.866025403784439,1.,0.866025403784439,1.,0.866025403784439,
1.,0.866025403784439,1.,0.866025403784439,1.,0.866025403784439,1.,0.866025403784439,
1.,0.866025403784439,1.,0.866025403784439,1.,0.866025403784439,1.,0.866025403784439,
1.,0.866025403784439,1.,0.866025403784439,1.,0.866025403784439,1.,0.866025403784439,
1.,0.866025403784439,1.,0.866025403784439,1.,0.866025403784439,1.,0.866025403784439,
1.,0.866025403784439,1.,0.866025403784439,1.,0.866025403784439,1.,0.866025403784439,
1.,0.866025403784439,1.,0.866025403784439,1.,0.866025403784439,1.,0.866025403784439,
1.,0.866025403784439,1.,0.866025403784439,1.,0.866025403784439,1.,0.866025403784439,
1.,0.866025403784439,1.,0.866025403784439,1.,0.866025403784439,1.,0.866025403784439,
1.,0.866025403784439,1.,0.866025403784439,1.,0.866025403784439,1.,0.866025403784439,
1.,0.866025403784439,1.,0.866025403784439,1.,0.866025403784439,1.,0.866025403784439,
1.,0.866025403784439,1.,0.866025403784439,1.,0.866025403784439,1.,0.866025403784439,
1.,0.866025403784439,1.,0.866025403784439,1.,0.866025403784439,1.,0.866025403784439,
1.,0.866025403784439,1.,0.866025403784439,1.,0.866025403784439,1.,0.866025403784439,
1.,0.866025403784439,1.,0.866025403784439,1.,0.866025403784439,1.,0.866025403784439,
1.,0.866025403784439,1.,0.866025403784439,1.,0.866025403784439,1.,0.866025403784439,
1.,0.866025403784439,1.,0.866025403784439,1.,0.866025403784439,1.,0.866025403784439,
1.,0.866025403784439,1.,0.866025403784439,1.,0.866025403784439,1.,0.866025403784439,
1.,0.866025403784439,1.,0.866025403784439,1.,0.866025403784439,1.,0.866025403784439,
1.,0.866025403784439,1.,0.866025403784439,1.,0.866025403784439,1.,0.866025403784439,
1.,0.866025403784439,1.,0.866025403784439,1.,0.866025403784439,1.,0.866025403784439,
1.,0.866025403784439,1.,0.866025403784439,1.,0.866025403784439,1.,0.866025403784439,
1.,0.866025403784439,1.,0.866025403784439,1.,0.866025403784439,1.,0.866025403784439,
1.,0.866025403784439,1.,0.866025403784439,1.,0.866025403784439,1.,0.866025403784439,
1.,0.866025403784439,1.,0.866025403784439,1.,0.866025403784439,1.,0.866025403784439,
1.,0.866025403784439,1.,0.866025403784439,1.,0.866025403784439,1.,0.866025403784439,
1.,0.866025403784439,1.,0.866025403784439,1.,0.866025403784439,1.,0.866025403784439,
1.,0.866025403784439,1.,0.866025403784439,1.,0.866025403784439,1.,0.866025403784439,
1.,0.866025403784439,1.,0.866025403784439,1.,0.866025403784439,1.,0.866025403784439,
1.,0.866025403784439,1.,0.866025403784439,1.,0.866025403784439,1.,0.866025403784439,
1.,0.866025403784439,1.,0.866025403784439,1.,0.866025403784439,1.,0.866025403784439,
1.,0.866025403784439,1.,0.866025403784439,1.,0.866025403784439,1.,0.866025403784439,
1.,0.866025403784439,1.,0.866025403784439,1.,0.866025403784439,1.,0.866025403784439,
1.,0.866025403784439,1.,0.866025403784439,1.,0.866025403784439,1.,0.866025403784439,
1.,0.866025403784439,1.,0.866025403784439,1.,0.866025403784439,1.,0.866025403784439,
1.,0.866025403784439,1.,0.866025403784439,1.,0.866025403784439,1.,0.866025403784439,
1.,0.866025403784439,1.,0.866025403784439,1.,0.866025403784439,1.,0.866025403784439,
1.,0.866025403784439,1.,0.866025403784439,1.,0.866025403784439,1.,0.866025403784439,
1.,0.866025403784439,1.,0.866025403784439,1.,0.866025403784439,1.,0.866025403784439,
1.,0.866025403784439,1.,0.866025403784439,1.,0.866025403784439,1.,0.866025403784439,
1.,0.866025403784439,1.,0.866025403784439,1.,0.866025403784439,1.,0.866025403784439,
1.,0.866025403784439,1.,0.866025403784439,1.,0.866025403784439,1.,0.866025403784439,
1.,0.866025403784439,1.,0.866025403784439,1.,0.866025403784439,1.,0.866025403784439,
1.,0.866025403784439,1.,0.866025403784439,1.,0.866025403784439,1.,0.866025403784439,
1.,0.866025403784439,1.,0.866025403784439,1.,0.866025403784439,1.,0.866025403784439,
1.,0.866025403784439,1.,0.866025403784439,1.,0.866025403784439,1.,0.866025403784439,
1.,0.866025403784439,1.,0.866025403784439,1.,0.866025403784439,1.,0.866025403784439,
1.,0.866025403784439,1.,0.866025403784439,1.,0.866025403784439,1.,0.866025403784439,
1.,0.866025403784439,1.,0.866025403784439,1.,0.866025403784439,1.,0.866025403784439,
1.,0.866025403784439,1.,0.866025403784439,1.,0.866025403784439,1.,0.866025403784439,
1.,0.866025403784439,1.,0.866025403784439,1.,0.866025403784439,1.,0.866025403784439,
1.,0.866025403784439,1.,0.866025403784439,1.,0.866025403784439,1.,0.866025403784439,
1.,0.866025403784439,1.,0.866025403784439,1.,0.866025403784439,1.,0.866025403784439,
1.,0.866025403784439,1.,0.866025403784439,1.,0.866025403784439,1.,0.866025403784439,
1.,0.866025403784439,1.,0.866025403784439,1.,0.866025403784439,1.,0.866025403784439,
1.,0.866025403784439,1.,0.866025403784439,1.,0.866025403784439,1.,0.866025403784439,
1.,0.866025403784439,1.,0.866025403784439,1.,0.866025403784439,1.,0.866025403784439,
1.,0.866025403784439,1.,0.866025403784439,1.,0.866025403784439,1.,0.866025403784439,
1.,0.866025403784439,1.,0.866025403784439,1.,0.866025403784439,1.,0.866025403784439,
1.,0.866025403784439,1.,0.866025403784439,1.,0.866025403784439,1.,0.866025403784439,
1.,0.866025403784439,1.,0.866025403784439,1.,0.866025403784439,1.,0.866025403784439,
1.,0.866025403784439,1.,0.866025403784439,1.,0.866025403784439,1.,0.866025403784439,
1.,0.866025403784439,1.,0.866025403784439,1.,0.866025403784439,1.,0.866025403784439,
1.,0.866025403784439,1.,0.866025403784439,1.,0.866025403784439,1.,0.866025403784439,
1.,0.866025403784439,1.,0.866025403784439,1.,0.866025403784439,1.,0.866025403784439,
1.,0.866025403784439,1.,0.866025403784439,1.,0.866025403784439,1.,0.866025403784439,
1.,0.866025403784439,1.,0.866025403784439,1.,0.866025403784439,1.,0.866025403784439,
1.,0.866025403784439,1.,0.866025403784439,1.,0.866025403784439,1.,0.866025403784439,
1.,0.866025403784439,1.,0.866025403784439,1.,0.866025403784439,1.,0.866025403784439,
1.,0.866025403784439,1.,0.866025403784439,1.,0.866025403784439,1.,0.866025403784439,
1.,0.866025403784439,1.,0.866025403784439,1.,0.866025403784439,1.,0.866025403784439,
1.,0.866025403784439,1.,0.866025403784439,1.,0.866025403784439,1.,0.866025403784439,
1.,0.866025403784439,1.,0.866025403784439,1.,0.866025403784439,1.,0.866025403784439,
1.,0.866025403784439,1.,0.866025403784439,1.,0.866025403784439,1.,0.866025403784439,
1.,0.866025403784439,1.,0.866025403784439,1.,0.866025403784439,1.,0.866025403784439,
1.,0.866025403784439,1.,0.866025403784439,1.,0.866025403784439,1.,0.866025403784439,
1.,0.866025403784439,1.,0.866025403784439,1.,0.866025403784439,1.,0.866025403784439,
1.,0.866025403784439,1.,0.866025403784439,1.,0.866025403784439,1.,0.866025403784439,
1.,0.866025403784439,1.,0.866025403784439,1.,0.866025403784439,1.,0.866025403784439,
1.,0.866025403784439,1.,0.866025403784439,1.,0.866025403784439,1.,0.866025403784439,
1.,0.866025403784439,1.,0.866025403784439,1.,0.866025403784439,1.,0.866025403784439,
1.,0.866025403784439,1.,0.866025403784439,1.,0.866025403784439,1.,0.866025403784439,
1.,0.866025403784439,1.,0.866025403784439,1.,0.866025403784439,1.,0.866025403784439,
1.,0.866025403784439,1.,0.866025403784439,1.,0.866025403784439,1.,0.866025403784439,
1.,0.866025403784439,1.,0.866025403784439,1.,0.866025403784439,1.,0.866025403784439,
1.,0.866025403784439,1.,0.866025403784439,1.,0.866025403784439,1.,0.866025403784439,
1.,0.866025403784439,1.,0.866025403784439,1.,0.866025403784439,1.,0.866025403784439,
1.,0.866025403784439,1.,0.866025403784439,1.,0.866025403784439,1.,0.866025403784439,
1.,0.866025403784439,1.,0.866025403784439,1.,0.866025403784439,1.,0.866025403784439,
1.,0.866025403784439,1.,0.866025403784439,1.,0.866025403784439,1.,0.866025403784439,
1.,0.866025403784439,1.,0.866025403784439,1.,0.866025403784439,1.,0.866025403784439,
1.,0.866025403784439,1.,0.866025403784439,1.,0.866025403784439,1.,0.866025403784439,
1.,0.866025403784439,1.,0.866025403784439,1.,0.866025403784439,1.,0.866025403784439,
1.,0.866025403784439,1.,0.866025403784439,1.,0.866025403784439,1.,0.866025403784439,
1.,0.866025403784439,1.,0.866025403784439,1.,0.866025403784439,1.,0.866025403784439,
1.,0.866025403784439,1.,0.866025403784439,1.,0.866025403784439,1.,0.866025403784439,
1.,0.866025403784439,1.,0.866025403784439,1.,0.866025403784439,1.,0.866025403784439,
1.,0.866025403784439,1.,0.866025403784439,1.,0.866025403784439,1.,0.866025403784439,
1.,0.866025403784439,1.,0.866025403784439,1.,0.866025403784439,1.,0.866025403784439,
1.,0.866025403784439,1.,0.866025403784439,1.,0.866025403784439,1.,0.866025403784439,
1.,0.866025403784439,1.,0.866025403784439,1.,0.866025403784439,1.,0.866025403784439,
1.,0.866025403784439,1.,0.866025403784439,1.,0.866025403784439,1.,0.866025403784439,
1.,0.866025403784439,1.,0.866025403784439,1.,0.866025403784439,1.,0.866025403784439,
1.,0.866025403784439,1.,0.866025403784439,1.,0.866025403784439,1.,0.866025403784439,
1.,0.866025403784439,1.,0.866025403784439,1.,0.866025403784439,1.,0.866025403784439,
1.,0.866025403784439,1.,0.866025403784439,1.,0.866025403784439,1.,0.866025403784439,
1.,0.866025403784439,1.,0.866025403784439,1.,0.866025403784439,1.,0.866025403784439,
1.,0.866025403784439,1.,0.866025403784439,1.,0.866025403784439,1.,0.866025403784439,
1.,0.866025403784439,1.,0.866025403784439,1.,0.866025403784439,1.,0.866025403784439,
1.,0.866025403784439,1.,0.866025403784439,1.,0.866025403784439,1.,0.866025403784439,
1.,0.866025403784439,1.,0.866025403784439,1.,0.866025403784439,1.,0.866025403784439,
1.,0.866025403784439,1.,0.866025403784439,1.,0.866025403784439,1.,0.866025403784439,
1.,0.866025403784439,1.,0.866025403784439,1.,0.866025403784439,1.,0.866025403784439,
1.,0.866025403784439,1.,0.866025403784439,1.,0.866025403784439,1.,0.866025403784439,
1.,0.866025403784439,1.,0.866025403784439,1.,0.866025403784439,1.)))
REPRESENTATION_ITEM('')
SURFACE()
);
#181=(
BOUNDED_SURFACE()
B_SPLINE_SURFACE(3,2,((#39526,#39527,#39528),(#39529,#39530,#39531),(#39532,
#39533,#39534),(#39535,#39536,#39537),(#39538,#39539,#39540),(#39541,#39542,
#39543),(#39544,#39545,#39546),(#39547,#39548,#39549),(#39550,#39551,#39552),
(#39553,#39554,#39555),(#39556,#39557,#39558),(#39559,#39560,#39561),(#39562,
#39563,#39564),(#39565,#39566,#39567),(#39568,#39569,#39570),(#39571,#39572,
#39573),(#39574,#39575,#39576),(#39577,#39578,#39579),(#39580,#39581,#39582),
(#39583,#39584,#39585),(#39586,#39587,#39588),(#39589,#39590,#39591),(#39592,
#39593,#39594),(#39595,#39596,#39597),(#39598,#39599,#39600),(#39601,#39602,
#39603),(#39604,#39605,#39606),(#39607,#39608,#39609),(#39610,#39611,#39612),
(#39613,#39614,#39615),(#39616,#39617,#39618),(#39619,#39620,#39621),(#39622,
#39623,#39624),(#39625,#39626,#39627),(#39628,#39629,#39630),(#39631,#39632,
#39633),(#39634,#39635,#39636),(#39637,#39638,#39639),(#39640,#39641,#39642),
(#39643,#39644,#39645),(#39646,#39647,#39648),(#39649,#39650,#39651)),
 .UNSPECIFIED.,.F.,.F.,.F.)
B_SPLINE_SURFACE_WITH_KNOTS((4,2,2,2,2,2,2,2,2,2,2,2,2,2,2,2,2,2,2,2,4),
(3,3),(0.0174298903432871,0.0185192584897425,0.019608626636198,0.0206979947826534,
0.0217873629291089,0.0223320470023366,0.0228767310755643,0.0239660992220198,
0.0250554673684752,0.025600151441703,0.0261448355149307,0.0272342036613861,
0.0277788877346139,0.0283235718078416,0.029412939954297,0.0305023081007525,
0.0315916762472079,0.0326810443936634,0.0332257284668911,0.0337704125401188,
0.0348597806865743),(0.,1.),.UNSPECIFIED.)
GEOMETRIC_REPRESENTATION_ITEM()
RATIONAL_B_SPLINE_SURFACE(((1.,0.706866009891761,1.),(1.,0.707709971120244,
1.),(1.,0.706378287598767,1.),(1.,0.699609550425451,1.),(1.,0.694251408628478,
1.),(1.,0.680153613237048,1.),(1.,0.671289168508122,1.),(1.,0.651466158778394,
1.),(1.,0.64048617306175,1.),(1.,0.623110795499309,1.),(1.,0.617152560263192,
1.),(1.,0.605316890643934,1.),(1.,0.599412164382846,1.),(1.,0.581980631318285,
1.),(1.,0.570694981696628,1.),(1.,0.550546690048529,1.),(1.,0.542015457727399,
1.),(1.,0.532586496259878,1.),(1.,0.530005387777312,1.),(1.,0.526142825846638,
1.),(1.,0.524867626920824,1.),(1.,0.523238184105568,1.),(1.,0.525025712186939,
1.),(1.,0.531687007265021,1.),(1.,0.534590177846375,1.),(1.,0.541481193611421,
1.),(1.,0.545459204735857,1.),(1.,0.558669094849934,1.),(1.,0.569250982154013,
1.),(1.,0.591912604715541,1.),(1.,0.603810048297302,1.),(1.,0.627370297955306,
1.),(1.,0.639116797025499,1.),(1.,0.660432022552727,1.),(1.,0.670115428840362,
1.),(1.,0.682559312106454,1.),(1.,0.686375173907005,1.),(1.,0.693053327636874,
1.),(1.,0.695935943959762,1.),(1.,0.703157954701394,1.),(1.,0.706075946662903,
1.),(1.,0.706882331541542,1.)))
REPRESENTATION_ITEM('')
SURFACE()
);
#182=(
BOUNDED_SURFACE()
B_SPLINE_SURFACE(3,2,((#39652,#39653,#39654),(#39655,#39656,#39657),(#39658,
#39659,#39660),(#39661,#39662,#39663),(#39664,#39665,#39666),(#39667,#39668,
#39669),(#39670,#39671,#39672),(#39673,#39674,#39675),(#39676,#39677,#39678),
(#39679,#39680,#39681),(#39682,#39683,#39684),(#39685,#39686,#39687),(#39688,
#39689,#39690),(#39691,#39692,#39693),(#39694,#39695,#39696),(#39697,#39698,
#39699),(#39700,#39701,#39702),(#39703,#39704,#39705),(#39706,#39707,#39708),
(#39709,#39710,#39711),(#39712,#39713,#39714),(#39715,#39716,#39717),(#39718,
#39719,#39720),(#39721,#39722,#39723),(#39724,#39725,#39726),(#39727,#39728,
#39729),(#39730,#39731,#39732),(#39733,#39734,#39735),(#39736,#39737,#39738),
(#39739,#39740,#39741),(#39742,#39743,#39744),(#39745,#39746,#39747),(#39748,
#39749,#39750),(#39751,#39752,#39753),(#39754,#39755,#39756),(#39757,#39758,
#39759),(#39760,#39761,#39762),(#39763,#39764,#39765),(#39766,#39767,#39768),
(#39769,#39770,#39771),(#39772,#39773,#39774),(#39775,#39776,#39777),(#39778,
#39779,#39780),(#39781,#39782,#39783)),.UNSPECIFIED.,.F.,.F.,.F.)
B_SPLINE_SURFACE_WITH_KNOTS((4,2,2,2,2,2,2,2,2,2,2,2,2,2,2,2,2,2,2,2,2,
4),(3,3),(0.0174355915143997,0.0185253159840497,0.0196150404536998,0.0207047649233498,
0.0217944893929999,0.0223393516278249,0.0228842138626499,0.0239739383323,
0.02506366280195,0.0256085250367751,0.0261533872716001,0.0272431117412501,
0.0277879739760752,0.0283328362109002,0.0288776984457252,0.0294225606805503,
0.0305122851502003,0.0316020096198504,0.0326917340895004,0.0332365963243254,
0.0337814585591505,0.0348711830288005),(0.,1.),.UNSPECIFIED.)
GEOMETRIC_REPRESENTATION_ITEM()
RATIONAL_B_SPLINE_SURFACE(((1.,0.524035202708704,1.),(1.,0.52369296431929,
1.),(1.,0.526394142477004,1.),(1.,0.536829948771709,1.),(1.,0.544467574436789,
1.),(1.,0.563002631288668,1.),(1.,0.574012202433206,1.),(1.,0.596893654025968,
1.),(1.,0.608827575768556,1.),(1.,0.626487538313077,1.),(1.,0.632339905306929,
1.),(1.,0.643592429688047,1.),(1.,0.649024086836218,1.),(1.,0.664570352465133,
1.),(1.,0.673967207524643,1.),(1.,0.689780774219124,1.),(1.,0.695966905675102,
1.),(1.,0.702388249318966,1.),(1.,0.704051452628861,1.),(1.,0.706358678483347,
1.),(1.,0.706995125392999,1.),(1.,0.707289148463133,1.),(1.,0.705381051410457,
1.),(1.,0.699485171860676,1.),(1.,0.696993043119987,1.),(1.,0.69112912697355,
1.),(1.,0.687757727348698,1.),(1.,0.680223099202971,1.),(1.,0.676059589951543,
1.),(1.,0.667018043806083,1.),(1.,0.662112134338359,1.),(1.,0.646674940339596,
1.),(1.,0.635448505441412,1.),(1.,0.612137111297426,1.),(1.,0.599953887245996,
1.),(1.,0.576916856514265,1.),(1.,0.565959879293194,1.),(1.,0.551559273150467,
1.),(1.,0.547084490609781,1.),(1.,0.539237982614899,1.),(1.,0.53584249288952,
1.),(1.,0.527460168857136,1.),(1.,0.524283085212896,1.),(1.,0.524030615668023,
1.)))
REPRESENTATION_ITEM('')
SURFACE()
);
#183=(
BOUNDED_CURVE()
B_SPLINE_CURVE(2,(#11448,#11449,#11450),.UNSPECIFIED.,.F.,.F.)
B_SPLINE_CURVE_WITH_KNOTS((3,3),(1.85021493467955,2.79463772249644),
 .UNSPECIFIED.)
CURVE()
GEOMETRIC_REPRESENTATION_ITEM()
RATIONAL_B_SPLINE_CURVE((1.69747704818698,1.78740157480315,1.78740157480315))
REPRESENTATION_ITEM('')
);
#184=(
BOUNDED_CURVE()
B_SPLINE_CURVE(2,(#11451,#11452,#11453),.UNSPECIFIED.,.F.,.F.)
B_SPLINE_CURVE_WITH_KNOTS((3,3),(2.79463772249644,3.73906051031331),
 .UNSPECIFIED.)
CURVE()
GEOMETRIC_REPRESENTATION_ITEM()
RATIONAL_B_SPLINE_CURVE((1.78740157480315,1.78740157480315,1.69747704818698))
REPRESENTATION_ITEM('')
);
#185=(
BOUNDED_CURVE()
B_SPLINE_CURVE(2,(#11462,#11463,#11464),.UNSPECIFIED.,.F.,.F.)
B_SPLINE_CURVE_WITH_KNOTS((3,3),(1.85021493467955,2.79463772249643),
 .UNSPECIFIED.)
CURVE()
GEOMETRIC_REPRESENTATION_ITEM()
RATIONAL_B_SPLINE_CURVE((1.69747704818698,1.78740157480315,1.78740157480315))
REPRESENTATION_ITEM('')
);
#186=(
BOUNDED_CURVE()
B_SPLINE_CURVE(2,(#11465,#11466,#11467),.UNSPECIFIED.,.F.,.F.)
B_SPLINE_CURVE_WITH_KNOTS((3,3),(2.79463772249643,3.73906051031332),
 .UNSPECIFIED.)
CURVE()
GEOMETRIC_REPRESENTATION_ITEM()
RATIONAL_B_SPLINE_CURVE((1.78740157480315,1.78740157480315,1.69747704818698))
REPRESENTATION_ITEM('')
);
#187=(
BOUNDED_CURVE()
B_SPLINE_CURVE(2,(#11476,#11477,#11478),.UNSPECIFIED.,.F.,.F.)
B_SPLINE_CURVE_WITH_KNOTS((3,3),(1.85021493467955,2.79463772249644),
 .UNSPECIFIED.)
CURVE()
GEOMETRIC_REPRESENTATION_ITEM()
RATIONAL_B_SPLINE_CURVE((1.69747704818698,1.78740157480315,1.78740157480315))
REPRESENTATION_ITEM('')
);
#188=(
BOUNDED_CURVE()
B_SPLINE_CURVE(2,(#11479,#11480,#11481),.UNSPECIFIED.,.F.,.F.)
B_SPLINE_CURVE_WITH_KNOTS((3,3),(2.79463772249644,3.73906051031331),
 .UNSPECIFIED.)
CURVE()
GEOMETRIC_REPRESENTATION_ITEM()
RATIONAL_B_SPLINE_CURVE((1.78740157480315,1.78740157480315,1.69747704818698))
REPRESENTATION_ITEM('')
);
#189=(
BOUNDED_CURVE()
B_SPLINE_CURVE(2,(#11490,#11491,#11492),.UNSPECIFIED.,.F.,.F.)
B_SPLINE_CURVE_WITH_KNOTS((3,3),(1.85021493467955,2.79463772249643),
 .UNSPECIFIED.)
CURVE()
GEOMETRIC_REPRESENTATION_ITEM()
RATIONAL_B_SPLINE_CURVE((1.69747704818698,1.78740157480315,1.78740157480315))
REPRESENTATION_ITEM('')
);
#190=(
BOUNDED_CURVE()
B_SPLINE_CURVE(2,(#11493,#11494,#11495),.UNSPECIFIED.,.F.,.F.)
B_SPLINE_CURVE_WITH_KNOTS((3,3),(2.79463772249643,3.73906051031332),
 .UNSPECIFIED.)
CURVE()
GEOMETRIC_REPRESENTATION_ITEM()
RATIONAL_B_SPLINE_CURVE((1.78740157480315,1.78740157480315,1.69747704818698))
REPRESENTATION_ITEM('')
);
#191=(
BOUNDED_CURVE()
B_SPLINE_CURVE(2,(#11504,#11505,#11506),.UNSPECIFIED.,.F.,.F.)
B_SPLINE_CURVE_WITH_KNOTS((3,3),(1.85021493467955,2.79463772249643),
 .UNSPECIFIED.)
CURVE()
GEOMETRIC_REPRESENTATION_ITEM()
RATIONAL_B_SPLINE_CURVE((1.69747704818698,1.78740157480315,1.78740157480316))
REPRESENTATION_ITEM('')
);
#192=(
BOUNDED_CURVE()
B_SPLINE_CURVE(2,(#11507,#11508,#11509),.UNSPECIFIED.,.F.,.F.)
B_SPLINE_CURVE_WITH_KNOTS((3,3),(2.79463772249643,3.73906051031331),
 .UNSPECIFIED.)
CURVE()
GEOMETRIC_REPRESENTATION_ITEM()
RATIONAL_B_SPLINE_CURVE((1.78740157480315,1.78740157480316,1.69747704818699))
REPRESENTATION_ITEM('')
);
#193=(
BOUNDED_CURVE()
B_SPLINE_CURVE(2,(#11518,#11519,#11520),.UNSPECIFIED.,.F.,.F.)
B_SPLINE_CURVE_WITH_KNOTS((3,3),(1.85021493467955,2.79463772249643),
 .UNSPECIFIED.)
CURVE()
GEOMETRIC_REPRESENTATION_ITEM()
RATIONAL_B_SPLINE_CURVE((1.69747704818698,1.78740157480315,1.78740157480315))
REPRESENTATION_ITEM('')
);
#194=(
BOUNDED_CURVE()
B_SPLINE_CURVE(2,(#11521,#11522,#11523),.UNSPECIFIED.,.F.,.F.)
B_SPLINE_CURVE_WITH_KNOTS((3,3),(2.79463772249643,3.73906051031331),
 .UNSPECIFIED.)
CURVE()
GEOMETRIC_REPRESENTATION_ITEM()
RATIONAL_B_SPLINE_CURVE((1.78740157480315,1.78740157480315,1.69747704818698))
REPRESENTATION_ITEM('')
);
#195=(
BOUNDED_CURVE()
B_SPLINE_CURVE(2,(#14999,#15000,#15001,#15002,#15003,#15004,#15005,#15006,
#15007,#15008,#15009,#15010,#15011,#15012,#15013,#15014,#15015,#15016,#15017,
#15018,#15019,#15020,#15021,#15022,#15023,#15024,#15025,#15026,#15027,#15028,
#15029,#15030,#15031,#15032,#15033,#15034,#15035,#15036,#15037,#15038,#15039,
#15040,#15041,#15042,#15043,#15044,#15045,#15046,#15047,#15048,#15049,#15050,
#15051,#15052,#15053,#15054,#15055,#15056,#15057,#15058,#15059,#15060,#15061,
#15062,#15063,#15064,#15065,#15066,#15067,#15068,#15069,#15070,#15071,#15072,
#15073,#15074,#15075,#15076,#15077,#15078,#15079,#15080,#15081,#15082,#15083,
#15084,#15085,#15086,#15087,#15088,#15089,#15090,#15091,#15092,#15093,#15094,
#15095,#15096,#15097,#15098,#15099,#15100,#15101,#15102,#15103,#15104,#15105,
#15106,#15107,#15108,#15109,#15110,#15111,#15112,#15113,#15114,#15115,#15116,
#15117,#15118,#15119,#15120,#15121,#15122,#15123,#15124,#15125,#15126,#15127,
#15128,#15129,#15130,#15131,#15132,#15133,#15134,#15135,#15136,#15137,#15138,
#15139,#15140,#15141,#15142,#15143,#15144,#15145,#15146,#15147,#15148,#15149,
#15150,#15151,#15152,#15153,#15154,#15155,#15156,#15157,#15158,#15159,#15160,
#15161,#15162,#15163,#15164,#15165,#15166,#15167,#15168,#15169,#15170,#15171,
#15172,#15173,#15174,#15175,#15176,#15177,#15178,#15179,#15180,#15181,#15182,
#15183,#15184,#15185,#15186,#15187,#15188,#15189,#15190,#15191,#15192,#15193,
#15194,#15195,#15196,#15197,#15198,#15199,#15200,#15201,#15202,#15203,#15204,
#15205,#15206,#15207,#15208,#15209,#15210,#15211,#15212,#15213,#15214,#15215,
#15216,#15217,#15218,#15219,#15220,#15221,#15222,#15223,#15224,#15225,#15226,
#15227,#15228,#15229,#15230,#15231,#15232,#15233,#15234,#15235,#15236,#15237,
#15238,#15239,#15240,#15241,#15242,#15243,#15244,#15245,#15246,#15247,#15248,
#15249,#15250,#15251,#15252,#15253,#15254,#15255,#15256,#15257,#15258,#15259,
#15260,#15261,#15262,#15263,#15264,#15265,#15266,#15267,#15268,#15269,#15270,
#15271),.UNSPECIFIED.,.F.,.F.)
B_SPLINE_CURVE_WITH_KNOTS((3,2,2,2,2,2,2,2,2,2,2,2,2,2,2,2,2,2,2,2,2,2,
2,2,2,2,2,2,2,2,2,2,2,2,2,2,2,2,2,2,2,2,2,2,2,2,2,2,2,2,2,2,2,2,2,2,2,2,
2,2,2,2,2,2,2,2,2,2,2,2,2,2,2,2,2,2,2,2,2,2,2,2,2,2,2,2,2,2,2,2,2,2,2,2,
2,2,2,2,2,2,2,2,2,2,2,2,2,2,2,2,2,2,2,2,2,2,2,2,2,2,2,2,2,2,2,2,2,2,2,2,
2,2,2,2,2,2,3),(0.700304458117265,0.701646090534979,0.703703703703704,0.705761316872428,
0.707818930041152,0.709876543209877,0.711934156378601,0.713991769547325,
0.716049382716049,0.718106995884774,0.720164609053498,0.722222222222222,
0.724279835390947,0.726337448559671,0.728395061728395,0.730452674897119,
0.732510288065844,0.734567901234568,0.736625514403292,0.738683127572016,
0.740740740740741,0.742798353909465,0.744855967078189,0.746913580246914,
0.748971193415638,0.751028806584362,0.753086419753086,0.755144032921811,
0.757201646090535,0.759259259259259,0.761316872427984,0.763374485596708,
0.765432098765432,0.767489711934156,0.769547325102881,0.771604938271605,
0.773662551440329,0.775720164609053,0.777777777777778,0.779835390946502,
0.781893004115226,0.783950617283951,0.786008230452675,0.788065843621399,
0.790123456790123,0.792181069958848,0.794238683127572,0.796296296296296,
0.798353909465021,0.800411522633745,0.802469135802469,0.804526748971193,
0.806584362139918,0.808641975308642,0.810699588477366,0.812757201646091,
0.814814814814815,0.816872427983539,0.818930041152263,0.820987654320988,
0.823045267489712,0.825102880658436,0.827160493827161,0.829218106995885,
0.831275720164609,0.833333333333333,0.835390946502058,0.837448559670782,
0.839506172839506,0.84156378600823,0.843621399176955,0.845679012345679,
0.847736625514403,0.849794238683128,0.851851851851852,0.853909465020576,
0.8559670781893,0.858024691358025,0.860082304526749,0.862139917695473,0.864197530864197,
0.866255144032922,0.868312757201646,0.87037037037037,0.872427983539095,
0.874485596707819,0.876543209876543,0.878600823045268,0.880658436213992,
0.882716049382716,0.88477366255144,0.886831275720165,0.888888888888889,
0.890946502057613,0.893004115226337,0.895061728395062,0.897119341563786,
0.89917695473251,0.901234567901235,0.903292181069959,0.905349794238683,
0.907407407407407,0.909465020576132,0.911522633744856,0.91358024691358,
0.915637860082305,0.917695473251029,0.919753086419753,0.921810699588477,
0.923868312757202,0.925925925925926,0.92798353909465,0.930041152263374,
0.932098765432099,0.934156378600823,0.936213991769547,0.938271604938272,
0.940329218106996,0.94238683127572,0.944444444444444,0.946502057613169,
0.948559670781893,0.950617283950617,0.952674897119342,0.954732510288066,
0.95679012345679,0.958847736625514,0.960905349794239,0.962962962962963,
0.965020576131687,0.967078189300412,0.969135802469136,0.97119341563786,
0.973251028806584,0.975308641975309,0.977366255144033,0.977769992664587),
 .UNSPECIFIED.)
CURVE()
GEOMETRIC_REPRESENTATION_ITEM()
RATIONAL_B_SPLINE_CURVE((0.939206117316363,0.912644094543595,1.,0.866025403784439,
1.,0.866025403784439,1.,0.866025403784439,1.,0.866025403784439,1.,0.866025403784439,
1.,0.866025403784439,1.,0.866025403784439,1.,0.866025403784439,1.,0.866025403784439,
1.,0.866025403784439,1.,0.866025403784439,1.,0.866025403784439,1.,0.866025403784439,
1.,0.866025403784439,1.,0.866025403784439,1.,0.866025403784439,1.,0.866025403784439,
1.,0.866025403784439,1.,0.866025403784439,1.,0.866025403784439,1.,0.866025403784439,
1.,0.866025403784439,1.,0.866025403784439,1.,0.866025403784439,1.,0.866025403784439,
1.,0.866025403784439,1.,0.866025403784439,1.,0.866025403784439,1.,0.866025403784439,
1.,0.866025403784439,1.,0.866025403784439,1.,0.866025403784439,1.,0.866025403784439,
1.,0.866025403784439,1.,0.866025403784439,1.,0.866025403784439,1.,0.866025403784439,
1.,0.866025403784439,1.,0.866025403784439,1.,0.866025403784439,1.,0.866025403784439,
1.,0.866025403784439,1.,0.866025403784439,1.,0.866025403784439,1.,0.866025403784439,
1.,0.866025403784439,1.,0.866025403784439,1.,0.866025403784439,1.,0.866025403784439,
1.,0.866025403784439,1.,0.866025403784439,1.,0.866025403784439,1.,0.866025403784439,
1.,0.866025403784439,1.,0.866025403784439,1.,0.866025403784439,1.,0.866025403784439,
1.,0.866025403784439,1.,0.866025403784439,1.,0.866025403784439,1.,0.866025403784439,
1.,0.866025403784439,1.,0.866025403784439,1.,0.866025403784439,1.,0.866025403784439,
1.,0.866025403784439,1.,0.866025403784439,1.,0.866025403784439,1.,0.866025403784439,
1.,0.866025403784439,1.,0.866025403784439,1.,0.866025403784439,1.,0.866025403784439,
1.,0.866025403784439,1.,0.866025403784439,1.,0.866025403784439,1.,0.866025403784439,
1.,0.866025403784439,1.,0.866025403784439,1.,0.866025403784439,1.,0.866025403784439,
1.,0.866025403784439,1.,0.866025403784439,1.,0.866025403784439,1.,0.866025403784439,
1.,0.866025403784439,1.,0.866025403784439,1.,0.866025403784439,1.,0.866025403784439,
1.,0.866025403784439,1.,0.866025403784439,1.,0.866025403784439,1.,0.866025403784439,
1.,0.866025403784439,1.,0.866025403784439,1.,0.866025403784439,1.,0.866025403784439,
1.,0.866025403784439,1.,0.866025403784439,1.,0.866025403784439,1.,0.866025403784439,
1.,0.866025403784439,1.,0.866025403784439,1.,0.866025403784439,1.,0.866025403784439,
1.,0.866025403784439,1.,0.866025403784439,1.,0.866025403784439,1.,0.866025403784439,
1.,0.866025403784439,1.,0.866025403784439,1.,0.866025403784439,1.,0.866025403784439,
1.,0.866025403784439,1.,0.866025403784439,1.,0.866025403784439,1.,0.866025403784439,
1.,0.866025403784439,1.,0.866025403784439,1.,0.866025403784439,1.,0.866025403784439,
1.,0.866025403784439,1.,0.866025403784439,1.,0.866025403784439,1.,0.866025403784439,
1.,0.866025403784439,1.,0.866025403784439,1.,0.866025403784439,1.,0.866025403784439,
1.,0.866025403784439,1.,0.866025403784439,1.,0.866025403784439,1.,0.866025403784439,
1.,0.866025403784439,1.,0.973711982351429,0.957740246914744))
REPRESENTATION_ITEM('')
);
#196=(
BOUNDED_CURVE()
B_SPLINE_CURVE(2,(#15272,#15273,#15274,#15275,#15276,#15277,#15278,#15279,
#15280,#15281,#15282,#15283,#15284,#15285,#15286,#15287,#15288,#15289,#15290,
#15291,#15292,#15293,#15294,#15295,#15296,#15297,#15298,#15299,#15300,#15301,
#15302,#15303,#15304,#15305,#15306,#15307,#15308,#15309,#15310,#15311,#15312,
#15313,#15314,#15315,#15316,#15317,#15318,#15319,#15320,#15321,#15322,#15323,
#15324,#15325,#15326,#15327,#15328,#15329,#15330,#15331,#15332,#15333,#15334,
#15335,#15336,#15337,#15338,#15339,#15340,#15341,#15342,#15343,#15344,#15345,
#15346,#15347,#15348,#15349,#15350,#15351,#15352,#15353,#15354,#15355,#15356,
#15357,#15358,#15359,#15360,#15361,#15362,#15363,#15364,#15365,#15366,#15367,
#15368,#15369,#15370,#15371,#15372,#15373,#15374,#15375,#15376,#15377,#15378,
#15379,#15380,#15381,#15382,#15383,#15384,#15385,#15386,#15387,#15388,#15389,
#15390,#15391,#15392,#15393,#15394,#15395,#15396,#15397,#15398,#15399,#15400,
#15401,#15402,#15403,#15404,#15405,#15406,#15407,#15408,#15409,#15410,#15411,
#15412,#15413,#15414,#15415,#15416,#15417,#15418,#15419,#15420,#15421,#15422,
#15423,#15424,#15425,#15426,#15427,#15428,#15429,#15430,#15431,#15432,#15433,
#15434,#15435,#15436,#15437,#15438,#15439,#15440,#15441,#15442,#15443,#15444,
#15445,#15446,#15447,#15448,#15449,#15450,#15451,#15452,#15453,#15454,#15455,
#15456,#15457,#15458,#15459,#15460,#15461,#15462,#15463,#15464,#15465,#15466,
#15467,#15468,#15469,#15470,#15471,#15472,#15473,#15474,#15475,#15476,#15477,
#15478,#15479,#15480,#15481,#15482,#15483,#15484,#15485,#15486,#15487,#15488,
#15489,#15490,#15491,#15492,#15493,#15494,#15495,#15496,#15497,#15498,#15499,
#15500,#15501,#15502,#15503,#15504,#15505,#15506,#15507,#15508,#15509,#15510,
#15511,#15512,#15513,#15514,#15515,#15516,#15517,#15518,#15519,#15520,#15521,
#15522,#15523,#15524,#15525,#15526,#15527,#15528,#15529,#15530,#15531,#15532,
#15533,#15534,#15535,#15536,#15537,#15538,#15539,#15540,#15541,#15542,#15543,
#15544,#15545,#15546),.UNSPECIFIED.,.F.,.F.)
B_SPLINE_CURVE_WITH_KNOTS((3,2,2,2,2,2,2,2,2,2,2,2,2,2,2,2,2,2,2,2,2,2,
2,2,2,2,2,2,2,2,2,2,2,2,2,2,2,2,2,2,2,2,2,2,2,2,2,2,2,2,2,2,2,2,2,2,2,2,
2,2,2,2,2,2,2,2,2,2,2,2,2,2,2,2,2,2,2,2,2,2,2,2,2,2,2,2,2,2,2,2,2,2,2,2,
2,2,2,2,2,2,2,2,2,2,2,2,2,2,2,2,2,2,2,2,2,2,2,2,2,2,2,2,2,2,2,2,2,2,2,2,
2,2,2,2,2,2,2,3),(0.690118789609514,0.691358024691358,0.693415637860082,
0.695473251028807,0.697530864197531,0.699588477366255,0.701646090534979,
0.703703703703704,0.705761316872428,0.707818930041152,0.709876543209877,
0.711934156378601,0.713991769547325,0.716049382716049,0.718106995884774,
0.720164609053498,0.722222222222222,0.724279835390947,0.726337448559671,
0.728395061728395,0.730452674897119,0.732510288065844,0.734567901234568,
0.736625514403292,0.738683127572016,0.740740740740741,0.742798353909465,
0.744855967078189,0.746913580246914,0.748971193415638,0.751028806584362,
0.753086419753086,0.755144032921811,0.757201646090535,0.759259259259259,
0.761316872427984,0.763374485596708,0.765432098765432,0.767489711934156,
0.769547325102881,0.771604938271605,0.773662551440329,0.775720164609053,
0.777777777777778,0.779835390946502,0.781893004115226,0.783950617283951,
0.786008230452675,0.788065843621399,0.790123456790123,0.792181069958848,
0.794238683127572,0.796296296296296,0.798353909465021,0.800411522633745,
0.802469135802469,0.804526748971193,0.806584362139918,0.808641975308642,
0.810699588477366,0.812757201646091,0.814814814814815,0.816872427983539,
0.818930041152263,0.820987654320988,0.823045267489712,0.825102880658436,
0.827160493827161,0.829218106995885,0.831275720164609,0.833333333333333,
0.835390946502058,0.837448559670782,0.839506172839506,0.84156378600823,
0.843621399176955,0.845679012345679,0.847736625514403,0.849794238683128,
0.851851851851852,0.853909465020576,0.8559670781893,0.858024691358025,0.860082304526749,
0.862139917695473,0.864197530864197,0.866255144032922,0.868312757201646,
0.87037037037037,0.872427983539095,0.874485596707819,0.876543209876543,
0.878600823045268,0.880658436213992,0.882716049382716,0.88477366255144,
0.886831275720165,0.888888888888889,0.890946502057613,0.893004115226337,
0.895061728395062,0.897119341563786,0.89917695473251,0.901234567901235,
0.903292181069959,0.905349794238683,0.907407407407407,0.909465020576132,
0.911522633744856,0.91358024691358,0.915637860082305,0.917695473251029,
0.919753086419753,0.921810699588477,0.923868312757202,0.925925925925926,
0.92798353909465,0.930041152263374,0.932098765432099,0.934156378600823,
0.936213991769547,0.938271604938272,0.940329218106996,0.94238683127572,
0.944444444444444,0.946502057613169,0.948559670781893,0.950617283950617,
0.952674897119342,0.954732510288066,0.95679012345679,0.958847736625514,
0.960905349794239,0.962962962962963,0.965020576131687,0.967078189300412,
0.969135802469136,0.970064444260615),.UNSPECIFIED.)
CURVE()
GEOMETRIC_REPRESENTATION_ITEM()
RATIONAL_B_SPLINE_CURVE((0.935815127542769,0.919311354422782,1.,0.866025403784439,
1.,0.866025403784439,1.,0.866025403784439,1.,0.866025403784439,1.,0.866025403784439,
1.,0.866025403784439,1.,0.866025403784439,1.,0.866025403784439,1.,0.866025403784439,
1.,0.866025403784439,1.,0.866025403784439,1.,0.866025403784439,1.,0.866025403784439,
1.,0.866025403784439,1.,0.866025403784439,1.,0.866025403784439,1.,0.866025403784439,
1.,0.866025403784439,1.,0.866025403784439,1.,0.866025403784439,1.,0.866025403784439,
1.,0.866025403784439,1.,0.866025403784439,1.,0.866025403784439,1.,0.866025403784439,
1.,0.866025403784439,1.,0.866025403784439,1.,0.866025403784439,1.,0.866025403784439,
1.,0.866025403784439,1.,0.866025403784439,1.,0.866025403784439,1.,0.866025403784439,
1.,0.866025403784439,1.,0.866025403784439,1.,0.866025403784439,1.,0.866025403784439,
1.,0.866025403784439,1.,0.866025403784439,1.,0.866025403784439,1.,0.866025403784439,
1.,0.866025403784439,1.,0.866025403784439,1.,0.866025403784439,1.,0.866025403784439,
1.,0.866025403784439,1.,0.866025403784439,1.,0.866025403784439,1.,0.866025403784439,
1.,0.866025403784439,1.,0.866025403784439,1.,0.866025403784439,1.,0.866025403784439,
1.,0.866025403784439,1.,0.866025403784439,1.,0.866025403784439,1.,0.866025403784439,
1.,0.866025403784439,1.,0.866025403784439,1.,0.866025403784439,1.,0.866025403784439,
1.,0.866025403784439,1.,0.866025403784439,1.,0.866025403784439,1.,0.866025403784439,
1.,0.866025403784439,1.,0.866025403784439,1.,0.866025403784439,1.,0.866025403784439,
1.,0.866025403784439,1.,0.866025403784439,1.,0.866025403784439,1.,0.866025403784439,
1.,0.866025403784439,1.,0.866025403784439,1.,0.866025403784439,1.,0.866025403784439,
1.,0.866025403784439,1.,0.866025403784439,1.,0.866025403784439,1.,0.866025403784439,
1.,0.866025403784439,1.,0.866025403784439,1.,0.866025403784439,1.,0.866025403784439,
1.,0.866025403784439,1.,0.866025403784439,1.,0.866025403784439,1.,0.866025403784439,
1.,0.866025403784439,1.,0.866025403784439,1.,0.866025403784439,1.,0.866025403784439,
1.,0.866025403784439,1.,0.866025403784439,1.,0.866025403784439,1.,0.866025403784439,
1.,0.866025403784439,1.,0.866025403784439,1.,0.866025403784439,1.,0.866025403784439,
1.,0.866025403784439,1.,0.866025403784439,1.,0.866025403784439,1.,0.866025403784439,
1.,0.866025403784439,1.,0.866025403784439,1.,0.866025403784439,1.,0.866025403784439,
1.,0.866025403784439,1.,0.866025403784439,1.,0.866025403784439,1.,0.866025403784439,
1.,0.866025403784439,1.,0.866025403784439,1.,0.866025403784439,1.,0.866025403784439,
1.,0.866025403784439,1.,0.866025403784439,1.,0.866025403784439,1.,0.866025403784439,
1.,0.866025403784439,1.,0.866025403784439,1.,0.866025403784439,1.,0.866025403784439,
1.,0.866025403784439,1.,0.866025403784439,1.,0.866025403784439,1.,0.866025403784439,
1.,0.866025403784439,1.,0.866025403784439,1.,0.866025403784439,1.,0.866025403784439,
1.,0.866025403784439,1.,0.866025403784439,1.,0.939534597205461,0.933647674785266))
REPRESENTATION_ITEM('')
);
#197=(
BOUNDED_CURVE()
B_SPLINE_CURVE(2,(#21385,#21386,#21387,#21388,#21389,#21390,#21391,#21392,
#21393,#21394,#21395,#21396,#21397,#21398,#21399,#21400,#21401,#21402,#21403,
#21404,#21405,#21406,#21407,#21408,#21409,#21410,#21411,#21412,#21413,#21414,
#21415,#21416,#21417,#21418,#21419,#21420,#21421,#21422,#21423,#21424,#21425,
#21426,#21427,#21428,#21429,#21430,#21431,#21432,#21433,#21434,#21435,#21436,
#21437,#21438,#21439,#21440,#21441,#21442,#21443,#21444,#21445,#21446,#21447,
#21448,#21449,#21450,#21451,#21452,#21453,#21454,#21455,#21456,#21457,#21458,
#21459,#21460,#21461,#21462,#21463,#21464,#21465,#21466,#21467,#21468,#21469,
#21470,#21471,#21472,#21473,#21474,#21475,#21476,#21477,#21478,#21479,#21480,
#21481,#21482,#21483,#21484,#21485,#21486,#21487,#21488,#21489,#21490,#21491,
#21492,#21493,#21494,#21495,#21496,#21497,#21498,#21499,#21500,#21501,#21502,
#21503,#21504,#21505,#21506,#21507,#21508,#21509,#21510,#21511,#21512,#21513,
#21514,#21515,#21516,#21517,#21518,#21519,#21520,#21521,#21522,#21523,#21524,
#21525,#21526,#21527,#21528,#21529,#21530,#21531,#21532,#21533,#21534,#21535,
#21536,#21537,#21538,#21539,#21540,#21541,#21542,#21543,#21544,#21545,#21546,
#21547,#21548,#21549,#21550,#21551,#21552,#21553,#21554,#21555,#21556,#21557,
#21558,#21559,#21560,#21561,#21562,#21563,#21564,#21565,#21566,#21567,#21568,
#21569,#21570,#21571,#21572,#21573,#21574,#21575,#21576,#21577,#21578,#21579,
#21580,#21581,#21582,#21583,#21584,#21585,#21586,#21587,#21588,#21589,#21590,
#21591,#21592,#21593,#21594,#21595,#21596,#21597,#21598,#21599,#21600,#21601,
#21602,#21603,#21604,#21605,#21606,#21607,#21608,#21609,#21610,#21611,#21612,
#21613,#21614,#21615,#21616,#21617,#21618,#21619,#21620,#21621,#21622,#21623,
#21624,#21625,#21626,#21627,#21628,#21629,#21630,#21631,#21632,#21633,#21634,
#21635,#21636,#21637,#21638,#21639,#21640,#21641,#21642,#21643,#21644,#21645,
#21646,#21647,#21648,#21649,#21650,#21651,#21652,#21653,#21654,#21655,#21656,
#21657),.UNSPECIFIED.,.F.,.F.)
B_SPLINE_CURVE_WITH_KNOTS((3,2,2,2,2,2,2,2,2,2,2,2,2,2,2,2,2,2,2,2,2,2,
2,2,2,2,2,2,2,2,2,2,2,2,2,2,2,2,2,2,2,2,2,2,2,2,2,2,2,2,2,2,2,2,2,2,2,2,
2,2,2,2,2,2,2,2,2,2,2,2,2,2,2,2,2,2,2,2,2,2,2,2,2,2,2,2,2,2,2,2,2,2,2,2,
2,2,2,2,2,2,2,2,2,2,2,2,2,2,2,2,2,2,2,2,2,2,2,2,2,2,2,2,2,2,2,2,2,2,2,2,
2,2,2,2,2,2,3),(0.697234701114643,0.697530864197531,0.699588477366255,0.701646090534979,
0.703703703703704,0.705761316872428,0.707818930041152,0.709876543209877,
0.711934156378601,0.713991769547325,0.716049382716049,0.718106995884774,
0.720164609053498,0.722222222222222,0.724279835390947,0.726337448559671,
0.728395061728395,0.730452674897119,0.732510288065844,0.734567901234568,
0.736625514403292,0.738683127572016,0.740740740740741,0.742798353909465,
0.744855967078189,0.746913580246914,0.748971193415638,0.751028806584362,
0.753086419753086,0.755144032921811,0.757201646090535,0.759259259259259,
0.761316872427984,0.763374485596708,0.765432098765432,0.767489711934156,
0.769547325102881,0.771604938271605,0.773662551440329,0.775720164609053,
0.777777777777778,0.779835390946502,0.781893004115226,0.783950617283951,
0.786008230452675,0.788065843621399,0.790123456790123,0.792181069958848,
0.794238683127572,0.796296296296296,0.798353909465021,0.800411522633745,
0.802469135802469,0.804526748971193,0.806584362139918,0.808641975308642,
0.810699588477366,0.812757201646091,0.814814814814815,0.816872427983539,
0.818930041152263,0.820987654320988,0.823045267489712,0.825102880658436,
0.827160493827161,0.829218106995885,0.831275720164609,0.833333333333333,
0.835390946502058,0.837448559670782,0.839506172839506,0.84156378600823,
0.843621399176955,0.845679012345679,0.847736625514403,0.849794238683128,
0.851851851851852,0.853909465020576,0.8559670781893,0.858024691358025,0.860082304526749,
0.862139917695473,0.864197530864197,0.866255144032922,0.868312757201646,
0.87037037037037,0.872427983539095,0.874485596707819,0.876543209876543,
0.878600823045268,0.880658436213992,0.882716049382716,0.88477366255144,
0.886831275720165,0.888888888888889,0.890946502057613,0.893004115226337,
0.895061728395062,0.897119341563786,0.89917695473251,0.901234567901235,
0.903292181069959,0.905349794238683,0.907407407407407,0.909465020576132,
0.911522633744856,0.91358024691358,0.915637860082305,0.917695473251029,
0.919753086419753,0.921810699588477,0.923868312757202,0.925925925925926,
0.92798353909465,0.930041152263374,0.932098765432099,0.934156378600823,
0.936213991769547,0.938271604938272,0.940329218106996,0.94238683127572,
0.944444444444444,0.946502057613169,0.948559670781893,0.950617283950617,
0.952674897119342,0.954732510288066,0.95679012345679,0.958847736625514,
0.960905349794239,0.962962962962963,0.965020576131687,0.967078189300412,
0.969135802469136,0.97119341563786,0.973251028806584,0.974693312758157),
 .UNSPECIFIED.)
CURVE()
GEOMETRIC_REPRESENTATION_ITEM()
RATIONAL_B_SPLINE_CURVE((0.966983863280644,0.980716331890302,1.,0.866025403784439,
1.,0.866025403784439,1.,0.866025403784439,1.,0.866025403784439,1.,0.866025403784439,
1.,0.866025403784439,1.,0.866025403784439,1.,0.866025403784439,1.,0.866025403784439,
1.,0.866025403784439,1.,0.866025403784439,1.,0.866025403784439,1.,0.866025403784439,
1.,0.866025403784439,1.,0.866025403784439,1.,0.866025403784439,1.,0.866025403784439,
1.,0.866025403784439,1.,0.866025403784439,1.,0.866025403784439,1.,0.866025403784439,
1.,0.866025403784439,1.,0.866025403784439,1.,0.866025403784439,1.,0.866025403784439,
1.,0.866025403784439,1.,0.866025403784439,1.,0.866025403784439,1.,0.866025403784439,
1.,0.866025403784439,1.,0.866025403784439,1.,0.866025403784439,1.,0.866025403784439,
1.,0.866025403784439,1.,0.866025403784439,1.,0.866025403784439,1.,0.866025403784439,
1.,0.866025403784439,1.,0.866025403784439,1.,0.866025403784439,1.,0.866025403784439,
1.,0.866025403784439,1.,0.866025403784439,1.,0.866025403784439,1.,0.866025403784439,
1.,0.866025403784439,1.,0.866025403784439,1.,0.866025403784439,1.,0.866025403784439,
1.,0.866025403784439,1.,0.866025403784439,1.,0.866025403784439,1.,0.866025403784439,
1.,0.866025403784439,1.,0.866025403784439,1.,0.866025403784439,1.,0.866025403784439,
1.,0.866025403784439,1.,0.866025403784439,1.,0.866025403784439,1.,0.866025403784439,
1.,0.866025403784439,1.,0.866025403784439,1.,0.866025403784439,1.,0.866025403784439,
1.,0.866025403784439,1.,0.866025403784439,1.,0.866025403784439,1.,0.866025403784439,
1.,0.866025403784439,1.,0.866025403784439,1.,0.866025403784439,1.,0.866025403784439,
1.,0.866025403784439,1.,0.866025403784439,1.,0.866025403784439,1.,0.866025403784439,
1.,0.866025403784439,1.,0.866025403784439,1.,0.866025403784439,1.,0.866025403784439,
1.,0.866025403784439,1.,0.866025403784439,1.,0.866025403784439,1.,0.866025403784439,
1.,0.866025403784439,1.,0.866025403784439,1.,0.866025403784439,1.,0.866025403784439,
1.,0.866025403784439,1.,0.866025403784439,1.,0.866025403784439,1.,0.866025403784439,
1.,0.866025403784439,1.,0.866025403784439,1.,0.866025403784439,1.,0.866025403784439,
1.,0.866025403784439,1.,0.866025403784439,1.,0.866025403784439,1.,0.866025403784439,
1.,0.866025403784439,1.,0.866025403784439,1.,0.866025403784439,1.,0.866025403784439,
1.,0.866025403784439,1.,0.866025403784439,1.,0.866025403784439,1.,0.866025403784439,
1.,0.866025403784439,1.,0.866025403784439,1.,0.866025403784439,1.,0.866025403784439,
1.,0.866025403784439,1.,0.866025403784439,1.,0.866025403784439,1.,0.866025403784439,
1.,0.866025403784439,1.,0.866025403784439,1.,0.866025403784439,1.,0.866025403784439,
1.,0.866025403784439,1.,0.866025403784439,1.,0.866025403784439,1.,0.866025403784439,
1.,0.866025403784439,1.,0.866025403784439,1.,0.866025403784439,1.,0.866025403784439,
1.,0.866025403784439,1.,0.866025403784439,1.,0.866025403784439,1.,0.866025403784439,
1.,0.866025403784439,1.,0.906090506720528,0.94383273215671))
REPRESENTATION_ITEM('')
);
#198=(
BOUNDED_CURVE()
B_SPLINE_CURVE(2,(#28081,#28082,#28083),.UNSPECIFIED.,.F.,.F.)
B_SPLINE_CURVE_WITH_KNOTS((3,3),(-2.2693844624543,-1.90898280074518),
 .UNSPECIFIED.)
CURVE()
GEOMETRIC_REPRESENTATION_ITEM()
RATIONAL_B_SPLINE_CURVE((1.7477494971405,1.72129587968328,1.68438569901946))
REPRESENTATION_ITEM('')
);
#199=(
BOUNDED_CURVE()
B_SPLINE_CURVE(2,(#28084,#28085,#28086),.UNSPECIFIED.,.F.,.F.)
B_SPLINE_CURVE_WITH_KNOTS((3,3),(1.90898280074519,2.2693844624543),
 .UNSPECIFIED.)
CURVE()
GEOMETRIC_REPRESENTATION_ITEM()
RATIONAL_B_SPLINE_CURVE((1.68438569901946,1.72129587968328,1.7477494971405))
REPRESENTATION_ITEM('')
);
#200=(
BOUNDED_CURVE()
B_SPLINE_CURVE(2,(#30719,#30720,#30721,#30722,#30723,#30724,#30725,#30726,
#30727,#30728,#30729,#30730,#30731,#30732,#30733,#30734,#30735,#30736,#30737,
#30738,#30739,#30740,#30741,#30742,#30743,#30744,#30745,#30746,#30747,#30748,
#30749,#30750,#30751,#30752,#30753,#30754,#30755,#30756,#30757,#30758,#30759,
#30760,#30761,#30762,#30763,#30764,#30765,#30766,#30767,#30768,#30769,#30770,
#30771,#30772,#30773,#30774,#30775,#30776,#30777,#30778,#30779,#30780,#30781,
#30782,#30783,#30784,#30785,#30786,#30787,#30788,#30789,#30790,#30791,#30792,
#30793,#30794,#30795,#30796,#30797,#30798,#30799,#30800,#30801,#30802,#30803,
#30804,#30805,#30806,#30807,#30808,#30809,#30810,#30811,#30812,#30813,#30814,
#30815,#30816,#30817,#30818,#30819,#30820,#30821,#30822,#30823,#30824,#30825,
#30826,#30827,#30828,#30829,#30830,#30831,#30832,#30833,#30834,#30835,#30836,
#30837,#30838,#30839,#30840,#30841,#30842,#30843,#30844,#30845,#30846,#30847,
#30848,#30849,#30850,#30851,#30852,#30853,#30854,#30855,#30856,#30857,#30858,
#30859,#30860,#30861,#30862,#30863,#30864,#30865,#30866,#30867,#30868,#30869,
#30870,#30871,#30872,#30873,#30874,#30875,#30876,#30877,#30878,#30879,#30880,
#30881,#30882,#30883,#30884,#30885,#30886,#30887,#30888,#30889,#30890,#30891,
#30892,#30893,#30894,#30895,#30896,#30897,#30898,#30899,#30900,#30901,#30902,
#30903,#30904,#30905,#30906,#30907,#30908,#30909,#30910,#30911,#30912,#30913,
#30914,#30915,#30916,#30917,#30918,#30919,#30920,#30921,#30922,#30923,#30924,
#30925,#30926,#30927,#30928,#30929,#30930,#30931,#30932,#30933,#30934,#30935,
#30936,#30937,#30938,#30939,#30940,#30941,#30942,#30943,#30944,#30945,#30946,
#30947,#30948,#30949,#30950,#30951,#30952,#30953,#30954,#30955,#30956,#30957,
#30958,#30959,#30960,#30961,#30962,#30963,#30964,#30965,#30966,#30967,#30968,
#30969,#30970,#30971,#30972,#30973,#30974,#30975,#30976,#30977,#30978,#30979,
#30980,#30981,#30982,#30983,#30984,#30985,#30986,#30987,#30988,#30989,#30990,
#30991,#30992,#30993,#30994,#30995,#30996,#30997,#30998,#30999,#31000,#31001,
#31002,#31003,#31004,#31005,#31006,#31007,#31008,#31009,#31010,#31011,#31012,
#31013,#31014,#31015,#31016,#31017,#31018,#31019,#31020,#31021,#31022,#31023,
#31024,#31025,#31026,#31027,#31028,#31029,#31030,#31031,#31032,#31033,#31034,
#31035,#31036,#31037,#31038,#31039,#31040,#31041,#31042,#31043,#31044,#31045,
#31046,#31047,#31048,#31049,#31050,#31051,#31052,#31053,#31054,#31055,#31056,
#31057,#31058,#31059,#31060,#31061,#31062,#31063,#31064,#31065,#31066,#31067,
#31068,#31069,#31070,#31071,#31072,#31073,#31074,#31075,#31076,#31077,#31078,
#31079,#31080,#31081,#31082,#31083,#31084,#31085,#31086,#31087,#31088,#31089,
#31090,#31091,#31092,#31093,#31094,#31095,#31096,#31097,#31098,#31099,#31100,
#31101,#31102,#31103,#31104,#31105,#31106,#31107,#31108,#31109,#31110,#31111,
#31112,#31113,#31114,#31115,#31116,#31117,#31118,#31119,#31120,#31121,#31122,
#31123,#31124,#31125,#31126,#31127,#31128,#31129,#31130,#31131,#31132,#31133,
#31134,#31135,#31136,#31137,#31138,#31139,#31140,#31141,#31142,#31143,#31144,
#31145,#31146,#31147,#31148,#31149,#31150,#31151,#31152,#31153,#31154,#31155,
#31156,#31157,#31158,#31159,#31160,#31161,#31162,#31163,#31164,#31165,#31166,
#31167,#31168,#31169,#31170,#31171,#31172,#31173,#31174,#31175,#31176,#31177,
#31178,#31179,#31180,#31181,#31182,#31183,#31184,#31185,#31186,#31187,#31188,
#31189,#31190,#31191,#31192,#31193,#31194,#31195,#31196,#31197,#31198,#31199,
#31200,#31201,#31202,#31203,#31204,#31205,#31206,#31207,#31208,#31209,#31210,
#31211,#31212,#31213,#31214,#31215,#31216,#31217,#31218,#31219,#31220,#31221,
#31222,#31223,#31224,#31225,#31226,#31227,#31228,#31229,#31230,#31231,#31232,
#31233,#31234,#31235,#31236,#31237,#31238,#31239,#31240,#31241,#31242,#31243,
#31244,#31245,#31246,#31247,#31248,#31249,#31250,#31251,#31252,#31253,#31254,
#31255,#31256,#31257,#31258,#31259,#31260,#31261,#31262,#31263,#31264,#31265,
#31266,#31267,#31268,#31269,#31270,#31271,#31272,#31273,#31274,#31275,#31276,
#31277,#31278,#31279,#31280,#31281,#31282,#31283,#31284,#31285,#31286,#31287,
#31288,#31289,#31290,#31291,#31292,#31293,#31294,#31295,#31296,#31297,#31298,
#31299,#31300,#31301,#31302,#31303,#31304,#31305,#31306,#31307,#31308,#31309,
#31310,#31311,#31312,#31313,#31314,#31315,#31316,#31317,#31318,#31319,#31320,
#31321,#31322,#31323,#31324,#31325,#31326,#31327,#31328,#31329,#31330,#31331,
#31332,#31333,#31334,#31335,#31336,#31337,#31338,#31339,#31340,#31341,#31342,
#31343,#31344,#31345,#31346,#31347,#31348,#31349,#31350,#31351,#31352,#31353,
#31354,#31355,#31356,#31357,#31358,#31359,#31360,#31361,#31362,#31363,#31364,
#31365,#31366,#31367,#31368,#31369,#31370,#31371,#31372,#31373,#31374,#31375,
#31376,#31377,#31378,#31379,#31380,#31381,#31382,#31383,#31384,#31385,#31386,
#31387,#31388,#31389,#31390,#31391,#31392,#31393,#31394,#31395,#31396,#31397,
#31398,#31399,#31400,#31401,#31402,#31403,#31404,#31405,#31406,#31407,#31408,
#31409,#31410,#31411,#31412,#31413,#31414,#31415,#31416,#31417,#31418,#31419,
#31420,#31421,#31422,#31423,#31424,#31425,#31426,#31427,#31428,#31429,#31430,
#31431,#31432,#31433,#31434,#31435,#31436,#31437,#31438,#31439,#31440,#31441,
#31442,#31443,#31444,#31445,#31446,#31447,#31448,#31449,#31450,#31451,#31452,
#31453,#31454,#31455,#31456,#31457,#31458,#31459,#31460,#31461,#31462,#31463,
#31464,#31465,#31466,#31467,#31468,#31469,#31470,#31471,#31472,#31473,#31474,
#31475,#31476,#31477,#31478,#31479,#31480,#31481,#31482,#31483,#31484,#31485,
#31486,#31487,#31488,#31489,#31490,#31491,#31492,#31493,#31494,#31495,#31496,
#31497,#31498,#31499,#31500,#31501,#31502,#31503,#31504,#31505,#31506,#31507,
#31508,#31509,#31510,#31511,#31512,#31513,#31514,#31515,#31516,#31517,#31518,
#31519,#31520,#31521,#31522,#31523,#31524,#31525,#31526,#31527,#31528,#31529,
#31530,#31531,#31532,#31533,#31534,#31535,#31536,#31537,#31538,#31539,#31540,
#31541,#31542,#31543,#31544,#31545,#31546,#31547,#31548,#31549,#31550,#31551,
#31552,#31553,#31554,#31555,#31556,#31557,#31558,#31559,#31560,#31561,#31562,
#31563,#31564,#31565,#31566,#31567,#31568,#31569,#31570,#31571,#31572,#31573,
#31574,#31575,#31576,#31577,#31578,#31579,#31580,#31581,#31582,#31583,#31584,
#31585,#31586,#31587,#31588,#31589,#31590,#31591,#31592,#31593,#31594,#31595,
#31596,#31597,#31598,#31599,#31600,#31601,#31602,#31603,#31604,#31605,#31606,
#31607,#31608,#31609,#31610,#31611,#31612,#31613,#31614,#31615,#31616,#31617,
#31618,#31619,#31620,#31621,#31622,#31623,#31624,#31625,#31626,#31627,#31628,
#31629,#31630,#31631,#31632,#31633,#31634,#31635,#31636,#31637,#31638,#31639,
#31640,#31641,#31642,#31643,#31644,#31645,#31646,#31647,#31648,#31649,#31650,
#31651,#31652,#31653,#31654,#31655,#31656,#31657,#31658,#31659,#31660,#31661,
#31662,#31663,#31664,#31665),.UNSPECIFIED.,.F.,.F.)
B_SPLINE_CURVE_WITH_KNOTS((3,2,2,2,2,2,2,2,2,2,2,2,2,2,2,2,2,2,2,2,2,2,
2,2,2,2,2,2,2,2,2,2,2,2,2,2,2,2,2,2,2,2,2,2,2,2,2,2,2,2,2,2,2,2,2,2,2,2,
2,2,2,2,2,2,2,2,2,2,2,2,2,2,2,2,2,2,2,2,2,2,2,2,2,2,2,2,2,2,2,2,2,2,2,2,
2,2,2,2,2,2,2,2,2,2,2,2,2,2,2,2,2,2,2,2,2,2,2,2,2,2,2,2,2,2,2,2,2,2,2,2,
2,2,2,2,2,2,2,2,2,2,2,2,2,2,2,2,2,2,2,2,2,2,2,2,2,2,2,2,2,2,2,2,2,2,2,2,
2,2,2,2,2,2,2,2,2,2,2,2,2,2,2,2,2,2,2,2,2,2,2,2,2,2,2,2,2,2,2,2,2,2,2,2,
2,2,2,2,2,2,2,2,2,2,2,2,2,2,2,2,2,2,2,2,2,2,2,2,2,2,2,2,2,2,2,2,2,2,2,2,
2,2,2,2,2,2,2,2,2,2,2,2,2,2,2,2,2,2,2,2,2,2,2,2,2,2,2,2,2,2,2,2,2,2,2,2,
2,2,2,2,2,2,2,2,2,2,2,2,2,2,2,2,2,2,2,2,2,2,2,2,2,2,2,2,2,2,2,2,2,2,2,2,
2,2,2,2,2,2,2,2,2,2,2,2,2,2,2,2,2,2,2,2,2,2,2,2,2,2,2,2,2,2,2,2,2,2,2,2,
2,2,2,2,2,2,2,2,2,2,2,2,2,2,2,2,2,2,2,2,2,2,2,2,2,2,2,2,2,2,2,2,2,2,2,2,
2,2,2,2,2,2,2,2,2,2,2,2,2,2,2,2,2,2,2,2,2,2,2,2,2,2,2,2,2,2,2,2,2,2,2,2,
2,2,2,2,2,2,2,2,2,2,2,2,2,2,2,2,2,2,2,2,2,2,2,2,2,2,2,2,2,2,2,2,2,2,2,2,
2,2,2,2,2,2,2,2,2,2,2,2,2,2,2,2,2,2,2,3),(0.00769788512143581,0.00823045267489712,
0.0102880658436214,0.0123456790123457,0.01440329218107,0.0164609053497942,
0.0185185185185185,0.0205761316872428,0.0226337448559671,0.0246913580246914,
0.0267489711934156,0.0288065843621399,0.0308641975308642,0.0329218106995885,
0.0349794238683128,0.037037037037037,0.0390946502057613,0.0411522633744856,
0.0432098765432099,0.0452674897119342,0.0473251028806584,0.0493827160493827,
0.051440329218107,0.0534979423868313,0.0555555555555556,0.0576131687242798,
0.0596707818930041,0.0617283950617284,0.0637860082304527,0.065843621399177,
0.0679012345679012,0.0699588477366255,0.0720164609053498,0.0740740740740741,
0.0761316872427984,0.0781893004115226,0.0802469135802469,0.0823045267489712,
0.0843621399176955,0.0864197530864197,0.088477366255144,0.0905349794238683,
0.0925925925925926,0.0946502057613169,0.0967078189300412,0.0987654320987654,
0.10082304526749,0.102880658436214,0.104938271604938,0.106995884773663,
0.109053497942387,0.111111111111111,0.113168724279835,0.11522633744856,
0.117283950617284,0.119341563786008,0.121399176954733,0.123456790123457,
0.125514403292181,0.127572016460905,0.12962962962963,0.131687242798354,
0.133744855967078,0.135802469135802,0.137860082304527,0.139917695473251,
0.141975308641975,0.1440329218107,0.146090534979424,0.148148148148148,0.150205761316872,
0.152263374485597,0.154320987654321,0.156378600823045,0.15843621399177,
0.160493827160494,0.162551440329218,0.164609053497942,0.166666666666667,
0.168724279835391,0.170781893004115,0.172839506172839,0.174897119341564,
0.176954732510288,0.179012345679012,0.181069958847737,0.183127572016461,
0.185185185185185,0.18724279835391,0.189300411522634,0.191358024691358,
0.193415637860082,0.195473251028807,0.197530864197531,0.199588477366255,
0.201646090534979,0.203703703703704,0.205761316872428,0.207818930041152,
0.209876543209877,0.211934156378601,0.213991769547325,0.216049382716049,
0.218106995884774,0.220164609053498,0.222222222222222,0.224279835390947,
0.226337448559671,0.228395061728395,0.230452674897119,0.232510288065844,
0.234567901234568,0.236625514403292,0.238683127572016,0.240740740740741,
0.242798353909465,0.244855967078189,0.246913580246914,0.248971193415638,
0.251028806584362,0.253086419753086,0.255144032921811,0.257201646090535,
0.259259259259259,0.261316872427984,0.263374485596708,0.265432098765432,
0.267489711934156,0.269547325102881,0.271604938271605,0.273662551440329,
0.275720164609054,0.277777777777778,0.279835390946502,0.281893004115226,
0.283950617283951,0.286008230452675,0.288065843621399,0.290123456790123,
0.292181069958848,0.294238683127572,0.296296296296296,0.298353909465021,
0.300411522633745,0.302469135802469,0.304526748971193,0.306584362139918,
0.308641975308642,0.310699588477366,0.312757201646091,0.314814814814815,
0.316872427983539,0.318930041152263,0.320987654320988,0.323045267489712,
0.325102880658436,0.327160493827161,0.329218106995885,0.331275720164609,
0.333333333333333,0.335390946502058,0.337448559670782,0.339506172839506,
0.34156378600823,0.343621399176955,0.345679012345679,0.347736625514403,
0.349794238683128,0.351851851851852,0.353909465020576,0.3559670781893,0.358024691358025,
0.360082304526749,0.362139917695473,0.364197530864198,0.366255144032922,
0.368312757201646,0.37037037037037,0.372427983539095,0.374485596707819,
0.376543209876543,0.378600823045267,0.380658436213992,0.382716049382716,
0.38477366255144,0.386831275720165,0.388888888888889,0.390946502057613,
0.393004115226337,0.395061728395062,0.397119341563786,0.39917695473251,
0.401234567901235,0.403292181069959,0.405349794238683,0.407407407407407,
0.409465020576132,0.411522633744856,0.41358024691358,0.415637860082305,
0.417695473251029,0.419753086419753,0.421810699588477,0.423868312757202,
0.425925925925926,0.42798353909465,0.430041152263374,0.432098765432099,
0.434156378600823,0.436213991769547,0.438271604938272,0.440329218106996,
0.44238683127572,0.444444444444444,0.446502057613169,0.448559670781893,
0.450617283950617,0.452674897119342,0.454732510288066,0.45679012345679,
0.458847736625514,0.460905349794239,0.462962962962963,0.465020576131687,
0.467078189300412,0.469135802469136,0.47119341563786,0.473251028806584,
0.475308641975309,0.477366255144033,0.479423868312757,0.481481481481481,
0.483539094650206,0.48559670781893,0.487654320987654,0.489711934156379,
0.491769547325103,0.493827160493827,0.495884773662551,0.497942386831276,
0.5,0.502057613168724,0.504115226337449,0.506172839506173,0.508230452674897,
0.510288065843621,0.512345679012346,0.51440329218107,0.516460905349794,
0.518518518518518,0.520576131687243,0.522633744855967,0.524691358024691,
0.526748971193416,0.52880658436214,0.530864197530864,0.532921810699588,
0.534979423868313,0.537037037037037,0.539094650205761,0.541152263374486,
0.54320987654321,0.545267489711934,0.547325102880658,0.549382716049383,
0.551440329218107,0.553497942386831,0.555555555555556,0.55761316872428,
0.559670781893004,0.561728395061728,0.563786008230453,0.565843621399177,
0.567901234567901,0.569958847736626,0.57201646090535,0.574074074074074,
0.576131687242798,0.578189300411523,0.580246913580247,0.582304526748971,
0.584362139917695,0.58641975308642,0.588477366255144,0.590534979423868,
0.592592592592593,0.594650205761317,0.596707818930041,0.598765432098765,
0.60082304526749,0.602880658436214,0.604938271604938,0.606995884773663,
0.609053497942387,0.611111111111111,0.613168724279835,0.61522633744856,
0.617283950617284,0.619341563786008,0.621399176954732,0.623456790123457,
0.625514403292181,0.627572016460905,0.62962962962963,0.631687242798354,
0.633744855967078,0.635802469135803,0.637860082304527,0.639917695473251,
0.641975308641975,0.6440329218107,0.646090534979424,0.648148148148148,0.650205761316872,
0.652263374485597,0.654320987654321,0.656378600823045,0.65843621399177,
0.660493827160494,0.662551440329218,0.664609053497942,0.666666666666667,
0.668724279835391,0.670781893004115,0.672839506172839,0.674897119341564,
0.676954732510288,0.679012345679012,0.681069958847737,0.683127572016461,
0.685185185185185,0.687242798353909,0.689300411522634,0.691358024691358,
0.693415637860082,0.695473251028807,0.697530864197531,0.699588477366255,
0.70164609053498,0.703703703703704,0.705761316872428,0.707818930041152,
0.709876543209877,0.711934156378601,0.713991769547325,0.716049382716049,
0.718106995884774,0.720164609053498,0.722222222222222,0.724279835390947,
0.726337448559671,0.728395061728395,0.730452674897119,0.732510288065844,
0.734567901234568,0.736625514403292,0.738683127572016,0.740740740740741,
0.742798353909465,0.744855967078189,0.746913580246914,0.748971193415638,
0.751028806584362,0.753086419753086,0.755144032921811,0.757201646090535,
0.759259259259259,0.761316872427984,0.763374485596708,0.765432098765432,
0.767489711934156,0.769547325102881,0.771604938271605,0.773662551440329,
0.775720164609053,0.777777777777778,0.779835390946502,0.781893004115226,
0.783950617283951,0.786008230452675,0.788065843621399,0.790123456790123,
0.792181069958848,0.794238683127572,0.796296296296296,0.798353909465021,
0.800411522633745,0.802469135802469,0.804526748971193,0.806584362139918,
0.808641975308642,0.810699588477366,0.812757201646091,0.814814814814815,
0.816872427983539,0.818930041152263,0.820987654320988,0.823045267489712,
0.825102880658436,0.827160493827161,0.829218106995885,0.831275720164609,
0.833333333333333,0.835390946502058,0.837448559670782,0.839506172839506,
0.84156378600823,0.843621399176955,0.845679012345679,0.847736625514403,
0.849794238683128,0.851851851851852,0.853909465020576,0.8559670781893,0.858024691358025,
0.860082304526749,0.862139917695473,0.864197530864197,0.866255144032922,
0.868312757201646,0.87037037037037,0.872427983539095,0.874485596707819,
0.876543209876543,0.878600823045268,0.880658436213992,0.882716049382716,
0.88477366255144,0.886831275720165,0.888888888888889,0.890946502057613,
0.893004115226337,0.895061728395062,0.897119341563786,0.89917695473251,
0.901234567901235,0.903292181069959,0.905349794238683,0.907407407407407,
0.909465020576132,0.911522633744856,0.91358024691358,0.915637860082305,
0.917695473251029,0.919753086419753,0.921810699588477,0.923868312757202,
0.925925925925926,0.92798353909465,0.930041152263374,0.932098765432099,
0.934156378600823,0.936213991769547,0.938271604938272,0.940329218106996,
0.94238683127572,0.944444444444444,0.946502057613169,0.948559670781893,
0.950617283950617,0.952674897119342,0.954732510288066,0.95679012345679,
0.958847736625514,0.960905349794239,0.962962962962963,0.965020576131687,
0.967078189300412,0.969135802469136,0.97119341563786,0.973251028806584,
0.975308641975309,0.977366255144033,0.977769992664587),.UNSPECIFIED.)
CURVE()
GEOMETRIC_REPRESENTATION_ITEM()
RATIONAL_B_SPLINE_CURVE((0.948597702769161,0.96532364585481,1.,0.866025403784439,
1.,0.866025403784439,1.,0.866025403784439,1.,0.866025403784439,1.,0.866025403784439,
1.,0.866025403784439,1.,0.866025403784439,1.,0.866025403784439,1.,0.866025403784439,
1.,0.866025403784439,1.,0.866025403784439,1.,0.866025403784439,1.,0.866025403784439,
1.,0.866025403784439,1.,0.866025403784439,1.,0.866025403784439,1.,0.866025403784439,
1.,0.866025403784439,1.,0.866025403784439,1.,0.866025403784439,1.,0.866025403784439,
1.,0.866025403784439,1.,0.866025403784439,1.,0.866025403784439,1.,0.866025403784439,
1.,0.866025403784439,1.,0.866025403784439,1.,0.866025403784439,1.,0.866025403784439,
1.,0.866025403784439,1.,0.866025403784439,1.,0.866025403784439,1.,0.866025403784439,
1.,0.866025403784439,1.,0.866025403784439,1.,0.866025403784439,1.,0.866025403784439,
1.,0.866025403784439,1.,0.866025403784439,1.,0.866025403784439,1.,0.866025403784439,
1.,0.866025403784439,1.,0.866025403784439,1.,0.866025403784439,1.,0.866025403784439,
1.,0.866025403784439,1.,0.866025403784439,1.,0.866025403784439,1.,0.866025403784439,
1.,0.866025403784439,1.,0.866025403784439,1.,0.866025403784439,1.,0.866025403784439,
1.,0.866025403784439,1.,0.866025403784439,1.,0.866025403784439,1.,0.866025403784439,
1.,0.866025403784439,1.,0.866025403784439,1.,0.866025403784439,1.,0.866025403784439,
1.,0.866025403784439,1.,0.866025403784439,1.,0.866025403784439,1.,0.866025403784439,
1.,0.866025403784439,1.,0.866025403784439,1.,0.866025403784439,1.,0.866025403784439,
1.,0.866025403784439,1.,0.866025403784439,1.,0.866025403784439,1.,0.866025403784439,
1.,0.866025403784439,1.,0.866025403784439,1.,0.866025403784439,1.,0.866025403784439,
1.,0.866025403784439,1.,0.866025403784439,1.,0.866025403784439,1.,0.866025403784439,
1.,0.866025403784439,1.,0.866025403784439,1.,0.866025403784439,1.,0.866025403784439,
1.,0.866025403784439,1.,0.866025403784439,1.,0.866025403784439,1.,0.866025403784439,
1.,0.866025403784439,1.,0.866025403784439,1.,0.866025403784439,1.,0.866025403784439,
1.,0.866025403784439,1.,0.866025403784439,1.,0.866025403784439,1.,0.866025403784439,
1.,0.866025403784439,1.,0.866025403784439,1.,0.866025403784439,1.,0.866025403784439,
1.,0.866025403784439,1.,0.866025403784439,1.,0.866025403784439,1.,0.866025403784439,
1.,0.866025403784439,1.,0.866025403784439,1.,0.866025403784439,1.,0.866025403784439,
1.,0.866025403784439,1.,0.866025403784439,1.,0.866025403784439,1.,0.866025403784439,
1.,0.866025403784439,1.,0.866025403784439,1.,0.866025403784439,1.,0.866025403784439,
1.,0.866025403784439,1.,0.866025403784439,1.,0.866025403784439,1.,0.866025403784439,
1.,0.866025403784439,1.,0.866025403784439,1.,0.866025403784439,1.,0.866025403784439,
1.,0.866025403784439,1.,0.866025403784439,1.,0.866025403784439,1.,0.866025403784439,
1.,0.866025403784439,1.,0.866025403784439,1.,0.866025403784439,1.,0.866025403784439,
1.,0.866025403784439,1.,0.866025403784439,1.,0.866025403784439,1.,0.866025403784439,
1.,0.866025403784439,1.,0.866025403784439,1.,0.866025403784439,1.,0.866025403784439,
1.,0.866025403784439,1.,0.866025403784439,1.,0.866025403784439,1.,0.866025403784439,
1.,0.866025403784439,1.,0.866025403784439,1.,0.866025403784439,1.,0.866025403784439,
1.,0.866025403784439,1.,0.866025403784439,1.,0.866025403784439,1.,0.866025403784439,
1.,0.866025403784439,1.,0.866025403784439,1.,0.866025403784439,1.,0.866025403784439,
1.,0.866025403784439,1.,0.866025403784439,1.,0.866025403784439,1.,0.866025403784439,
1.,0.866025403784439,1.,0.866025403784439,1.,0.866025403784439,1.,0.866025403784439,
1.,0.866025403784439,1.,0.866025403784439,1.,0.866025403784439,1.,0.866025403784439,
1.,0.866025403784439,1.,0.866025403784439,1.,0.866025403784439,1.,0.866025403784439,
1.,0.866025403784439,1.,0.866025403784439,1.,0.866025403784439,1.,0.866025403784439,
1.,0.866025403784439,1.,0.866025403784439,1.,0.866025403784439,1.,0.866025403784439,
1.,0.866025403784439,1.,0.866025403784439,1.,0.866025403784439,1.,0.866025403784439,
1.,0.866025403784439,1.,0.866025403784439,1.,0.866025403784439,1.,0.866025403784439,
1.,0.866025403784439,1.,0.866025403784439,1.,0.866025403784439,1.,0.866025403784439,
1.,0.866025403784439,1.,0.866025403784439,1.,0.866025403784439,1.,0.866025403784439,
1.,0.866025403784439,1.,0.866025403784439,1.,0.866025403784439,1.,0.866025403784439,
1.,0.866025403784439,1.,0.866025403784439,1.,0.866025403784439,1.,0.866025403784439,
1.,0.866025403784439,1.,0.866025403784439,1.,0.866025403784439,1.,0.866025403784439,
1.,0.866025403784439,1.,0.866025403784439,1.,0.866025403784439,1.,0.866025403784439,
1.,0.866025403784439,1.,0.866025403784439,1.,0.866025403784439,1.,0.866025403784439,
1.,0.866025403784439,1.,0.866025403784439,1.,0.866025403784439,1.,0.866025403784439,
1.,0.866025403784439,1.,0.866025403784439,1.,0.866025403784439,1.,0.866025403784439,
1.,0.866025403784439,1.,0.866025403784439,1.,0.866025403784439,1.,0.866025403784439,
1.,0.866025403784439,1.,0.866025403784439,1.,0.866025403784439,1.,0.866025403784439,
1.,0.866025403784439,1.,0.866025403784439,1.,0.866025403784439,1.,0.866025403784439,
1.,0.866025403784439,1.,0.866025403784439,1.,0.866025403784439,1.,0.866025403784439,
1.,0.866025403784439,1.,0.866025403784439,1.,0.866025403784439,1.,0.866025403784439,
1.,0.866025403784439,1.,0.866025403784439,1.,0.866025403784439,1.,0.866025403784439,
1.,0.866025403784439,1.,0.866025403784439,1.,0.866025403784439,1.,0.866025403784439,
1.,0.866025403784439,1.,0.866025403784439,1.,0.866025403784439,1.,0.866025403784439,
1.,0.866025403784439,1.,0.866025403784439,1.,0.866025403784439,1.,0.866025403784439,
1.,0.866025403784439,1.,0.866025403784439,1.,0.866025403784439,1.,0.866025403784439,
1.,0.866025403784439,1.,0.866025403784439,1.,0.866025403784439,1.,0.866025403784439,
1.,0.866025403784439,1.,0.866025403784439,1.,0.866025403784439,1.,0.866025403784439,
1.,0.866025403784439,1.,0.866025403784439,1.,0.866025403784439,1.,0.866025403784439,
1.,0.866025403784439,1.,0.866025403784439,1.,0.866025403784439,1.,0.866025403784439,
1.,0.866025403784439,1.,0.866025403784439,1.,0.866025403784439,1.,0.866025403784439,
1.,0.866025403784439,1.,0.866025403784439,1.,0.866025403784439,1.,0.866025403784439,
1.,0.866025403784439,1.,0.866025403784439,1.,0.866025403784439,1.,0.866025403784439,
1.,0.866025403784439,1.,0.866025403784439,1.,0.866025403784439,1.,0.866025403784439,
1.,0.866025403784439,1.,0.866025403784439,1.,0.866025403784439,1.,0.866025403784439,
1.,0.866025403784439,1.,0.866025403784439,1.,0.866025403784439,1.,0.866025403784439,
1.,0.866025403784439,1.,0.866025403784439,1.,0.866025403784439,1.,0.866025403784439,
1.,0.866025403784439,1.,0.866025403784439,1.,0.866025403784439,1.,0.866025403784439,
1.,0.866025403784439,1.,0.866025403784439,1.,0.866025403784439,1.,0.866025403784439,
1.,0.866025403784439,1.,0.866025403784439,1.,0.866025403784439,1.,0.866025403784439,
1.,0.866025403784439,1.,0.866025403784439,1.,0.866025403784439,1.,0.866025403784439,
1.,0.866025403784439,1.,0.866025403784439,1.,0.866025403784439,1.,0.866025403784439,
1.,0.866025403784439,1.,0.866025403784439,1.,0.866025403784439,1.,0.866025403784439,
1.,0.866025403784439,1.,0.866025403784439,1.,0.866025403784439,1.,0.866025403784439,
1.,0.866025403784439,1.,0.866025403784439,1.,0.866025403784439,1.,0.866025403784439,
1.,0.866025403784439,1.,0.866025403784439,1.,0.866025403784439,1.,0.866025403784439,
1.,0.866025403784439,1.,0.866025403784439,1.,0.866025403784439,1.,0.866025403784439,
1.,0.866025403784439,1.,0.866025403784439,1.,0.866025403784439,1.,0.866025403784439,
1.,0.866025403784439,1.,0.866025403784439,1.,0.866025403784439,1.,0.866025403784439,
1.,0.866025403784439,1.,0.866025403784439,1.,0.866025403784439,1.,0.866025403784439,
1.,0.866025403784439,1.,0.866025403784439,1.,0.866025403784439,1.,0.866025403784439,
1.,0.866025403784439,1.,0.866025403784439,1.,0.866025403784439,1.,0.866025403784439,
1.,0.866025403784439,1.,0.866025403784439,1.,0.866025403784439,1.,0.866025403784439,
1.,0.866025403784439,1.,0.866025403784439,1.,0.866025403784439,1.,0.866025403784439,
1.,0.866025403784439,1.,0.866025403784439,1.,0.866025403784439,1.,0.866025403784439,
1.,0.866025403784439,1.,0.866025403784439,1.,0.866025403784439,1.,0.866025403784439,
1.,0.866025403784439,1.,0.866025403784439,1.,0.866025403784439,1.,0.866025403784439,
1.,0.866025403784439,1.,0.866025403784439,1.,0.866025403784439,1.,0.866025403784439,
1.,0.866025403784439,1.,0.866025403784439,1.,0.866025403784439,1.,0.866025403784439,
1.,0.866025403784439,1.,0.866025403784439,1.,0.866025403784439,1.,0.866025403784439,
1.,0.866025403784439,1.,0.866025403784439,1.,0.866025403784439,1.,0.866025403784439,
1.,0.866025403784439,1.,0.866025403784439,1.,0.866025403784439,1.,0.866025403784439,
1.,0.866025403784439,1.,0.866025403784439,1.,0.866025403784439,1.,0.866025403784439,
1.,0.866025403784439,1.,0.866025403784439,1.,0.866025403784439,1.,0.866025403784439,
1.,0.866025403784439,1.,0.866025403784439,1.,0.866025403784439,1.,0.866025403784439,
1.,0.866025403784439,1.,0.866025403784439,1.,0.866025403784439,1.,0.866025403784439,
1.,0.866025403784439,1.,0.866025403784439,1.,0.866025403784439,1.,0.866025403784439,
1.,0.866025403784439,1.,0.866025403784439,1.,0.866025403784439,1.,0.866025403784439,
1.,0.866025403784439,1.,0.866025403784439,1.,0.866025403784439,1.,0.866025403784439,
1.,0.866025403784439,1.,0.866025403784439,1.,0.866025403784439,1.,0.866025403784439,
1.,0.866025403784439,1.,0.866025403784439,1.,0.866025403784439,1.,0.866025403784439,
1.,0.866025403784439,1.,0.866025403784439,1.,0.866025403784439,1.,0.866025403784439,
1.,0.866025403784439,1.,0.866025403784439,1.,0.866025403784439,1.,0.866025403784439,
1.,0.866025403784439,1.,0.866025403784439,1.,0.866025403784439,1.,0.866025403784439,
1.,0.866025403784439,1.,0.866025403784439,1.,0.866025403784439,1.,0.866025403784439,
1.,0.866025403784439,1.,0.866025403784439,1.,0.866025403784439,1.,0.866025403784439,
1.,0.866025403784439,1.,0.866025403784439,1.,0.866025403784439,1.,0.866025403784439,
1.,0.866025403784439,1.,0.866025403784439,1.,0.973711982351429,0.957740246914744))
REPRESENTATION_ITEM('')
);
#201=(
BOUNDED_CURVE()
B_SPLINE_CURVE(2,(#31683,#31684,#31685,#31686,#31687,#31688,#31689,#31690,
#31691,#31692,#31693,#31694,#31695,#31696,#31697,#31698,#31699,#31700,#31701,
#31702,#31703,#31704,#31705,#31706,#31707,#31708,#31709,#31710,#31711,#31712,
#31713,#31714,#31715,#31716,#31717,#31718,#31719,#31720,#31721,#31722,#31723,
#31724,#31725,#31726,#31727,#31728,#31729,#31730,#31731,#31732,#31733,#31734,
#31735,#31736,#31737,#31738,#31739,#31740,#31741,#31742,#31743,#31744,#31745,
#31746,#31747,#31748,#31749,#31750,#31751,#31752,#31753,#31754,#31755,#31756,
#31757,#31758,#31759,#31760,#31761,#31762,#31763,#31764,#31765,#31766,#31767,
#31768,#31769,#31770,#31771,#31772,#31773,#31774,#31775,#31776,#31777,#31778,
#31779,#31780,#31781,#31782,#31783,#31784,#31785,#31786,#31787,#31788,#31789,
#31790,#31791,#31792,#31793,#31794,#31795,#31796,#31797,#31798,#31799,#31800,
#31801,#31802,#31803,#31804,#31805,#31806,#31807,#31808,#31809,#31810,#31811,
#31812,#31813,#31814,#31815,#31816,#31817,#31818,#31819,#31820,#31821,#31822,
#31823,#31824,#31825,#31826,#31827,#31828,#31829,#31830,#31831,#31832,#31833,
#31834,#31835,#31836,#31837,#31838,#31839,#31840,#31841,#31842,#31843,#31844,
#31845,#31846,#31847,#31848,#31849,#31850,#31851,#31852,#31853,#31854,#31855,
#31856,#31857,#31858,#31859,#31860,#31861,#31862,#31863,#31864,#31865,#31866,
#31867,#31868,#31869,#31870,#31871,#31872,#31873,#31874,#31875,#31876,#31877,
#31878,#31879,#31880,#31881,#31882,#31883,#31884,#31885,#31886,#31887,#31888,
#31889,#31890,#31891,#31892,#31893,#31894,#31895,#31896,#31897,#31898,#31899,
#31900,#31901,#31902,#31903,#31904,#31905,#31906,#31907,#31908,#31909,#31910,
#31911,#31912,#31913,#31914,#31915,#31916,#31917,#31918,#31919,#31920,#31921,
#31922,#31923,#31924,#31925,#31926,#31927,#31928,#31929,#31930,#31931,#31932,
#31933,#31934,#31935,#31936,#31937,#31938,#31939,#31940,#31941,#31942,#31943,
#31944,#31945,#31946,#31947,#31948,#31949,#31950,#31951,#31952,#31953,#31954,
#31955,#31956,#31957,#31958,#31959,#31960,#31961,#31962,#31963,#31964,#31965,
#31966,#31967,#31968,#31969,#31970,#31971,#31972,#31973,#31974,#31975,#31976,
#31977,#31978,#31979,#31980,#31981,#31982,#31983,#31984,#31985,#31986,#31987,
#31988,#31989,#31990,#31991,#31992,#31993,#31994,#31995,#31996,#31997,#31998,
#31999,#32000,#32001,#32002,#32003,#32004,#32005,#32006,#32007,#32008,#32009,
#32010,#32011,#32012,#32013,#32014,#32015,#32016,#32017,#32018,#32019,#32020,
#32021,#32022,#32023,#32024,#32025,#32026,#32027,#32028,#32029,#32030,#32031,
#32032,#32033,#32034,#32035,#32036,#32037,#32038,#32039,#32040,#32041,#32042,
#32043,#32044,#32045,#32046,#32047,#32048,#32049,#32050,#32051,#32052,#32053,
#32054,#32055,#32056,#32057,#32058,#32059,#32060,#32061,#32062,#32063,#32064,
#32065,#32066,#32067,#32068,#32069,#32070,#32071,#32072,#32073,#32074,#32075,
#32076,#32077,#32078,#32079,#32080,#32081,#32082,#32083,#32084,#32085,#32086,
#32087,#32088,#32089,#32090,#32091,#32092,#32093,#32094,#32095,#32096,#32097,
#32098,#32099,#32100,#32101,#32102,#32103,#32104,#32105,#32106,#32107,#32108,
#32109,#32110,#32111,#32112,#32113,#32114,#32115,#32116,#32117,#32118,#32119,
#32120,#32121,#32122,#32123,#32124,#32125,#32126,#32127,#32128,#32129,#32130,
#32131,#32132,#32133,#32134,#32135,#32136,#32137,#32138,#32139,#32140,#32141,
#32142,#32143,#32144,#32145,#32146,#32147,#32148,#32149,#32150,#32151,#32152,
#32153,#32154,#32155,#32156,#32157,#32158,#32159,#32160,#32161,#32162,#32163,
#32164,#32165,#32166,#32167,#32168,#32169,#32170,#32171,#32172,#32173,#32174,
#32175,#32176,#32177,#32178,#32179,#32180,#32181,#32182,#32183,#32184,#32185,
#32186,#32187,#32188,#32189,#32190,#32191,#32192,#32193,#32194,#32195,#32196,
#32197,#32198,#32199,#32200,#32201,#32202,#32203,#32204,#32205,#32206,#32207,
#32208,#32209,#32210,#32211,#32212,#32213,#32214,#32215,#32216,#32217,#32218,
#32219,#32220,#32221,#32222,#32223,#32224,#32225,#32226,#32227,#32228,#32229,
#32230,#32231,#32232,#32233,#32234,#32235,#32236,#32237,#32238,#32239,#32240,
#32241,#32242,#32243,#32244,#32245,#32246,#32247,#32248,#32249,#32250,#32251,
#32252,#32253,#32254,#32255,#32256,#32257,#32258,#32259,#32260,#32261,#32262,
#32263,#32264,#32265,#32266,#32267,#32268,#32269,#32270,#32271,#32272,#32273,
#32274,#32275,#32276,#32277,#32278,#32279,#32280,#32281,#32282,#32283,#32284,
#32285,#32286,#32287,#32288,#32289,#32290,#32291,#32292,#32293,#32294,#32295,
#32296,#32297,#32298,#32299,#32300,#32301,#32302,#32303,#32304,#32305,#32306,
#32307,#32308,#32309,#32310,#32311,#32312,#32313,#32314,#32315,#32316,#32317,
#32318,#32319,#32320,#32321,#32322,#32323,#32324,#32325,#32326,#32327,#32328,
#32329,#32330,#32331,#32332,#32333,#32334,#32335,#32336,#32337,#32338,#32339,
#32340,#32341,#32342,#32343,#32344,#32345,#32346,#32347,#32348,#32349,#32350,
#32351,#32352,#32353,#32354,#32355,#32356,#32357,#32358,#32359,#32360,#32361,
#32362,#32363,#32364,#32365,#32366,#32367,#32368,#32369,#32370,#32371,#32372,
#32373,#32374,#32375,#32376,#32377,#32378,#32379,#32380,#32381,#32382,#32383,
#32384,#32385,#32386,#32387,#32388,#32389,#32390,#32391,#32392,#32393,#32394,
#32395,#32396,#32397,#32398,#32399,#32400,#32401,#32402,#32403,#32404,#32405,
#32406,#32407,#32408,#32409,#32410,#32411,#32412,#32413,#32414,#32415,#32416,
#32417,#32418,#32419,#32420,#32421,#32422,#32423,#32424,#32425,#32426,#32427,
#32428,#32429,#32430,#32431,#32432,#32433,#32434,#32435,#32436,#32437,#32438,
#32439,#32440,#32441,#32442,#32443,#32444,#32445,#32446,#32447,#32448,#32449,
#32450,#32451,#32452,#32453,#32454,#32455,#32456,#32457,#32458,#32459,#32460,
#32461,#32462,#32463,#32464,#32465,#32466,#32467,#32468,#32469,#32470,#32471,
#32472,#32473,#32474,#32475,#32476,#32477,#32478,#32479,#32480,#32481,#32482,
#32483,#32484,#32485,#32486,#32487,#32488,#32489,#32490,#32491,#32492,#32493,
#32494,#32495,#32496,#32497,#32498,#32499,#32500,#32501,#32502,#32503,#32504,
#32505,#32506,#32507,#32508,#32509,#32510,#32511,#32512,#32513,#32514,#32515,
#32516,#32517,#32518,#32519,#32520,#32521,#32522,#32523,#32524,#32525,#32526,
#32527,#32528,#32529,#32530,#32531,#32532,#32533,#32534,#32535,#32536,#32537,
#32538,#32539,#32540,#32541,#32542,#32543,#32544,#32545,#32546,#32547,#32548,
#32549,#32550,#32551,#32552,#32553,#32554,#32555,#32556,#32557,#32558,#32559,
#32560,#32561,#32562,#32563,#32564,#32565,#32566,#32567,#32568,#32569,#32570,
#32571,#32572,#32573,#32574,#32575,#32576,#32577,#32578,#32579,#32580,#32581,
#32582,#32583,#32584,#32585,#32586,#32587,#32588,#32589,#32590,#32591,#32592,
#32593,#32594,#32595,#32596,#32597,#32598,#32599,#32600,#32601,#32602,#32603,
#32604,#32605,#32606,#32607,#32608,#32609,#32610,#32611,#32612,#32613,#32614,
#32615,#32616,#32617,#32618,#32619,#32620,#32621,#32622,#32623,#32624,#32625,
#32626,#32627),.UNSPECIFIED.,.F.,.F.)
B_SPLINE_CURVE_WITH_KNOTS((3,2,2,2,2,2,2,2,2,2,2,2,2,2,2,2,2,2,2,2,2,2,
2,2,2,2,2,2,2,2,2,2,2,2,2,2,2,2,2,2,2,2,2,2,2,2,2,2,2,2,2,2,2,2,2,2,2,2,
2,2,2,2,2,2,2,2,2,2,2,2,2,2,2,2,2,2,2,2,2,2,2,2,2,2,2,2,2,2,2,2,2,2,2,2,
2,2,2,2,2,2,2,2,2,2,2,2,2,2,2,2,2,2,2,2,2,2,2,2,2,2,2,2,2,2,2,2,2,2,2,2,
2,2,2,2,2,2,2,2,2,2,2,2,2,2,2,2,2,2,2,2,2,2,2,2,2,2,2,2,2,2,2,2,2,2,2,2,
2,2,2,2,2,2,2,2,2,2,2,2,2,2,2,2,2,2,2,2,2,2,2,2,2,2,2,2,2,2,2,2,2,2,2,2,
2,2,2,2,2,2,2,2,2,2,2,2,2,2,2,2,2,2,2,2,2,2,2,2,2,2,2,2,2,2,2,2,2,2,2,2,
2,2,2,2,2,2,2,2,2,2,2,2,2,2,2,2,2,2,2,2,2,2,2,2,2,2,2,2,2,2,2,2,2,2,2,2,
2,2,2,2,2,2,2,2,2,2,2,2,2,2,2,2,2,2,2,2,2,2,2,2,2,2,2,2,2,2,2,2,2,2,2,2,
2,2,2,2,2,2,2,2,2,2,2,2,2,2,2,2,2,2,2,2,2,2,2,2,2,2,2,2,2,2,2,2,2,2,2,2,
2,2,2,2,2,2,2,2,2,2,2,2,2,2,2,2,2,2,2,2,2,2,2,2,2,2,2,2,2,2,2,2,2,2,2,2,
2,2,2,2,2,2,2,2,2,2,2,2,2,2,2,2,2,2,2,2,2,2,2,2,2,2,2,2,2,2,2,2,2,2,2,2,
2,2,2,2,2,2,2,2,2,2,2,2,2,2,2,2,2,2,2,2,2,2,2,2,2,2,2,2,2,2,2,2,2,2,2,2,
2,2,2,2,2,2,2,2,2,2,2,2,2,2,2,2,2,2,3),(4.54089542788183E-5,0.00205761316872428,
0.00411522633744856,0.00617283950617284,0.00823045267489712,0.0102880658436214,
0.0123456790123457,0.01440329218107,0.0164609053497942,0.0185185185185185,
0.0205761316872428,0.0226337448559671,0.0246913580246914,0.0267489711934156,
0.0288065843621399,0.0308641975308642,0.0329218106995885,0.0349794238683128,
0.037037037037037,0.0390946502057613,0.0411522633744856,0.0432098765432099,
0.0452674897119342,0.0473251028806584,0.0493827160493827,0.051440329218107,
0.0534979423868313,0.0555555555555556,0.0576131687242798,0.0596707818930041,
0.0617283950617284,0.0637860082304527,0.065843621399177,0.0679012345679012,
0.0699588477366255,0.0720164609053498,0.0740740740740741,0.0761316872427984,
0.0781893004115226,0.0802469135802469,0.0823045267489712,0.0843621399176955,
0.0864197530864197,0.088477366255144,0.0905349794238683,0.0925925925925926,
0.0946502057613169,0.0967078189300412,0.0987654320987654,0.10082304526749,
0.102880658436214,0.104938271604938,0.106995884773663,0.109053497942387,
0.111111111111111,0.113168724279835,0.11522633744856,0.117283950617284,
0.119341563786008,0.121399176954733,0.123456790123457,0.125514403292181,
0.127572016460905,0.12962962962963,0.131687242798354,0.133744855967078,
0.135802469135802,0.137860082304527,0.139917695473251,0.141975308641975,
0.1440329218107,0.146090534979424,0.148148148148148,0.150205761316872,0.152263374485597,
0.154320987654321,0.156378600823045,0.15843621399177,0.160493827160494,
0.162551440329218,0.164609053497942,0.166666666666667,0.168724279835391,
0.170781893004115,0.172839506172839,0.174897119341564,0.176954732510288,
0.179012345679012,0.181069958847737,0.183127572016461,0.185185185185185,
0.187242798353909,0.189300411522634,0.191358024691358,0.193415637860082,
0.195473251028807,0.197530864197531,0.199588477366255,0.201646090534979,
0.203703703703704,0.205761316872428,0.207818930041152,0.209876543209877,
0.211934156378601,0.213991769547325,0.216049382716049,0.218106995884774,
0.220164609053498,0.222222222222222,0.224279835390947,0.226337448559671,
0.228395061728395,0.230452674897119,0.232510288065844,0.234567901234568,
0.236625514403292,0.238683127572016,0.240740740740741,0.242798353909465,
0.244855967078189,0.246913580246914,0.248971193415638,0.251028806584362,
0.253086419753086,0.255144032921811,0.257201646090535,0.259259259259259,
0.261316872427984,0.263374485596708,0.265432098765432,0.267489711934156,
0.269547325102881,0.271604938271605,0.273662551440329,0.275720164609054,
0.277777777777778,0.279835390946502,0.281893004115226,0.283950617283951,
0.286008230452675,0.288065843621399,0.290123456790123,0.292181069958848,
0.294238683127572,0.296296296296296,0.298353909465021,0.300411522633745,
0.302469135802469,0.304526748971193,0.306584362139918,0.308641975308642,
0.310699588477366,0.312757201646091,0.314814814814815,0.316872427983539,
0.318930041152263,0.320987654320988,0.323045267489712,0.325102880658436,
0.327160493827161,0.329218106995885,0.331275720164609,0.333333333333333,
0.335390946502058,0.337448559670782,0.339506172839506,0.34156378600823,
0.343621399176955,0.345679012345679,0.347736625514403,0.349794238683128,
0.351851851851852,0.353909465020576,0.3559670781893,0.358024691358025,0.360082304526749,
0.362139917695473,0.364197530864198,0.366255144032922,0.368312757201646,
0.37037037037037,0.372427983539095,0.374485596707819,0.376543209876543,
0.378600823045267,0.380658436213992,0.382716049382716,0.38477366255144,
0.386831275720165,0.388888888888889,0.390946502057613,0.393004115226337,
0.395061728395062,0.397119341563786,0.39917695473251,0.401234567901235,
0.403292181069959,0.405349794238683,0.407407407407407,0.409465020576132,
0.411522633744856,0.41358024691358,0.415637860082305,0.417695473251029,
0.419753086419753,0.421810699588477,0.423868312757202,0.425925925925926,
0.42798353909465,0.430041152263374,0.432098765432099,0.434156378600823,
0.436213991769547,0.438271604938272,0.440329218106996,0.44238683127572,
0.444444444444444,0.446502057613169,0.448559670781893,0.450617283950617,
0.452674897119342,0.454732510288066,0.45679012345679,0.458847736625514,
0.460905349794239,0.462962962962963,0.465020576131687,0.467078189300412,
0.469135802469136,0.47119341563786,0.473251028806584,0.475308641975309,
0.477366255144033,0.479423868312757,0.481481481481482,0.483539094650206,
0.48559670781893,0.487654320987654,0.489711934156379,0.491769547325103,
0.493827160493827,0.495884773662551,0.497942386831276,0.5,0.502057613168724,
0.504115226337449,0.506172839506173,0.508230452674897,0.510288065843621,
0.512345679012346,0.51440329218107,0.516460905349794,0.518518518518519,
0.520576131687243,0.522633744855967,0.524691358024691,0.526748971193416,
0.52880658436214,0.530864197530864,0.532921810699588,0.534979423868313,
0.537037037037037,0.539094650205761,0.541152263374486,0.54320987654321,
0.545267489711934,0.547325102880658,0.549382716049383,0.551440329218107,
0.553497942386831,0.555555555555556,0.55761316872428,0.559670781893004,
0.561728395061728,0.563786008230453,0.565843621399177,0.567901234567901,
0.569958847736626,0.57201646090535,0.574074074074074,0.576131687242798,
0.578189300411523,0.580246913580247,0.582304526748971,0.584362139917695,
0.58641975308642,0.588477366255144,0.590534979423868,0.592592592592593,
0.594650205761317,0.596707818930041,0.598765432098765,0.60082304526749,
0.602880658436214,0.604938271604938,0.606995884773663,0.609053497942387,
0.611111111111111,0.613168724279835,0.61522633744856,0.617283950617284,
0.619341563786008,0.621399176954732,0.623456790123457,0.625514403292181,
0.627572016460905,0.62962962962963,0.631687242798354,0.633744855967078,
0.635802469135803,0.637860082304527,0.639917695473251,0.641975308641975,
0.6440329218107,0.646090534979424,0.648148148148148,0.650205761316872,0.652263374485597,
0.654320987654321,0.656378600823045,0.65843621399177,0.660493827160494,
0.662551440329218,0.664609053497942,0.666666666666667,0.668724279835391,
0.670781893004115,0.672839506172839,0.674897119341564,0.676954732510288,
0.679012345679012,0.681069958847737,0.683127572016461,0.685185185185185,
0.687242798353909,0.689300411522634,0.691358024691358,0.693415637860082,
0.695473251028807,0.697530864197531,0.699588477366255,0.701646090534979,
0.703703703703704,0.705761316872428,0.707818930041152,0.709876543209877,
0.711934156378601,0.713991769547325,0.716049382716049,0.718106995884774,
0.720164609053498,0.722222222222222,0.724279835390947,0.726337448559671,
0.728395061728395,0.730452674897119,0.732510288065844,0.734567901234568,
0.736625514403292,0.738683127572016,0.740740740740741,0.742798353909465,
0.744855967078189,0.746913580246914,0.748971193415638,0.751028806584362,
0.753086419753086,0.755144032921811,0.757201646090535,0.759259259259259,
0.761316872427984,0.763374485596708,0.765432098765432,0.767489711934156,
0.769547325102881,0.771604938271605,0.773662551440329,0.775720164609053,
0.777777777777778,0.779835390946502,0.781893004115226,0.783950617283951,
0.786008230452675,0.788065843621399,0.790123456790123,0.792181069958848,
0.794238683127572,0.796296296296296,0.798353909465021,0.800411522633745,
0.802469135802469,0.804526748971193,0.806584362139918,0.808641975308642,
0.810699588477366,0.812757201646091,0.814814814814815,0.816872427983539,
0.818930041152263,0.820987654320988,0.823045267489712,0.825102880658436,
0.827160493827161,0.829218106995885,0.831275720164609,0.833333333333333,
0.835390946502058,0.837448559670782,0.839506172839506,0.84156378600823,
0.843621399176955,0.845679012345679,0.847736625514403,0.849794238683128,
0.851851851851852,0.853909465020576,0.8559670781893,0.858024691358025,0.860082304526749,
0.862139917695473,0.864197530864197,0.866255144032922,0.868312757201646,
0.87037037037037,0.872427983539095,0.874485596707819,0.876543209876543,
0.878600823045268,0.880658436213992,0.882716049382716,0.88477366255144,
0.886831275720165,0.888888888888889,0.890946502057613,0.893004115226337,
0.895061728395062,0.897119341563786,0.89917695473251,0.901234567901235,
0.903292181069959,0.905349794238683,0.907407407407407,0.909465020576132,
0.911522633744856,0.91358024691358,0.915637860082305,0.917695473251029,
0.919753086419753,0.921810699588477,0.923868312757202,0.925925925925926,
0.92798353909465,0.930041152263374,0.932098765432099,0.934156378600823,
0.936213991769547,0.938271604938272,0.940329218106996,0.94238683127572,
0.944444444444444,0.946502057613169,0.948559670781893,0.950617283950617,
0.952674897119342,0.954732510288066,0.95679012345679,0.958847736625514,
0.960905349794239,0.962962962962963,0.965020576131687,0.967078189300412,
0.969135802469136,0.970064444260615),.UNSPECIFIED.)
CURVE()
GEOMETRIC_REPRESENTATION_ITEM()
RATIONAL_B_SPLINE_CURVE((0.994217195025686,0.868982055893079,1.,0.866025403784439,
1.,0.866025403784439,1.,0.866025403784439,1.,0.866025403784439,1.,0.866025403784439,
1.,0.866025403784439,1.,0.866025403784439,1.,0.866025403784439,1.,0.866025403784439,
1.,0.866025403784439,1.,0.866025403784439,1.,0.866025403784439,1.,0.866025403784439,
1.,0.866025403784439,1.,0.866025403784439,1.,0.866025403784439,1.,0.866025403784439,
1.,0.866025403784439,1.,0.866025403784439,1.,0.866025403784439,1.,0.866025403784439,
1.,0.866025403784439,1.,0.866025403784439,1.,0.866025403784439,1.,0.866025403784439,
1.,0.866025403784439,1.,0.866025403784439,1.,0.866025403784439,1.,0.866025403784439,
1.,0.866025403784439,1.,0.866025403784439,1.,0.866025403784439,1.,0.866025403784439,
1.,0.866025403784439,1.,0.866025403784439,1.,0.866025403784439,1.,0.866025403784439,
1.,0.866025403784439,1.,0.866025403784439,1.,0.866025403784439,1.,0.866025403784439,
1.,0.866025403784439,1.,0.866025403784439,1.,0.866025403784439,1.,0.866025403784439,
1.,0.866025403784439,1.,0.866025403784439,1.,0.866025403784439,1.,0.866025403784439,
1.,0.866025403784439,1.,0.866025403784439,1.,0.866025403784439,1.,0.866025403784439,
1.,0.866025403784439,1.,0.866025403784439,1.,0.866025403784439,1.,0.866025403784439,
1.,0.866025403784439,1.,0.866025403784439,1.,0.866025403784439,1.,0.866025403784439,
1.,0.866025403784439,1.,0.866025403784439,1.,0.866025403784439,1.,0.866025403784439,
1.,0.866025403784439,1.,0.866025403784439,1.,0.866025403784439,1.,0.866025403784439,
1.,0.866025403784439,1.,0.866025403784439,1.,0.866025403784439,1.,0.866025403784439,
1.,0.866025403784439,1.,0.866025403784439,1.,0.866025403784439,1.,0.866025403784439,
1.,0.866025403784439,1.,0.866025403784439,1.,0.866025403784439,1.,0.866025403784439,
1.,0.866025403784439,1.,0.866025403784439,1.,0.866025403784439,1.,0.866025403784439,
1.,0.866025403784439,1.,0.866025403784439,1.,0.866025403784439,1.,0.866025403784439,
1.,0.866025403784439,1.,0.866025403784439,1.,0.866025403784439,1.,0.866025403784439,
1.,0.866025403784439,1.,0.866025403784439,1.,0.866025403784439,1.,0.866025403784439,
1.,0.866025403784439,1.,0.866025403784439,1.,0.866025403784439,1.,0.866025403784439,
1.,0.866025403784439,1.,0.866025403784439,1.,0.866025403784439,1.,0.866025403784439,
1.,0.866025403784439,1.,0.866025403784439,1.,0.866025403784439,1.,0.866025403784439,
1.,0.866025403784439,1.,0.866025403784439,1.,0.866025403784439,1.,0.866025403784439,
1.,0.866025403784439,1.,0.866025403784439,1.,0.866025403784439,1.,0.866025403784439,
1.,0.866025403784439,1.,0.866025403784439,1.,0.866025403784439,1.,0.866025403784439,
1.,0.866025403784439,1.,0.866025403784439,1.,0.866025403784439,1.,0.866025403784439,
1.,0.866025403784439,1.,0.866025403784439,1.,0.866025403784439,1.,0.866025403784439,
1.,0.866025403784439,1.,0.866025403784439,1.,0.866025403784439,1.,0.866025403784439,
1.,0.866025403784439,1.,0.866025403784439,1.,0.866025403784439,1.,0.866025403784439,
1.,0.866025403784439,1.,0.866025403784439,1.,0.866025403784439,1.,0.866025403784439,
1.,0.866025403784439,1.,0.866025403784439,1.,0.866025403784439,1.,0.866025403784439,
1.,0.866025403784439,1.,0.866025403784439,1.,0.866025403784439,1.,0.866025403784439,
1.,0.866025403784439,1.,0.866025403784439,1.,0.866025403784439,1.,0.866025403784439,
1.,0.866025403784439,1.,0.866025403784439,1.,0.866025403784439,1.,0.866025403784439,
1.,0.866025403784439,1.,0.866025403784439,1.,0.866025403784439,1.,0.866025403784439,
1.,0.866025403784439,1.,0.866025403784439,1.,0.866025403784439,1.,0.866025403784439,
1.,0.866025403784439,1.,0.866025403784439,1.,0.866025403784439,1.,0.866025403784439,
1.,0.866025403784439,1.,0.866025403784439,1.,0.866025403784439,1.,0.866025403784439,
1.,0.866025403784439,1.,0.866025403784439,1.,0.866025403784439,1.,0.866025403784439,
1.,0.866025403784439,1.,0.866025403784439,1.,0.866025403784439,1.,0.866025403784439,
1.,0.866025403784439,1.,0.866025403784439,1.,0.866025403784439,1.,0.866025403784439,
1.,0.866025403784439,1.,0.866025403784439,1.,0.866025403784439,1.,0.866025403784439,
1.,0.866025403784439,1.,0.866025403784439,1.,0.866025403784439,1.,0.866025403784439,
1.,0.866025403784439,1.,0.866025403784439,1.,0.866025403784439,1.,0.866025403784439,
1.,0.866025403784439,1.,0.866025403784439,1.,0.866025403784439,1.,0.866025403784439,
1.,0.866025403784439,1.,0.866025403784439,1.,0.866025403784439,1.,0.866025403784439,
1.,0.866025403784439,1.,0.866025403784439,1.,0.866025403784439,1.,0.866025403784439,
1.,0.866025403784439,1.,0.866025403784439,1.,0.866025403784439,1.,0.866025403784439,
1.,0.866025403784439,1.,0.866025403784439,1.,0.866025403784439,1.,0.866025403784439,
1.,0.866025403784439,1.,0.866025403784439,1.,0.866025403784439,1.,0.866025403784439,
1.,0.866025403784439,1.,0.866025403784439,1.,0.866025403784439,1.,0.866025403784439,
1.,0.866025403784439,1.,0.866025403784439,1.,0.866025403784439,1.,0.866025403784439,
1.,0.866025403784439,1.,0.866025403784439,1.,0.866025403784439,1.,0.866025403784439,
1.,0.866025403784439,1.,0.866025403784439,1.,0.866025403784439,1.,0.866025403784439,
1.,0.866025403784439,1.,0.866025403784439,1.,0.866025403784439,1.,0.866025403784439,
1.,0.866025403784439,1.,0.866025403784439,1.,0.866025403784439,1.,0.866025403784439,
1.,0.866025403784439,1.,0.866025403784439,1.,0.866025403784439,1.,0.866025403784439,
1.,0.866025403784439,1.,0.866025403784439,1.,0.866025403784439,1.,0.866025403784439,
1.,0.866025403784439,1.,0.866025403784439,1.,0.866025403784439,1.,0.866025403784439,
1.,0.866025403784439,1.,0.866025403784439,1.,0.866025403784439,1.,0.866025403784439,
1.,0.866025403784439,1.,0.866025403784439,1.,0.866025403784439,1.,0.866025403784439,
1.,0.866025403784439,1.,0.866025403784439,1.,0.866025403784439,1.,0.866025403784439,
1.,0.866025403784439,1.,0.866025403784439,1.,0.866025403784439,1.,0.866025403784439,
1.,0.866025403784439,1.,0.866025403784439,1.,0.866025403784439,1.,0.866025403784439,
1.,0.866025403784439,1.,0.866025403784439,1.,0.866025403784439,1.,0.866025403784439,
1.,0.866025403784439,1.,0.866025403784439,1.,0.866025403784439,1.,0.866025403784439,
1.,0.866025403784439,1.,0.866025403784439,1.,0.866025403784439,1.,0.866025403784439,
1.,0.866025403784439,1.,0.866025403784439,1.,0.866025403784439,1.,0.866025403784439,
1.,0.866025403784439,1.,0.866025403784439,1.,0.866025403784439,1.,0.866025403784439,
1.,0.866025403784439,1.,0.866025403784439,1.,0.866025403784439,1.,0.866025403784439,
1.,0.866025403784439,1.,0.866025403784439,1.,0.866025403784439,1.,0.866025403784439,
1.,0.866025403784439,1.,0.866025403784439,1.,0.866025403784439,1.,0.866025403784439,
1.,0.866025403784439,1.,0.866025403784439,1.,0.866025403784439,1.,0.866025403784439,
1.,0.866025403784439,1.,0.866025403784439,1.,0.866025403784439,1.,0.866025403784439,
1.,0.866025403784439,1.,0.866025403784439,1.,0.866025403784439,1.,0.866025403784439,
1.,0.866025403784439,1.,0.866025403784439,1.,0.866025403784439,1.,0.866025403784439,
1.,0.866025403784439,1.,0.866025403784439,1.,0.866025403784439,1.,0.866025403784439,
1.,0.866025403784439,1.,0.866025403784439,1.,0.866025403784439,1.,0.866025403784439,
1.,0.866025403784439,1.,0.866025403784439,1.,0.866025403784439,1.,0.866025403784439,
1.,0.866025403784439,1.,0.866025403784439,1.,0.866025403784439,1.,0.866025403784439,
1.,0.866025403784439,1.,0.866025403784439,1.,0.866025403784439,1.,0.866025403784439,
1.,0.866025403784439,1.,0.866025403784439,1.,0.866025403784439,1.,0.866025403784439,
1.,0.866025403784439,1.,0.866025403784439,1.,0.866025403784439,1.,0.866025403784439,
1.,0.866025403784439,1.,0.866025403784439,1.,0.866025403784439,1.,0.866025403784439,
1.,0.866025403784439,1.,0.866025403784439,1.,0.866025403784439,1.,0.866025403784439,
1.,0.866025403784439,1.,0.866025403784439,1.,0.866025403784439,1.,0.866025403784439,
1.,0.866025403784439,1.,0.866025403784439,1.,0.866025403784439,1.,0.866025403784439,
1.,0.866025403784439,1.,0.866025403784439,1.,0.866025403784439,1.,0.866025403784439,
1.,0.866025403784439,1.,0.866025403784439,1.,0.866025403784439,1.,0.866025403784439,
1.,0.866025403784439,1.,0.866025403784439,1.,0.866025403784439,1.,0.866025403784439,
1.,0.866025403784439,1.,0.866025403784439,1.,0.866025403784439,1.,0.866025403784439,
1.,0.866025403784439,1.,0.866025403784439,1.,0.866025403784439,1.,0.866025403784439,
1.,0.866025403784439,1.,0.866025403784439,1.,0.866025403784439,1.,0.866025403784439,
1.,0.866025403784439,1.,0.866025403784439,1.,0.866025403784439,1.,0.866025403784439,
1.,0.866025403784439,1.,0.866025403784439,1.,0.866025403784439,1.,0.866025403784439,
1.,0.866025403784439,1.,0.866025403784439,1.,0.866025403784439,1.,0.866025403784439,
1.,0.866025403784439,1.,0.866025403784439,1.,0.866025403784439,1.,0.866025403784439,
1.,0.866025403784439,1.,0.866025403784439,1.,0.866025403784439,1.,0.866025403784439,
1.,0.866025403784439,1.,0.866025403784439,1.,0.866025403784439,1.,0.866025403784439,
1.,0.866025403784439,1.,0.866025403784439,1.,0.866025403784439,1.,0.866025403784439,
1.,0.866025403784439,1.,0.866025403784439,1.,0.866025403784439,1.,0.866025403784439,
1.,0.866025403784439,1.,0.866025403784439,1.,0.866025403784439,1.,0.866025403784439,
1.,0.866025403784439,1.,0.866025403784439,1.,0.866025403784439,1.,0.866025403784439,
1.,0.866025403784439,1.,0.866025403784439,1.,0.866025403784439,1.,0.866025403784439,
1.,0.866025403784439,1.,0.866025403784439,1.,0.866025403784439,1.,0.866025403784439,
1.,0.866025403784439,1.,0.866025403784439,1.,0.866025403784439,1.,0.866025403784439,
1.,0.866025403784439,1.,0.866025403784439,1.,0.866025403784439,1.,0.866025403784439,
1.,0.866025403784439,1.,0.866025403784439,1.,0.866025403784439,1.,0.866025403784439,
1.,0.866025403784439,1.,0.866025403784439,1.,0.866025403784439,1.,0.866025403784439,
1.,0.866025403784439,1.,0.866025403784439,1.,0.866025403784439,1.,0.866025403784439,
1.,0.866025403784439,1.,0.866025403784439,1.,0.866025403784439,1.,0.866025403784439,
1.,0.866025403784439,1.,0.866025403784439,1.,0.866025403784439,1.,0.866025403784439,
1.,0.866025403784439,1.,0.939534597205461,0.933647674785266))
REPRESENTATION_ITEM('')
);
#202=(
BOUNDED_CURVE()
B_SPLINE_CURVE(2,(#36521,#36522,#36523,#36524,#36525,#36526,#36527,#36528,
#36529,#36530,#36531,#36532,#36533,#36534,#36535,#36536,#36537,#36538,#36539,
#36540,#36541,#36542,#36543,#36544,#36545,#36546,#36547,#36548,#36549,#36550,
#36551,#36552,#36553,#36554,#36555,#36556,#36557,#36558,#36559,#36560,#36561,
#36562,#36563,#36564,#36565,#36566,#36567,#36568,#36569,#36570,#36571,#36572,
#36573,#36574,#36575,#36576,#36577,#36578,#36579,#36580,#36581,#36582,#36583,
#36584,#36585,#36586,#36587,#36588,#36589,#36590,#36591,#36592,#36593,#36594,
#36595,#36596,#36597,#36598,#36599,#36600,#36601,#36602,#36603,#36604,#36605,
#36606,#36607,#36608,#36609,#36610,#36611,#36612,#36613,#36614,#36615,#36616,
#36617,#36618,#36619,#36620,#36621,#36622,#36623,#36624,#36625,#36626,#36627,
#36628,#36629,#36630,#36631,#36632,#36633,#36634,#36635,#36636,#36637,#36638,
#36639,#36640,#36641,#36642,#36643,#36644,#36645,#36646,#36647,#36648,#36649,
#36650,#36651,#36652,#36653,#36654,#36655,#36656,#36657,#36658,#36659,#36660,
#36661,#36662,#36663,#36664,#36665,#36666,#36667,#36668,#36669,#36670,#36671,
#36672,#36673,#36674,#36675,#36676,#36677,#36678,#36679,#36680,#36681,#36682,
#36683,#36684,#36685,#36686,#36687,#36688,#36689,#36690,#36691,#36692,#36693,
#36694,#36695,#36696,#36697,#36698,#36699,#36700,#36701,#36702,#36703,#36704,
#36705,#36706,#36707,#36708,#36709,#36710,#36711,#36712,#36713,#36714,#36715,
#36716,#36717,#36718,#36719,#36720,#36721,#36722,#36723,#36724,#36725,#36726,
#36727,#36728,#36729,#36730,#36731,#36732,#36733,#36734,#36735,#36736,#36737,
#36738,#36739,#36740,#36741,#36742,#36743,#36744,#36745,#36746,#36747,#36748,
#36749,#36750,#36751,#36752,#36753,#36754,#36755,#36756,#36757,#36758,#36759,
#36760,#36761,#36762,#36763,#36764,#36765,#36766,#36767,#36768,#36769,#36770,
#36771,#36772,#36773,#36774,#36775,#36776,#36777,#36778,#36779,#36780,#36781,
#36782,#36783,#36784,#36785,#36786,#36787,#36788,#36789,#36790,#36791,#36792,
#36793,#36794,#36795,#36796,#36797,#36798,#36799,#36800,#36801,#36802,#36803,
#36804,#36805,#36806,#36807,#36808,#36809,#36810,#36811,#36812,#36813,#36814,
#36815,#36816,#36817,#36818,#36819,#36820,#36821,#36822,#36823,#36824,#36825,
#36826,#36827,#36828,#36829,#36830,#36831,#36832,#36833,#36834,#36835,#36836,
#36837,#36838,#36839,#36840,#36841,#36842,#36843,#36844,#36845,#36846,#36847,
#36848,#36849,#36850,#36851,#36852,#36853,#36854,#36855,#36856,#36857,#36858,
#36859,#36860,#36861,#36862,#36863,#36864,#36865,#36866,#36867,#36868,#36869,
#36870,#36871,#36872,#36873,#36874,#36875,#36876,#36877,#36878,#36879,#36880,
#36881,#36882,#36883,#36884,#36885,#36886,#36887,#36888,#36889,#36890,#36891,
#36892,#36893,#36894,#36895,#36896,#36897,#36898,#36899,#36900,#36901,#36902,
#36903,#36904,#36905,#36906,#36907,#36908,#36909,#36910,#36911,#36912,#36913,
#36914,#36915,#36916,#36917,#36918,#36919,#36920,#36921,#36922,#36923,#36924,
#36925,#36926,#36927,#36928,#36929,#36930,#36931,#36932,#36933,#36934,#36935,
#36936,#36937,#36938,#36939,#36940,#36941,#36942,#36943,#36944,#36945,#36946,
#36947,#36948,#36949,#36950,#36951,#36952,#36953,#36954,#36955,#36956,#36957,
#36958,#36959,#36960,#36961,#36962,#36963,#36964,#36965,#36966,#36967,#36968,
#36969,#36970,#36971,#36972,#36973,#36974,#36975,#36976,#36977,#36978,#36979,
#36980,#36981,#36982,#36983,#36984,#36985,#36986,#36987,#36988,#36989,#36990,
#36991,#36992,#36993,#36994,#36995,#36996,#36997,#36998,#36999,#37000,#37001,
#37002,#37003,#37004,#37005,#37006,#37007,#37008,#37009,#37010,#37011,#37012,
#37013,#37014,#37015,#37016,#37017,#37018,#37019,#37020,#37021,#37022,#37023,
#37024,#37025,#37026,#37027,#37028,#37029,#37030,#37031,#37032,#37033,#37034,
#37035,#37036,#37037,#37038,#37039,#37040,#37041,#37042,#37043,#37044,#37045,
#37046,#37047,#37048,#37049,#37050,#37051,#37052,#37053,#37054,#37055,#37056,
#37057,#37058,#37059,#37060,#37061,#37062,#37063,#37064,#37065,#37066,#37067,
#37068,#37069,#37070,#37071,#37072,#37073,#37074,#37075,#37076,#37077,#37078,
#37079,#37080,#37081,#37082,#37083,#37084,#37085,#37086,#37087,#37088,#37089,
#37090,#37091,#37092,#37093,#37094,#37095,#37096,#37097,#37098,#37099,#37100,
#37101,#37102,#37103,#37104,#37105,#37106,#37107,#37108,#37109,#37110,#37111,
#37112,#37113,#37114,#37115,#37116,#37117,#37118,#37119,#37120,#37121,#37122,
#37123,#37124,#37125,#37126,#37127,#37128,#37129,#37130,#37131,#37132,#37133,
#37134,#37135,#37136,#37137,#37138,#37139,#37140,#37141,#37142,#37143,#37144,
#37145,#37146,#37147,#37148,#37149,#37150,#37151,#37152,#37153,#37154,#37155,
#37156,#37157,#37158,#37159,#37160,#37161,#37162,#37163,#37164,#37165,#37166,
#37167,#37168,#37169,#37170,#37171,#37172,#37173,#37174,#37175,#37176,#37177,
#37178,#37179,#37180,#37181,#37182,#37183,#37184,#37185,#37186,#37187,#37188,
#37189,#37190,#37191,#37192,#37193,#37194,#37195,#37196,#37197,#37198,#37199,
#37200,#37201,#37202,#37203,#37204,#37205,#37206,#37207,#37208,#37209,#37210,
#37211,#37212,#37213,#37214,#37215,#37216,#37217,#37218,#37219,#37220,#37221,
#37222,#37223,#37224,#37225,#37226,#37227,#37228,#37229,#37230,#37231,#37232,
#37233,#37234,#37235,#37236,#37237,#37238,#37239,#37240,#37241,#37242,#37243,
#37244,#37245,#37246,#37247,#37248,#37249,#37250,#37251,#37252,#37253,#37254,
#37255,#37256,#37257,#37258,#37259,#37260,#37261,#37262,#37263,#37264,#37265,
#37266,#37267,#37268,#37269,#37270,#37271,#37272,#37273,#37274,#37275,#37276,
#37277,#37278,#37279,#37280,#37281,#37282,#37283,#37284,#37285,#37286,#37287,
#37288,#37289,#37290,#37291,#37292,#37293,#37294,#37295,#37296,#37297,#37298,
#37299,#37300,#37301,#37302,#37303,#37304,#37305,#37306,#37307,#37308,#37309,
#37310,#37311,#37312,#37313,#37314,#37315,#37316,#37317,#37318,#37319,#37320,
#37321,#37322,#37323,#37324,#37325,#37326,#37327,#37328,#37329,#37330,#37331,
#37332,#37333,#37334,#37335,#37336,#37337,#37338,#37339,#37340,#37341,#37342,
#37343,#37344,#37345,#37346,#37347,#37348,#37349,#37350,#37351,#37352,#37353,
#37354,#37355,#37356,#37357,#37358,#37359,#37360,#37361,#37362,#37363,#37364,
#37365,#37366,#37367,#37368,#37369,#37370,#37371,#37372,#37373,#37374,#37375,
#37376,#37377,#37378,#37379,#37380,#37381,#37382,#37383,#37384,#37385,#37386,
#37387,#37388,#37389,#37390,#37391,#37392,#37393,#37394,#37395,#37396,#37397,
#37398,#37399,#37400,#37401,#37402,#37403,#37404,#37405,#37406,#37407,#37408,
#37409,#37410,#37411,#37412,#37413,#37414,#37415,#37416,#37417,#37418,#37419,
#37420,#37421,#37422,#37423,#37424,#37425,#37426,#37427,#37428,#37429,#37430,
#37431,#37432,#37433,#37434,#37435,#37436,#37437,#37438,#37439,#37440,#37441,
#37442,#37443,#37444,#37445,#37446,#37447,#37448,#37449,#37450,#37451,#37452,
#37453,#37454,#37455,#37456,#37457,#37458,#37459,#37460,#37461,#37462,#37463,
#37464,#37465),.UNSPECIFIED.,.F.,.F.)
B_SPLINE_CURVE_WITH_KNOTS((3,2,2,2,2,2,2,2,2,2,2,2,2,2,2,2,2,2,2,2,2,2,
2,2,2,2,2,2,2,2,2,2,2,2,2,2,2,2,2,2,2,2,2,2,2,2,2,2,2,2,2,2,2,2,2,2,2,2,
2,2,2,2,2,2,2,2,2,2,2,2,2,2,2,2,2,2,2,2,2,2,2,2,2,2,2,2,2,2,2,2,2,2,2,2,
2,2,2,2,2,2,2,2,2,2,2,2,2,2,2,2,2,2,2,2,2,2,2,2,2,2,2,2,2,2,2,2,2,2,2,2,
2,2,2,2,2,2,2,2,2,2,2,2,2,2,2,2,2,2,2,2,2,2,2,2,2,2,2,2,2,2,2,2,2,2,2,2,
2,2,2,2,2,2,2,2,2,2,2,2,2,2,2,2,2,2,2,2,2,2,2,2,2,2,2,2,2,2,2,2,2,2,2,2,
2,2,2,2,2,2,2,2,2,2,2,2,2,2,2,2,2,2,2,2,2,2,2,2,2,2,2,2,2,2,2,2,2,2,2,2,
2,2,2,2,2,2,2,2,2,2,2,2,2,2,2,2,2,2,2,2,2,2,2,2,2,2,2,2,2,2,2,2,2,2,2,2,
2,2,2,2,2,2,2,2,2,2,2,2,2,2,2,2,2,2,2,2,2,2,2,2,2,2,2,2,2,2,2,2,2,2,2,2,
2,2,2,2,2,2,2,2,2,2,2,2,2,2,2,2,2,2,2,2,2,2,2,2,2,2,2,2,2,2,2,2,2,2,2,2,
2,2,2,2,2,2,2,2,2,2,2,2,2,2,2,2,2,2,2,2,2,2,2,2,2,2,2,2,2,2,2,2,2,2,2,2,
2,2,2,2,2,2,2,2,2,2,2,2,2,2,2,2,2,2,2,2,2,2,2,2,2,2,2,2,2,2,2,2,2,2,2,2,
2,2,2,2,2,2,2,2,2,2,2,2,2,2,2,2,2,2,2,2,2,2,2,2,2,2,2,2,2,2,2,2,2,2,2,2,
2,2,2,2,2,2,2,2,2,2,2,2,2,2,2,2,2,2,3),(0.00472507824212208,0.00617283950617284,
0.00823045267489712,0.0102880658436214,0.0123456790123457,0.01440329218107,
0.0164609053497942,0.0185185185185185,0.0205761316872428,0.0226337448559671,
0.0246913580246914,0.0267489711934156,0.0288065843621399,0.0308641975308642,
0.0329218106995885,0.0349794238683128,0.037037037037037,0.0390946502057613,
0.0411522633744856,0.0432098765432099,0.0452674897119342,0.0473251028806584,
0.0493827160493827,0.051440329218107,0.0534979423868313,0.0555555555555556,
0.0576131687242798,0.0596707818930041,0.0617283950617284,0.0637860082304527,
0.065843621399177,0.0679012345679012,0.0699588477366255,0.0720164609053498,
0.0740740740740741,0.0761316872427984,0.0781893004115226,0.0802469135802469,
0.0823045267489712,0.0843621399176955,0.0864197530864197,0.088477366255144,
0.0905349794238683,0.0925925925925926,0.0946502057613169,0.0967078189300412,
0.0987654320987654,0.10082304526749,0.102880658436214,0.104938271604938,
0.106995884773663,0.109053497942387,0.111111111111111,0.113168724279835,
0.11522633744856,0.117283950617284,0.119341563786008,0.121399176954733,
0.123456790123457,0.125514403292181,0.127572016460905,0.12962962962963,
0.131687242798354,0.133744855967078,0.135802469135802,0.137860082304527,
0.139917695473251,0.141975308641975,0.1440329218107,0.146090534979424,0.148148148148148,
0.150205761316872,0.152263374485597,0.154320987654321,0.156378600823045,
0.15843621399177,0.160493827160494,0.162551440329218,0.164609053497942,
0.166666666666667,0.168724279835391,0.170781893004115,0.172839506172839,
0.174897119341564,0.176954732510288,0.179012345679012,0.181069958847737,
0.183127572016461,0.185185185185185,0.187242798353909,0.189300411522634,
0.191358024691358,0.193415637860082,0.195473251028807,0.197530864197531,
0.199588477366255,0.201646090534979,0.203703703703704,0.205761316872428,
0.207818930041152,0.209876543209877,0.211934156378601,0.213991769547325,
0.216049382716049,0.218106995884774,0.220164609053498,0.222222222222222,
0.224279835390947,0.226337448559671,0.228395061728395,0.230452674897119,
0.232510288065844,0.234567901234568,0.236625514403292,0.238683127572016,
0.240740740740741,0.242798353909465,0.244855967078189,0.246913580246914,
0.248971193415638,0.251028806584362,0.253086419753086,0.255144032921811,
0.257201646090535,0.259259259259259,0.261316872427984,0.263374485596708,
0.265432098765432,0.267489711934156,0.269547325102881,0.271604938271605,
0.273662551440329,0.275720164609054,0.277777777777778,0.279835390946502,
0.281893004115226,0.283950617283951,0.286008230452675,0.288065843621399,
0.290123456790123,0.292181069958848,0.294238683127572,0.296296296296296,
0.298353909465021,0.300411522633745,0.302469135802469,0.304526748971193,
0.306584362139918,0.308641975308642,0.310699588477366,0.312757201646091,
0.314814814814815,0.316872427983539,0.318930041152263,0.320987654320988,
0.323045267489712,0.325102880658436,0.327160493827161,0.329218106995885,
0.331275720164609,0.333333333333333,0.335390946502058,0.337448559670782,
0.339506172839506,0.34156378600823,0.343621399176955,0.345679012345679,
0.347736625514403,0.349794238683128,0.351851851851852,0.353909465020576,
0.3559670781893,0.358024691358025,0.360082304526749,0.362139917695473,0.364197530864198,
0.366255144032922,0.368312757201646,0.37037037037037,0.372427983539095,
0.374485596707819,0.376543209876543,0.378600823045267,0.380658436213992,
0.382716049382716,0.38477366255144,0.386831275720165,0.388888888888889,
0.390946502057613,0.393004115226337,0.395061728395062,0.397119341563786,
0.39917695473251,0.401234567901235,0.403292181069959,0.405349794238683,
0.407407407407407,0.409465020576132,0.411522633744856,0.41358024691358,
0.415637860082305,0.417695473251029,0.419753086419753,0.421810699588477,
0.423868312757202,0.425925925925926,0.42798353909465,0.430041152263374,
0.432098765432099,0.434156378600823,0.436213991769547,0.438271604938272,
0.440329218106996,0.44238683127572,0.444444444444444,0.446502057613169,
0.448559670781893,0.450617283950617,0.452674897119342,0.454732510288066,
0.45679012345679,0.458847736625514,0.460905349794239,0.462962962962963,
0.465020576131687,0.467078189300412,0.469135802469136,0.47119341563786,
0.473251028806584,0.475308641975309,0.477366255144033,0.479423868312757,
0.481481481481481,0.483539094650206,0.48559670781893,0.487654320987654,
0.489711934156379,0.491769547325103,0.493827160493827,0.495884773662551,
0.497942386831276,0.5,0.502057613168724,0.504115226337449,0.506172839506173,
0.508230452674897,0.510288065843621,0.512345679012346,0.51440329218107,
0.516460905349794,0.518518518518518,0.520576131687243,0.522633744855967,
0.524691358024691,0.526748971193416,0.52880658436214,0.530864197530864,
0.532921810699588,0.534979423868313,0.537037037037037,0.539094650205761,
0.541152263374486,0.54320987654321,0.545267489711934,0.547325102880658,
0.549382716049383,0.551440329218107,0.553497942386831,0.555555555555556,
0.55761316872428,0.559670781893004,0.561728395061728,0.563786008230453,
0.565843621399177,0.567901234567901,0.569958847736626,0.57201646090535,
0.574074074074074,0.576131687242798,0.578189300411523,0.580246913580247,
0.582304526748971,0.584362139917695,0.58641975308642,0.588477366255144,
0.590534979423868,0.592592592592593,0.594650205761317,0.596707818930041,
0.598765432098765,0.60082304526749,0.602880658436214,0.604938271604938,
0.606995884773663,0.609053497942387,0.611111111111111,0.613168724279835,
0.61522633744856,0.617283950617284,0.619341563786008,0.621399176954732,
0.623456790123457,0.625514403292181,0.627572016460905,0.62962962962963,
0.631687242798354,0.633744855967078,0.635802469135803,0.637860082304527,
0.639917695473251,0.641975308641975,0.6440329218107,0.646090534979424,0.648148148148148,
0.650205761316872,0.652263374485597,0.654320987654321,0.656378600823045,
0.65843621399177,0.660493827160494,0.662551440329218,0.664609053497942,
0.666666666666667,0.668724279835391,0.670781893004115,0.672839506172839,
0.674897119341564,0.676954732510288,0.679012345679012,0.681069958847737,
0.683127572016461,0.685185185185185,0.687242798353909,0.689300411522634,
0.691358024691358,0.693415637860082,0.695473251028807,0.697530864197531,
0.699588477366255,0.701646090534979,0.703703703703704,0.705761316872428,
0.707818930041152,0.709876543209877,0.711934156378601,0.713991769547325,
0.716049382716049,0.718106995884774,0.720164609053498,0.722222222222222,
0.724279835390947,0.726337448559671,0.728395061728395,0.730452674897119,
0.732510288065844,0.734567901234568,0.736625514403292,0.738683127572016,
0.740740740740741,0.742798353909465,0.744855967078189,0.746913580246914,
0.748971193415638,0.751028806584362,0.753086419753086,0.755144032921811,
0.757201646090535,0.759259259259259,0.761316872427984,0.763374485596708,
0.765432098765432,0.767489711934156,0.769547325102881,0.771604938271605,
0.773662551440329,0.775720164609053,0.777777777777778,0.779835390946502,
0.781893004115226,0.783950617283951,0.786008230452675,0.788065843621399,
0.790123456790123,0.792181069958848,0.794238683127572,0.796296296296296,
0.798353909465021,0.800411522633745,0.802469135802469,0.804526748971193,
0.806584362139918,0.808641975308642,0.810699588477366,0.812757201646091,
0.814814814814815,0.816872427983539,0.818930041152263,0.820987654320988,
0.823045267489712,0.825102880658436,0.827160493827161,0.829218106995885,
0.831275720164609,0.833333333333333,0.835390946502058,0.837448559670782,
0.839506172839506,0.84156378600823,0.843621399176955,0.845679012345679,
0.847736625514403,0.849794238683128,0.851851851851852,0.853909465020576,
0.8559670781893,0.858024691358025,0.860082304526749,0.862139917695473,0.864197530864197,
0.866255144032922,0.868312757201646,0.87037037037037,0.872427983539095,
0.874485596707819,0.876543209876543,0.878600823045268,0.880658436213992,
0.882716049382716,0.88477366255144,0.886831275720165,0.888888888888889,
0.890946502057613,0.893004115226337,0.895061728395062,0.897119341563786,
0.89917695473251,0.901234567901235,0.903292181069959,0.905349794238683,
0.907407407407407,0.909465020576132,0.911522633744856,0.91358024691358,
0.915637860082305,0.917695473251029,0.919753086419753,0.921810699588477,
0.923868312757202,0.925925925925926,0.92798353909465,0.930041152263374,
0.932098765432099,0.934156378600823,0.936213991769547,0.938271604938272,
0.940329218106996,0.94238683127572,0.944444444444444,0.946502057613169,
0.948559670781893,0.950617283950617,0.952674897119342,0.954732510288066,
0.95679012345679,0.958847736625514,0.960905349794239,0.962962962962963,
0.965020576131687,0.967078189300412,0.969135802469136,0.97119341563786,
0.973251028806584,0.974693312758157),.UNSPECIFIED.)
CURVE()
GEOMETRIC_REPRESENTATION_ITEM()
RATIONAL_B_SPLINE_CURVE((0.944121295592482,0.905733869846882,1.,0.866025403784439,
1.,0.866025403784439,1.,0.866025403784439,1.,0.866025403784439,1.,0.866025403784439,
1.,0.866025403784439,1.,0.866025403784439,1.,0.866025403784439,1.,0.866025403784439,
1.,0.866025403784439,1.,0.866025403784439,1.,0.866025403784439,1.,0.866025403784439,
1.,0.866025403784439,1.,0.866025403784439,1.,0.866025403784439,1.,0.866025403784439,
1.,0.866025403784439,1.,0.866025403784439,1.,0.866025403784439,1.,0.866025403784439,
1.,0.866025403784439,1.,0.866025403784439,1.,0.866025403784439,1.,0.866025403784439,
1.,0.866025403784439,1.,0.866025403784439,1.,0.866025403784439,1.,0.866025403784439,
1.,0.866025403784439,1.,0.866025403784439,1.,0.866025403784439,1.,0.866025403784439,
1.,0.866025403784439,1.,0.866025403784439,1.,0.866025403784439,1.,0.866025403784439,
1.,0.866025403784439,1.,0.866025403784439,1.,0.866025403784439,1.,0.866025403784439,
1.,0.866025403784439,1.,0.866025403784439,1.,0.866025403784439,1.,0.866025403784439,
1.,0.866025403784439,1.,0.866025403784439,1.,0.866025403784439,1.,0.866025403784439,
1.,0.866025403784439,1.,0.866025403784439,1.,0.866025403784439,1.,0.866025403784439,
1.,0.866025403784439,1.,0.866025403784439,1.,0.866025403784439,1.,0.866025403784439,
1.,0.866025403784439,1.,0.866025403784439,1.,0.866025403784439,1.,0.866025403784439,
1.,0.866025403784439,1.,0.866025403784439,1.,0.866025403784439,1.,0.866025403784439,
1.,0.866025403784439,1.,0.866025403784439,1.,0.866025403784439,1.,0.866025403784439,
1.,0.866025403784439,1.,0.866025403784439,1.,0.866025403784439,1.,0.866025403784439,
1.,0.866025403784439,1.,0.866025403784439,1.,0.866025403784439,1.,0.866025403784439,
1.,0.866025403784439,1.,0.866025403784439,1.,0.866025403784439,1.,0.866025403784439,
1.,0.866025403784439,1.,0.866025403784439,1.,0.866025403784439,1.,0.866025403784439,
1.,0.866025403784439,1.,0.866025403784439,1.,0.866025403784439,1.,0.866025403784439,
1.,0.866025403784439,1.,0.866025403784439,1.,0.866025403784439,1.,0.866025403784439,
1.,0.866025403784439,1.,0.866025403784439,1.,0.866025403784439,1.,0.866025403784439,
1.,0.866025403784439,1.,0.866025403784439,1.,0.866025403784439,1.,0.866025403784439,
1.,0.866025403784439,1.,0.866025403784439,1.,0.866025403784439,1.,0.866025403784439,
1.,0.866025403784439,1.,0.866025403784439,1.,0.866025403784439,1.,0.866025403784439,
1.,0.866025403784439,1.,0.866025403784439,1.,0.866025403784439,1.,0.866025403784439,
1.,0.866025403784439,1.,0.866025403784439,1.,0.866025403784439,1.,0.866025403784439,
1.,0.866025403784439,1.,0.866025403784439,1.,0.866025403784439,1.,0.866025403784439,
1.,0.866025403784439,1.,0.866025403784439,1.,0.866025403784439,1.,0.866025403784439,
1.,0.866025403784439,1.,0.866025403784439,1.,0.866025403784439,1.,0.866025403784439,
1.,0.866025403784439,1.,0.866025403784439,1.,0.866025403784439,1.,0.866025403784439,
1.,0.866025403784439,1.,0.866025403784439,1.,0.866025403784439,1.,0.866025403784439,
1.,0.866025403784439,1.,0.866025403784439,1.,0.866025403784439,1.,0.866025403784439,
1.,0.866025403784439,1.,0.866025403784439,1.,0.866025403784439,1.,0.866025403784439,
1.,0.866025403784439,1.,0.866025403784439,1.,0.866025403784439,1.,0.866025403784439,
1.,0.866025403784439,1.,0.866025403784439,1.,0.866025403784439,1.,0.866025403784439,
1.,0.866025403784439,1.,0.866025403784439,1.,0.866025403784439,1.,0.866025403784439,
1.,0.866025403784439,1.,0.866025403784439,1.,0.866025403784439,1.,0.866025403784439,
1.,0.866025403784439,1.,0.866025403784439,1.,0.866025403784439,1.,0.866025403784439,
1.,0.866025403784439,1.,0.866025403784439,1.,0.866025403784439,1.,0.866025403784439,
1.,0.866025403784439,1.,0.866025403784439,1.,0.866025403784439,1.,0.866025403784439,
1.,0.866025403784439,1.,0.866025403784439,1.,0.866025403784439,1.,0.866025403784439,
1.,0.866025403784439,1.,0.866025403784439,1.,0.866025403784439,1.,0.866025403784439,
1.,0.866025403784439,1.,0.866025403784439,1.,0.866025403784439,1.,0.866025403784439,
1.,0.866025403784439,1.,0.866025403784439,1.,0.866025403784439,1.,0.866025403784439,
1.,0.866025403784439,1.,0.866025403784439,1.,0.866025403784439,1.,0.866025403784439,
1.,0.866025403784439,1.,0.866025403784439,1.,0.866025403784439,1.,0.866025403784439,
1.,0.866025403784439,1.,0.866025403784439,1.,0.866025403784439,1.,0.866025403784439,
1.,0.866025403784439,1.,0.866025403784439,1.,0.866025403784439,1.,0.866025403784439,
1.,0.866025403784439,1.,0.866025403784439,1.,0.866025403784439,1.,0.866025403784439,
1.,0.866025403784439,1.,0.866025403784439,1.,0.866025403784439,1.,0.866025403784439,
1.,0.866025403784439,1.,0.866025403784439,1.,0.866025403784439,1.,0.866025403784439,
1.,0.866025403784439,1.,0.866025403784439,1.,0.866025403784439,1.,0.866025403784439,
1.,0.866025403784439,1.,0.866025403784439,1.,0.866025403784439,1.,0.866025403784439,
1.,0.866025403784439,1.,0.866025403784439,1.,0.866025403784439,1.,0.866025403784439,
1.,0.866025403784439,1.,0.866025403784439,1.,0.866025403784439,1.,0.866025403784439,
1.,0.866025403784439,1.,0.866025403784439,1.,0.866025403784439,1.,0.866025403784439,
1.,0.866025403784439,1.,0.866025403784439,1.,0.866025403784439,1.,0.866025403784439,
1.,0.866025403784439,1.,0.866025403784439,1.,0.866025403784439,1.,0.866025403784439,
1.,0.866025403784439,1.,0.866025403784439,1.,0.866025403784439,1.,0.866025403784439,
1.,0.866025403784439,1.,0.866025403784439,1.,0.866025403784439,1.,0.866025403784439,
1.,0.866025403784439,1.,0.866025403784439,1.,0.866025403784439,1.,0.866025403784439,
1.,0.866025403784439,1.,0.866025403784439,1.,0.866025403784439,1.,0.866025403784439,
1.,0.866025403784439,1.,0.866025403784439,1.,0.866025403784439,1.,0.866025403784439,
1.,0.866025403784439,1.,0.866025403784439,1.,0.866025403784439,1.,0.866025403784439,
1.,0.866025403784439,1.,0.866025403784439,1.,0.866025403784439,1.,0.866025403784439,
1.,0.866025403784439,1.,0.866025403784439,1.,0.866025403784439,1.,0.866025403784439,
1.,0.866025403784439,1.,0.866025403784439,1.,0.866025403784439,1.,0.866025403784439,
1.,0.866025403784439,1.,0.866025403784439,1.,0.866025403784439,1.,0.866025403784439,
1.,0.866025403784439,1.,0.866025403784439,1.,0.866025403784439,1.,0.866025403784439,
1.,0.866025403784439,1.,0.866025403784439,1.,0.866025403784439,1.,0.866025403784439,
1.,0.866025403784439,1.,0.866025403784439,1.,0.866025403784439,1.,0.866025403784439,
1.,0.866025403784439,1.,0.866025403784439,1.,0.866025403784439,1.,0.866025403784439,
1.,0.866025403784439,1.,0.866025403784439,1.,0.866025403784439,1.,0.866025403784439,
1.,0.866025403784439,1.,0.866025403784439,1.,0.866025403784439,1.,0.866025403784439,
1.,0.866025403784439,1.,0.866025403784439,1.,0.866025403784439,1.,0.866025403784439,
1.,0.866025403784439,1.,0.866025403784439,1.,0.866025403784439,1.,0.866025403784439,
1.,0.866025403784439,1.,0.866025403784439,1.,0.866025403784439,1.,0.866025403784439,
1.,0.866025403784439,1.,0.866025403784439,1.,0.866025403784439,1.,0.866025403784439,
1.,0.866025403784439,1.,0.866025403784439,1.,0.866025403784439,1.,0.866025403784439,
1.,0.866025403784439,1.,0.866025403784439,1.,0.866025403784439,1.,0.866025403784439,
1.,0.866025403784439,1.,0.866025403784439,1.,0.866025403784439,1.,0.866025403784439,
1.,0.866025403784439,1.,0.866025403784439,1.,0.866025403784439,1.,0.866025403784439,
1.,0.866025403784439,1.,0.866025403784439,1.,0.866025403784439,1.,0.866025403784439,
1.,0.866025403784439,1.,0.866025403784439,1.,0.866025403784439,1.,0.866025403784439,
1.,0.866025403784439,1.,0.866025403784439,1.,0.866025403784439,1.,0.866025403784439,
1.,0.866025403784439,1.,0.866025403784439,1.,0.866025403784439,1.,0.866025403784439,
1.,0.866025403784439,1.,0.866025403784439,1.,0.866025403784439,1.,0.866025403784439,
1.,0.866025403784439,1.,0.866025403784439,1.,0.866025403784439,1.,0.866025403784439,
1.,0.866025403784439,1.,0.866025403784439,1.,0.866025403784439,1.,0.866025403784439,
1.,0.866025403784439,1.,0.866025403784439,1.,0.866025403784439,1.,0.866025403784439,
1.,0.866025403784439,1.,0.866025403784439,1.,0.866025403784439,1.,0.866025403784439,
1.,0.866025403784439,1.,0.866025403784439,1.,0.866025403784439,1.,0.866025403784439,
1.,0.866025403784439,1.,0.866025403784439,1.,0.866025403784439,1.,0.866025403784439,
1.,0.866025403784439,1.,0.866025403784439,1.,0.866025403784439,1.,0.866025403784439,
1.,0.866025403784439,1.,0.866025403784439,1.,0.866025403784439,1.,0.866025403784439,
1.,0.866025403784439,1.,0.866025403784439,1.,0.866025403784439,1.,0.866025403784439,
1.,0.866025403784439,1.,0.866025403784439,1.,0.866025403784439,1.,0.866025403784439,
1.,0.866025403784439,1.,0.866025403784439,1.,0.866025403784439,1.,0.866025403784439,
1.,0.866025403784439,1.,0.866025403784439,1.,0.866025403784439,1.,0.866025403784439,
1.,0.866025403784439,1.,0.866025403784439,1.,0.866025403784439,1.,0.866025403784439,
1.,0.866025403784439,1.,0.866025403784439,1.,0.866025403784439,1.,0.866025403784439,
1.,0.866025403784439,1.,0.866025403784439,1.,0.866025403784439,1.,0.866025403784439,
1.,0.866025403784439,1.,0.866025403784439,1.,0.866025403784439,1.,0.866025403784439,
1.,0.866025403784439,1.,0.866025403784439,1.,0.866025403784439,1.,0.866025403784439,
1.,0.866025403784439,1.,0.866025403784439,1.,0.866025403784439,1.,0.866025403784439,
1.,0.866025403784439,1.,0.866025403784439,1.,0.866025403784439,1.,0.866025403784439,
1.,0.866025403784439,1.,0.866025403784439,1.,0.866025403784439,1.,0.866025403784439,
1.,0.866025403784439,1.,0.866025403784439,1.,0.866025403784439,1.,0.866025403784439,
1.,0.866025403784439,1.,0.866025403784439,1.,0.866025403784439,1.,0.866025403784439,
1.,0.866025403784439,1.,0.866025403784439,1.,0.866025403784439,1.,0.866025403784439,
1.,0.866025403784439,1.,0.866025403784439,1.,0.866025403784439,1.,0.866025403784439,
1.,0.866025403784439,1.,0.866025403784439,1.,0.866025403784439,1.,0.866025403784439,
1.,0.866025403784439,1.,0.866025403784439,1.,0.866025403784439,1.,0.866025403784439,
1.,0.866025403784439,1.,0.866025403784439,1.,0.866025403784439,1.,0.866025403784439,
1.,0.866025403784439,1.,0.906090506720528,0.94383273215671))
REPRESENTATION_ITEM('')
);
#203=(
BOUNDED_CURVE()
B_SPLINE_CURVE(2,(#39448,#39449,#39450),.UNSPECIFIED.,.F.,.F.)
B_SPLINE_CURVE_WITH_KNOTS((3,3),(-2.2693844624543,-1.90898280074519),
 .UNSPECIFIED.)
CURVE()
GEOMETRIC_REPRESENTATION_ITEM()
RATIONAL_B_SPLINE_CURVE((1.7477494971405,1.72129587968328,1.68438569901946))
REPRESENTATION_ITEM('')
);
#204=(
BOUNDED_CURVE()
B_SPLINE_CURVE(2,(#39453,#39454,#39455),.UNSPECIFIED.,.F.,.F.)
B_SPLINE_CURVE_WITH_KNOTS((3,3),(-4.45331599749568,-4.09291433578657),
 .UNSPECIFIED.)
CURVE()
GEOMETRIC_REPRESENTATION_ITEM()
RATIONAL_B_SPLINE_CURVE((1.68438569901946,1.72129587968328,1.7477494971405))
REPRESENTATION_ITEM('')
);
#205=(
BOUNDED_CURVE()
B_SPLINE_CURVE(2,(#39462,#39463,#39464),.UNSPECIFIED.,.F.,.F.)
B_SPLINE_CURVE_WITH_KNOTS((3,3),(-2.2693844624543,-1.90898280074519),
 .UNSPECIFIED.)
CURVE()
GEOMETRIC_REPRESENTATION_ITEM()
RATIONAL_B_SPLINE_CURVE((1.7477494971405,1.72129587968328,1.68438569901946))
REPRESENTATION_ITEM('')
);
#206=(
BOUNDED_CURVE()
B_SPLINE_CURVE(2,(#39467,#39468,#39469),.UNSPECIFIED.,.F.,.F.)
B_SPLINE_CURVE_WITH_KNOTS((3,3),(-4.45331599749568,-4.09291433578656),
 .UNSPECIFIED.)
CURVE()
GEOMETRIC_REPRESENTATION_ITEM()
RATIONAL_B_SPLINE_CURVE((1.68438569901946,1.72129587968328,1.7477494971405))
REPRESENTATION_ITEM('')
);
#207=(
BOUNDED_CURVE()
B_SPLINE_CURVE(2,(#39476,#39477,#39478),.UNSPECIFIED.,.F.,.F.)
B_SPLINE_CURVE_WITH_KNOTS((3,3),(-2.2693844624543,-1.90898280074518),
 .UNSPECIFIED.)
CURVE()
GEOMETRIC_REPRESENTATION_ITEM()
RATIONAL_B_SPLINE_CURVE((1.7477494971405,1.72129587968328,1.68438569901946))
REPRESENTATION_ITEM('')
);
#208=(
BOUNDED_CURVE()
B_SPLINE_CURVE(2,(#39481,#39482,#39483),.UNSPECIFIED.,.F.,.F.)
B_SPLINE_CURVE_WITH_KNOTS((3,3),(-4.45331599749568,-4.09291433578656),
 .UNSPECIFIED.)
CURVE()
GEOMETRIC_REPRESENTATION_ITEM()
RATIONAL_B_SPLINE_CURVE((1.68438569901946,1.72129587968328,1.7477494971405))
REPRESENTATION_ITEM('')
);
#209=(
BOUNDED_CURVE()
B_SPLINE_CURVE(2,(#39490,#39491,#39492),.UNSPECIFIED.,.F.,.F.)
B_SPLINE_CURVE_WITH_KNOTS((3,3),(-2.2693844624543,-1.90898280074518),
 .UNSPECIFIED.)
CURVE()
GEOMETRIC_REPRESENTATION_ITEM()
RATIONAL_B_SPLINE_CURVE((1.7477494971405,1.72129587968328,1.68438569901946))
REPRESENTATION_ITEM('')
);
#210=(
BOUNDED_CURVE()
B_SPLINE_CURVE(2,(#39495,#39496,#39497),.UNSPECIFIED.,.F.,.F.)
B_SPLINE_CURVE_WITH_KNOTS((3,3),(-4.45331599749568,-4.09291433578657),
 .UNSPECIFIED.)
CURVE()
GEOMETRIC_REPRESENTATION_ITEM()
RATIONAL_B_SPLINE_CURVE((1.68438569901946,1.72129587968328,1.7477494971405))
REPRESENTATION_ITEM('')
);
#211=(
BOUNDED_CURVE()
B_SPLINE_CURVE(2,(#39504,#39505,#39506),.UNSPECIFIED.,.F.,.F.)
B_SPLINE_CURVE_WITH_KNOTS((3,3),(-4.45331599749568,-4.09291433578656),
 .UNSPECIFIED.)
CURVE()
GEOMETRIC_REPRESENTATION_ITEM()
RATIONAL_B_SPLINE_CURVE((1.68438569901946,1.72129587968328,1.7477494971405))
REPRESENTATION_ITEM('')
);
#212=(
BOUNDED_CURVE()
B_SPLINE_CURVE(2,(#39510,#39511,#39512),.UNSPECIFIED.,.F.,.F.)
B_SPLINE_CURVE_WITH_KNOTS((3,3),(-2.2693844624543,-1.90898280074519),
 .UNSPECIFIED.)
CURVE()
GEOMETRIC_REPRESENTATION_ITEM()
RATIONAL_B_SPLINE_CURVE((1.7477494971405,1.72129587968328,1.68438569901946))
REPRESENTATION_ITEM('')
);
#213=(
BOUNDED_CURVE()
B_SPLINE_CURVE(2,(#39889,#39890,#39891),.UNSPECIFIED.,.F.,.F.)
B_SPLINE_CURVE_WITH_KNOTS((3,3),(0.700862393254458,1.2335087310839),
 .UNSPECIFIED.)
CURVE()
GEOMETRIC_REPRESENTATION_ITEM()
RATIONAL_B_SPLINE_CURVE((1.50938394797057,1.62613520265909,1.62613520265909))
REPRESENTATION_ITEM('')
);
#214=(
BOUNDED_CURVE()
B_SPLINE_CURVE(2,(#39893,#39894,#39895),.UNSPECIFIED.,.F.,.F.)
B_SPLINE_CURVE_WITH_KNOTS((3,3),(1.2335087310839,1.76615506891335),
 .UNSPECIFIED.)
CURVE()
GEOMETRIC_REPRESENTATION_ITEM()
RATIONAL_B_SPLINE_CURVE((1.62613520265909,1.62613520265909,1.50938394797057))
REPRESENTATION_ITEM('')
);
#215=(
BOUNDED_CURVE()
B_SPLINE_CURVE(2,(#39899,#39900,#39901),.UNSPECIFIED.,.F.,.F.)
B_SPLINE_CURVE_WITH_KNOTS((3,3),(-1.2335087310839,-0.70086239325445),
 .UNSPECIFIED.)
CURVE()
GEOMETRIC_REPRESENTATION_ITEM()
RATIONAL_B_SPLINE_CURVE((1.62613520265909,1.62613520265909,1.50938394797057))
REPRESENTATION_ITEM('')
);
#216=(
BOUNDED_CURVE()
B_SPLINE_CURVE(2,(#39902,#39903,#39904),.UNSPECIFIED.,.F.,.F.)
B_SPLINE_CURVE_WITH_KNOTS((3,3),(-1.76615506891334,-1.2335087310839),
 .UNSPECIFIED.)
CURVE()
GEOMETRIC_REPRESENTATION_ITEM()
RATIONAL_B_SPLINE_CURVE((1.50938394797057,1.62613520265909,1.62613520265909))
REPRESENTATION_ITEM('')
);
#217=(
BOUNDED_CURVE()
B_SPLINE_CURVE(2,(#39907,#39908,#39909),.UNSPECIFIED.,.F.,.F.)
B_SPLINE_CURVE_WITH_KNOTS((3,3),(0.700862393254451,1.2335087310839),
 .UNSPECIFIED.)
CURVE()
GEOMETRIC_REPRESENTATION_ITEM()
RATIONAL_B_SPLINE_CURVE((1.50938394797057,1.62613520265909,1.62613520265909))
REPRESENTATION_ITEM('')
);
#218=(
BOUNDED_CURVE()
B_SPLINE_CURVE(2,(#39911,#39912,#39913),.UNSPECIFIED.,.F.,.F.)
B_SPLINE_CURVE_WITH_KNOTS((3,3),(1.2335087310839,1.76615506891334),
 .UNSPECIFIED.)
CURVE()
GEOMETRIC_REPRESENTATION_ITEM()
RATIONAL_B_SPLINE_CURVE((1.62613520265909,1.62613520265909,1.50938394797057))
REPRESENTATION_ITEM('')
);
#219=(
BOUNDED_CURVE()
B_SPLINE_CURVE(2,(#39917,#39918,#39919),.UNSPECIFIED.,.F.,.F.)
B_SPLINE_CURVE_WITH_KNOTS((3,3),(-1.2335087310839,-0.700862393254457),
 .UNSPECIFIED.)
CURVE()
GEOMETRIC_REPRESENTATION_ITEM()
RATIONAL_B_SPLINE_CURVE((1.62613520265909,1.62613520265909,1.50938394797057))
REPRESENTATION_ITEM('')
);
#220=(
BOUNDED_CURVE()
B_SPLINE_CURVE(2,(#39920,#39921,#39922),.UNSPECIFIED.,.F.,.F.)
B_SPLINE_CURVE_WITH_KNOTS((3,3),(-1.76615506891334,-1.2335087310839),
 .UNSPECIFIED.)
CURVE()
GEOMETRIC_REPRESENTATION_ITEM()
RATIONAL_B_SPLINE_CURVE((1.50938394797057,1.62613520265909,1.62613520265909))
REPRESENTATION_ITEM('')
);
#221=(
BOUNDED_CURVE()
B_SPLINE_CURVE(2,(#39926,#39927,#39928),.UNSPECIFIED.,.F.,.F.)
B_SPLINE_CURVE_WITH_KNOTS((3,3),(0.700862393254448,1.2335087310839),
 .UNSPECIFIED.)
CURVE()
GEOMETRIC_REPRESENTATION_ITEM()
RATIONAL_B_SPLINE_CURVE((1.50938394797057,1.62613520265909,1.62613520265909))
REPRESENTATION_ITEM('')
);
#222=(
BOUNDED_CURVE()
B_SPLINE_CURVE(2,(#39932,#39933,#39934),.UNSPECIFIED.,.F.,.F.)
B_SPLINE_CURVE_WITH_KNOTS((3,3),(-1.76615506891334,-1.23350873108389),
 .UNSPECIFIED.)
CURVE()
GEOMETRIC_REPRESENTATION_ITEM()
RATIONAL_B_SPLINE_CURVE((1.50938394797057,1.62613520265909,1.62613520265909))
REPRESENTATION_ITEM('')
);
#223=(
BOUNDED_CURVE()
B_SPLINE_CURVE(2,(#39935,#39936,#39937),.UNSPECIFIED.,.F.,.F.)
B_SPLINE_CURVE_WITH_KNOTS((3,3),(-1.23350873108389,-0.70086239325445),
 .UNSPECIFIED.)
CURVE()
GEOMETRIC_REPRESENTATION_ITEM()
RATIONAL_B_SPLINE_CURVE((1.62613520265909,1.62613520265909,1.50938394797057))
REPRESENTATION_ITEM('')
);
#224=(
BOUNDED_CURVE()
B_SPLINE_CURVE(2,(#39938,#39939,#39940),.UNSPECIFIED.,.F.,.F.)
B_SPLINE_CURVE_WITH_KNOTS((3,3),(1.2335087310839,1.76615506891334),
 .UNSPECIFIED.)
CURVE()
GEOMETRIC_REPRESENTATION_ITEM()
RATIONAL_B_SPLINE_CURVE((1.62613520265909,1.62613520265909,1.50938394797057))
REPRESENTATION_ITEM('')
);
#225=(
BOUNDED_CURVE()
B_SPLINE_CURVE(2,(#39943,#39944,#39945),.UNSPECIFIED.,.F.,.F.)
B_SPLINE_CURVE_WITH_KNOTS((3,3),(0.700862393254458,1.23350873108389),
 .UNSPECIFIED.)
CURVE()
GEOMETRIC_REPRESENTATION_ITEM()
RATIONAL_B_SPLINE_CURVE((1.50938394797057,1.62613520265908,1.62613520265908))
REPRESENTATION_ITEM('')
);
#226=(
BOUNDED_CURVE()
B_SPLINE_CURVE(2,(#39947,#39948,#39949),.UNSPECIFIED.,.F.,.F.)
B_SPLINE_CURVE_WITH_KNOTS((3,3),(1.23350873108389,1.76615506891335),
 .UNSPECIFIED.)
CURVE()
GEOMETRIC_REPRESENTATION_ITEM()
RATIONAL_B_SPLINE_CURVE((1.62613520265908,1.62613520265908,1.50938394797056))
REPRESENTATION_ITEM('')
);
#227=(
BOUNDED_CURVE()
B_SPLINE_CURVE(2,(#39953,#39954,#39955),.UNSPECIFIED.,.F.,.F.)
B_SPLINE_CURVE_WITH_KNOTS((3,3),(-1.23350873108389,-0.700862393254442),
 .UNSPECIFIED.)
CURVE()
GEOMETRIC_REPRESENTATION_ITEM()
RATIONAL_B_SPLINE_CURVE((1.62613520265908,1.62613520265908,1.50938394797056))
REPRESENTATION_ITEM('')
);
#228=(
BOUNDED_CURVE()
B_SPLINE_CURVE(2,(#39956,#39957,#39958),.UNSPECIFIED.,.F.,.F.)
B_SPLINE_CURVE_WITH_KNOTS((3,3),(-1.76615506891333,-1.23350873108389),
 .UNSPECIFIED.)
CURVE()
GEOMETRIC_REPRESENTATION_ITEM()
RATIONAL_B_SPLINE_CURVE((1.50938394797057,1.62613520265908,1.62613520265908))
REPRESENTATION_ITEM('')
);
#229=(
BOUNDED_CURVE()
B_SPLINE_CURVE(2,(#39961,#39962,#39963),.UNSPECIFIED.,.F.,.F.)
B_SPLINE_CURVE_WITH_KNOTS((3,3),(0.700862393254457,1.23350873108389),
 .UNSPECIFIED.)
CURVE()
GEOMETRIC_REPRESENTATION_ITEM()
RATIONAL_B_SPLINE_CURVE((1.50938394797056,1.62613520265908,1.62613520265908))
REPRESENTATION_ITEM('')
);
#230=(
BOUNDED_CURVE()
B_SPLINE_CURVE(2,(#39965,#39966,#39967),.UNSPECIFIED.,.F.,.F.)
B_SPLINE_CURVE_WITH_KNOTS((3,3),(1.23350873108389,1.76615506891333),
 .UNSPECIFIED.)
CURVE()
GEOMETRIC_REPRESENTATION_ITEM()
RATIONAL_B_SPLINE_CURVE((1.62613520265908,1.62613520265908,1.50938394797056))
REPRESENTATION_ITEM('')
);
#231=(
BOUNDED_CURVE()
B_SPLINE_CURVE(2,(#39971,#39972,#39973),.UNSPECIFIED.,.F.,.F.)
B_SPLINE_CURVE_WITH_KNOTS((3,3),(-1.23350873108389,-0.700862393254458),
 .UNSPECIFIED.)
CURVE()
GEOMETRIC_REPRESENTATION_ITEM()
RATIONAL_B_SPLINE_CURVE((1.62613520265908,1.62613520265908,1.50938394797057))
REPRESENTATION_ITEM('')
);
#232=(
BOUNDED_CURVE()
B_SPLINE_CURVE(2,(#39974,#39975,#39976),.UNSPECIFIED.,.F.,.F.)
B_SPLINE_CURVE_WITH_KNOTS((3,3),(-1.76615506891333,-1.23350873108389),
 .UNSPECIFIED.)
CURVE()
GEOMETRIC_REPRESENTATION_ITEM()
RATIONAL_B_SPLINE_CURVE((1.50938394797056,1.62613520265908,1.62613520265908))
REPRESENTATION_ITEM('')
);
#233=(
BOUNDED_CURVE()
B_SPLINE_CURVE(2,(#39979,#39980,#39981),.UNSPECIFIED.,.F.,.F.)
B_SPLINE_CURVE_WITH_KNOTS((3,3),(0.700862393254449,1.2335087310839),
 .UNSPECIFIED.)
CURVE()
GEOMETRIC_REPRESENTATION_ITEM()
RATIONAL_B_SPLINE_CURVE((1.50938394797057,1.62613520265909,1.62613520265909))
REPRESENTATION_ITEM('')
);
#234=(
BOUNDED_CURVE()
B_SPLINE_CURVE(2,(#39982,#39983,#39984),.UNSPECIFIED.,.F.,.F.)
B_SPLINE_CURVE_WITH_KNOTS((3,3),(1.2335087310839,1.76615506891334),
 .UNSPECIFIED.)
CURVE()
GEOMETRIC_REPRESENTATION_ITEM()
RATIONAL_B_SPLINE_CURVE((1.62613520265909,1.62613520265909,1.50938394797057))
REPRESENTATION_ITEM('')
);
#235=(
BOUNDED_CURVE()
B_SPLINE_CURVE(2,(#39986,#39987,#39988),.UNSPECIFIED.,.F.,.F.)
B_SPLINE_CURVE_WITH_KNOTS((3,3),(-1.2335087310839,-0.700862393254449),
 .UNSPECIFIED.)
CURVE()
GEOMETRIC_REPRESENTATION_ITEM()
RATIONAL_B_SPLINE_CURVE((1.62613520265909,1.62613520265909,1.50938394797057))
REPRESENTATION_ITEM('')
);
#236=(
BOUNDED_CURVE()
B_SPLINE_CURVE(2,(#39989,#39990,#39991),.UNSPECIFIED.,.F.,.F.)
B_SPLINE_CURVE_WITH_KNOTS((3,3),(-1.76615506891334,-1.2335087310839),
 .UNSPECIFIED.)
CURVE()
GEOMETRIC_REPRESENTATION_ITEM()
RATIONAL_B_SPLINE_CURVE((1.50938394797057,1.62613520265909,1.62613520265909))
REPRESENTATION_ITEM('')
);
#237=(
BOUNDED_CURVE()
B_SPLINE_CURVE(2,(#40369,#40370,#40371),.UNSPECIFIED.,.F.,.F.)
B_SPLINE_CURVE_WITH_KNOTS((3,3),(-1.35021080745884,-0.79564467090931),
 .UNSPECIFIED.)
CURVE()
GEOMETRIC_REPRESENTATION_ITEM()
RATIONAL_B_SPLINE_CURVE((1.74094633834734,1.74094633834734,1.61595201499016))
REPRESENTATION_ITEM('')
);
#238=(
BOUNDED_CURVE()
B_SPLINE_CURVE(2,(#40372,#40373,#40374),.UNSPECIFIED.,.F.,.F.)
B_SPLINE_CURVE_WITH_KNOTS((3,3),(-1.90477694400836,-1.35021080745884),
 .UNSPECIFIED.)
CURVE()
GEOMETRIC_REPRESENTATION_ITEM()
RATIONAL_B_SPLINE_CURVE((1.61595201499016,1.74094633834734,1.74094633834734))
REPRESENTATION_ITEM('')
);
#239=(
BOUNDED_CURVE()
B_SPLINE_CURVE(2,(#40377,#40378,#40379),.UNSPECIFIED.,.F.,.F.)
B_SPLINE_CURVE_WITH_KNOTS((3,3),(-1.35021080745884,-0.795644670909311),
 .UNSPECIFIED.)
CURVE()
GEOMETRIC_REPRESENTATION_ITEM()
RATIONAL_B_SPLINE_CURVE((1.74094633834734,1.74094633834734,1.61595201499016))
REPRESENTATION_ITEM('')
);
#240=(
BOUNDED_CURVE()
B_SPLINE_CURVE(2,(#40380,#40381,#40382),.UNSPECIFIED.,.F.,.F.)
B_SPLINE_CURVE_WITH_KNOTS((3,3),(-1.90477694400836,-1.35021080745884),
 .UNSPECIFIED.)
CURVE()
GEOMETRIC_REPRESENTATION_ITEM()
RATIONAL_B_SPLINE_CURVE((1.61595201499017,1.74094633834734,1.74094633834734))
REPRESENTATION_ITEM('')
);
#241=(
BOUNDED_CURVE()
B_SPLINE_CURVE(2,(#40385,#40386,#40387),.UNSPECIFIED.,.F.,.F.)
B_SPLINE_CURVE_WITH_KNOTS((3,3),(-1.90477694400836,-1.35021080745884),
 .UNSPECIFIED.)
CURVE()
GEOMETRIC_REPRESENTATION_ITEM()
RATIONAL_B_SPLINE_CURVE((1.61595201499017,1.74094633834734,1.74094633834734))
REPRESENTATION_ITEM('')
);
#242=(
BOUNDED_CURVE()
B_SPLINE_CURVE(2,(#40388,#40389,#40390),.UNSPECIFIED.,.F.,.F.)
B_SPLINE_CURVE_WITH_KNOTS((3,3),(-1.35021080745884,-0.795644670909311),
 .UNSPECIFIED.)
CURVE()
GEOMETRIC_REPRESENTATION_ITEM()
RATIONAL_B_SPLINE_CURVE((1.74094633834735,1.74094633834735,1.61595201499017))
REPRESENTATION_ITEM('')
);
#243=(
BOUNDED_CURVE()
B_SPLINE_CURVE(2,(#40393,#40394,#40395),.UNSPECIFIED.,.F.,.F.)
B_SPLINE_CURVE_WITH_KNOTS((3,3),(-1.90477694400837,-1.35021080745884),
 .UNSPECIFIED.)
CURVE()
GEOMETRIC_REPRESENTATION_ITEM()
RATIONAL_B_SPLINE_CURVE((1.61595201499017,1.74094633834735,1.74094633834735))
REPRESENTATION_ITEM('')
);
#244=(
BOUNDED_CURVE()
B_SPLINE_CURVE(2,(#40396,#40397,#40398),.UNSPECIFIED.,.F.,.F.)
B_SPLINE_CURVE_WITH_KNOTS((3,3),(-1.35021080745884,-0.795644670909312),
 .UNSPECIFIED.)
CURVE()
GEOMETRIC_REPRESENTATION_ITEM()
RATIONAL_B_SPLINE_CURVE((1.74094633834734,1.74094633834734,1.61595201499016))
REPRESENTATION_ITEM('')
);
#245=(
BOUNDED_CURVE()
B_SPLINE_CURVE(2,(#40401,#40402,#40403),.UNSPECIFIED.,.F.,.F.)
B_SPLINE_CURVE_WITH_KNOTS((3,3),(-1.35021080745884,-0.795644670909311),
 .UNSPECIFIED.)
CURVE()
GEOMETRIC_REPRESENTATION_ITEM()
RATIONAL_B_SPLINE_CURVE((1.74094633834734,1.74094633834734,1.61595201499016))
REPRESENTATION_ITEM('')
);
#246=(
BOUNDED_CURVE()
B_SPLINE_CURVE(2,(#40404,#40405,#40406),.UNSPECIFIED.,.F.,.F.)
B_SPLINE_CURVE_WITH_KNOTS((3,3),(-1.90477694400836,-1.35021080745884),
 .UNSPECIFIED.)
CURVE()
GEOMETRIC_REPRESENTATION_ITEM()
RATIONAL_B_SPLINE_CURVE((1.61595201499016,1.74094633834734,1.74094633834734))
REPRESENTATION_ITEM('')
);
#247=(
BOUNDED_CURVE()
B_SPLINE_CURVE(2,(#40409,#40410,#40411),.UNSPECIFIED.,.F.,.F.)
B_SPLINE_CURVE_WITH_KNOTS((3,3),(-1.90477694400833,-1.35021080745884),
 .UNSPECIFIED.)
CURVE()
GEOMETRIC_REPRESENTATION_ITEM()
RATIONAL_B_SPLINE_CURVE((1.61595201499018,1.74094633834734,1.74094633834734))
REPRESENTATION_ITEM('')
);
#248=(
BOUNDED_CURVE()
B_SPLINE_CURVE(2,(#40412,#40413,#40414),.UNSPECIFIED.,.F.,.F.)
B_SPLINE_CURVE_WITH_KNOTS((3,3),(-1.35021080745884,-0.795644670909275),
 .UNSPECIFIED.)
CURVE()
GEOMETRIC_REPRESENTATION_ITEM()
RATIONAL_B_SPLINE_CURVE((1.74094633834734,1.74094633834734,1.61595201499015))
REPRESENTATION_ITEM('')
);
#249=PLANE('',#6475);
#250=PLANE('',#6482);
#251=PLANE('',#6483);
#252=PLANE('',#6484);
#253=PLANE('',#6485);
#254=PLANE('',#6486);
#255=PLANE('',#6487);
#256=PLANE('',#6488);
#257=PLANE('',#6491);
#258=PLANE('',#6493);
#259=PLANE('',#6495);
#260=PLANE('',#6500);
#261=PLANE('',#6504);
#262=PLANE('',#6505);
#263=PLANE('',#6510);
#264=PLANE('',#6512);
#265=PLANE('',#6517);
#266=PLANE('',#6521);
#267=PLANE('',#6522);
#268=PLANE('',#6526);
#269=PLANE('',#6528);
#270=PLANE('',#6530);
#271=PLANE('',#6534);
#272=PLANE('',#6538);
#273=PLANE('',#6539);
#274=PLANE('',#6545);
#275=PLANE('',#6562);
#276=PLANE('',#6563);
#277=PLANE('',#6723);
#278=PLANE('',#6724);
#279=PLANE('',#6725);
#280=PLANE('',#6726);
#281=PLANE('',#6727);
#282=PLANE('',#6728);
#283=PLANE('',#6729);
#284=PLANE('',#6730);
#285=PLANE('',#6731);
#286=PLANE('',#6732);
#287=PLANE('',#6743);
#288=PLANE('',#6796);
#289=PLANE('',#6797);
#290=PLANE('',#6798);
#291=PLANE('',#6799);
#292=PLANE('',#6800);
#293=PLANE('',#6801);
#294=PLANE('',#6802);
#295=PLANE('',#6809);
#296=PLANE('',#6834);
#297=PLANE('',#6835);
#298=PLANE('',#6987);
#299=PLANE('',#6988);
#300=PLANE('',#6989);
#301=PLANE('',#6990);
#302=PLANE('',#6991);
#303=PLANE('',#6992);
#304=PLANE('',#6993);
#305=PLANE('',#6994);
#306=PLANE('',#7007);
#307=PLANE('',#7008);
#308=PLANE('',#7009);
#309=PLANE('',#7010);
#310=PLANE('',#7011);
#311=PLANE('',#7012);
#312=PLANE('',#7013);
#313=PLANE('',#7024);
#314=PLANE('',#7025);
#315=PLANE('',#7026);
#316=PLANE('',#7027);
#317=PLANE('',#7031);
#318=PLANE('',#7032);
#319=PLANE('',#7033);
#320=PLANE('',#7034);
#321=PLANE('',#7035);
#322=PLANE('',#7038);
#323=PLANE('',#7043);
#324=PLANE('',#7046);
#325=PLANE('',#7051);
#326=PLANE('',#7052);
#327=PLANE('',#7053);
#328=PLANE('',#7054);
#329=PLANE('',#7120);
#330=PLANE('',#7124);
#331=PLANE('',#7128);
#332=PLANE('',#7133);
#333=PLANE('',#7134);
#334=PLANE('',#7136);
#335=FACE_BOUND('',#921,.T.);
#336=FACE_BOUND('',#922,.T.);
#337=FACE_BOUND('',#924,.T.);
#338=FACE_BOUND('',#932,.T.);
#339=FACE_BOUND('',#935,.T.);
#340=FACE_BOUND('',#937,.T.);
#341=FACE_BOUND('',#945,.T.);
#342=FACE_BOUND('',#953,.T.);
#343=FACE_BOUND('',#955,.T.);
#344=FACE_BOUND('',#963,.T.);
#345=FACE_BOUND('',#979,.T.);
#346=FACE_BOUND('',#1077,.T.);
#347=FACE_BOUND('',#1079,.T.);
#348=FACE_BOUND('',#1081,.T.);
#349=FACE_BOUND('',#1086,.T.);
#350=FACE_BOUND('',#1094,.T.);
#351=FACE_BOUND('',#1128,.T.);
#352=FACE_BOUND('',#1130,.T.);
#353=FACE_BOUND('',#1147,.T.);
#354=FACE_BOUND('',#1197,.T.);
#355=FACE_BOUND('',#1227,.T.);
#356=FACE_BOUND('',#1230,.T.);
#357=FACE_BOUND('',#1241,.T.);
#358=FACE_BOUND('',#1244,.T.);
#359=FACE_BOUND('',#1268,.T.);
#360=FACE_BOUND('',#1269,.T.);
#361=FACE_BOUND('',#1270,.T.);
#362=FACE_BOUND('',#1271,.T.);
#363=FACE_BOUND('',#1272,.T.);
#364=FACE_BOUND('',#1274,.T.);
#365=FACE_BOUND('',#1275,.T.);
#366=FACE_BOUND('',#1276,.T.);
#367=FACE_BOUND('',#1277,.T.);
#368=FACE_BOUND('',#1278,.T.);
#369=CONICAL_SURFACE('',#6448,8.326,0.785398163397447);
#370=CONICAL_SURFACE('',#6490,8.82600000000001,0.785398163397447);
#371=CONICAL_SURFACE('',#6570,10.9985226280624,1.0471975511966);
#372=CONICAL_SURFACE('',#6571,10.9985226280624,1.0471975511966);
#373=CONICAL_SURFACE('',#6572,10.9985226280624,1.0471975511966);
#374=CONICAL_SURFACE('',#6573,10.9985226280624,1.0471975511966);
#375=CONICAL_SURFACE('',#6574,10.9985226280624,1.0471975511966);
#376=CONICAL_SURFACE('',#6575,10.9985226280624,1.0471975511966);
#377=CONICAL_SURFACE('',#6704,12.7,0.785398163397453);
#378=CONICAL_SURFACE('',#6712,7.4375,0.785398163397444);
#379=CONICAL_SURFACE('',#6713,11.7,0.78539816339744);
#380=CONICAL_SURFACE('',#6733,12.7,0.785398163397453);
#381=CONICAL_SURFACE('',#6735,12.7,0.785398163397453);
#382=CONICAL_SURFACE('',#6737,12.7,0.785398163397453);
#383=CONICAL_SURFACE('',#6739,12.7,0.785398163397453);
#384=CONICAL_SURFACE('',#6741,12.7,0.785398163397453);
#385=CONICAL_SURFACE('',#6755,2.5527,0.959931088596876);
#386=CONICAL_SURFACE('',#6759,3.175,0.959931088596891);
#387=CONICAL_SURFACE('',#6762,2.5527,0.959931088596876);
#388=CONICAL_SURFACE('',#6766,3.175,0.959931088596891);
#389=CONICAL_SURFACE('',#6769,2.5527,0.959931088596876);
#390=CONICAL_SURFACE('',#6773,3.175,0.959931088596891);
#391=CONICAL_SURFACE('',#6776,2.5527,0.959931088596876);
#392=CONICAL_SURFACE('',#6780,3.175,0.959931088596891);
#393=CONICAL_SURFACE('',#6787,3.175,0.95993108859688);
#394=CONICAL_SURFACE('',#6790,2.49047,0.959931088596878);
#395=CONICAL_SURFACE('',#6816,5.55625,0.934531290657969);
#396=CONICAL_SURFACE('',#6817,5.55625,0.934531290657969);
#397=CONICAL_SURFACE('',#6818,5.55625,0.934531290657969);
#398=CONICAL_SURFACE('',#6819,5.55625,0.934531290657969);
#399=CONICAL_SURFACE('',#6820,5.55625,0.934531290657969);
#400=CONICAL_SURFACE('',#6821,5.55625,0.934531290657969);
#401=CONICAL_SURFACE('',#6822,5.55625,0.934531290657969);
#402=CONICAL_SURFACE('',#6823,5.55625,0.934531290657969);
#403=CONICAL_SURFACE('',#6824,5.55625,0.934531290657969);
#404=CONICAL_SURFACE('',#6825,5.55625,0.934531290657969);
#405=CONICAL_SURFACE('',#6826,5.55625,0.934531290657969);
#406=CONICAL_SURFACE('',#6827,5.55625,0.934531290657969);
#407=CONICAL_SURFACE('',#6837,2.41935,0.785398163397442);
#408=CONICAL_SURFACE('',#6841,2.41935,0.959931088596876);
#409=CONICAL_SURFACE('',#6846,3.175,0.959931088596883);
#410=CONICAL_SURFACE('',#6850,2.41935,0.959931088596876);
#411=CONICAL_SURFACE('',#6855,3.175,0.959931088596883);
#412=CONICAL_SURFACE('',#6859,2.41935,0.959931088596876);
#413=CONICAL_SURFACE('',#6864,3.175,0.959931088596883);
#414=CONICAL_SURFACE('',#6868,2.41935,0.959931088596876);
#415=CONICAL_SURFACE('',#6873,3.175,0.959931088596883);
#416=CONICAL_SURFACE('',#6877,2.41935,0.959931088596876);
#417=CONICAL_SURFACE('',#6882,3.175,0.959931088596883);
#418=CONICAL_SURFACE('',#6886,2.41935,0.959931088596876);
#419=CONICAL_SURFACE('',#6891,3.175,0.959931088596883);
#420=CONICAL_SURFACE('',#6895,2.41935,0.959931088596876);
#421=CONICAL_SURFACE('',#6900,3.175,0.959931088596883);
#422=CONICAL_SURFACE('',#6904,2.41935,0.959931088596876);
#423=CONICAL_SURFACE('',#6909,3.175,0.959931088596883);
#424=CONICAL_SURFACE('',#6913,2.41935,0.959931088596876);
#425=CONICAL_SURFACE('',#6918,3.175,0.959931088596883);
#426=CONICAL_SURFACE('',#6922,2.41935,0.959931088596876);
#427=CONICAL_SURFACE('',#6927,3.175,0.959931088596883);
#428=CONICAL_SURFACE('',#6931,2.41935,0.959931088596876);
#429=CONICAL_SURFACE('',#6936,3.175,0.959931088596883);
#430=CONICAL_SURFACE('',#6940,2.41935,0.959931088596876);
#431=CONICAL_SURFACE('',#6945,3.175,0.959931088596883);
#432=CONICAL_SURFACE('',#6949,2.41935,0.959931088596876);
#433=CONICAL_SURFACE('',#6954,3.175,0.959931088596883);
#434=CONICAL_SURFACE('',#6958,2.41935,0.959931088596876);
#435=CONICAL_SURFACE('',#6963,3.175,0.959931088596883);
#436=CONICAL_SURFACE('',#6967,2.41935,0.959931088596876);
#437=CONICAL_SURFACE('',#6972,3.175,0.959931088596883);
#438=CONICAL_SURFACE('',#7001,5.5626,1.0471975511966);
#439=CONICAL_SURFACE('',#7002,5.5626,1.0471975511966);
#440=CONICAL_SURFACE('',#7003,5.5626,1.0471975511966);
#441=CONICAL_SURFACE('',#7004,5.5626,1.0471975511966);
#442=CONICAL_SURFACE('',#7005,5.5626,1.0471975511966);
#443=CONICAL_SURFACE('',#7006,5.5626,1.0471975511966);
#444=CONICAL_SURFACE('',#7074,3.5,0.785398163397436);
#445=CONICAL_SURFACE('',#7078,3.99999999999998,0.785398163397405);
#446=CONICAL_SURFACE('',#7081,3.5,0.785398163397436);
#447=CONICAL_SURFACE('',#7085,4.,0.785398163397429);
#448=CONICAL_SURFACE('',#7088,3.5,0.785398163397436);
#449=CONICAL_SURFACE('',#7092,4.,0.785398163397436);
#450=CONICAL_SURFACE('',#7095,3.49999999999999,0.785398163397435);
#451=CONICAL_SURFACE('',#7099,4.,0.785398163397435);
#452=CONICAL_SURFACE('',#7102,3.49999999999999,0.785398163397435);
#453=CONICAL_SURFACE('',#7106,3.99999999999998,0.785398163397463);
#454=ELLIPSE('',#6439,5.07947085861221,5.00000000004167);
#455=ELLIPSE('',#6446,5.07947085864035,5.00000000005631);
#456=ELLIPSE('',#6492,155.887927744283,31.9541505812655);
#457=ELLIPSE('',#6494,155.887927068924,31.9541505120991);
#458=ELLIPSE('',#6511,155.887927258897,31.9541505315509);
#459=ELLIPSE('',#6527,155.887927546699,31.9541505609938);
#460=ELLIPSE('',#6529,155.887927788136,31.9541505857567);
#461=ELLIPSE('',#6546,155.887926302679,31.9541504336181);
#462=ELLIPSE('',#6707,2.36743243982073,1.24520550947174);
#463=TOROIDAL_SURFACE('',#6422,18.05,1.);
#464=TOROIDAL_SURFACE('',#6427,18.05,1.);
#465=TOROIDAL_SURFACE('',#6432,4.,1.);
#466=TOROIDAL_SURFACE('',#6450,19.55,0.5);
#467=TOROIDAL_SURFACE('',#6453,19.55,0.5);
#468=TOROIDAL_SURFACE('',#6457,19.55,0.5);
#469=TOROIDAL_SURFACE('',#6559,19.55,0.5);
#470=TOROIDAL_SURFACE('',#6560,19.55,0.5);
#471=TOROIDAL_SURFACE('',#6561,19.55,0.5);
#472=TOROIDAL_SURFACE('',#6588,3.,1.);
#473=TOROIDAL_SURFACE('',#6595,3.,1.);
#474=TOROIDAL_SURFACE('',#6597,3.,1.);
#475=TOROIDAL_SURFACE('',#6603,3.,1.);
#476=TOROIDAL_SURFACE('',#6605,3.,1.);
#477=TOROIDAL_SURFACE('',#6611,3.,1.);
#478=TOROIDAL_SURFACE('',#6657,7.35,1.);
#479=TOROIDAL_SURFACE('',#6661,4.,1.);
#480=TOROIDAL_SURFACE('',#6665,4.,1.);
#481=TOROIDAL_SURFACE('',#6669,7.35,1.);
#482=TOROIDAL_SURFACE('',#6672,7.35,1.);
#483=TOROIDAL_SURFACE('',#6676,4.,1.);
#484=TOROIDAL_SURFACE('',#6680,4.,1.);
#485=TOROIDAL_SURFACE('',#6684,7.35,1.);
#486=TOROIDAL_SURFACE('',#6687,7.35,1.);
#487=TOROIDAL_SURFACE('',#6692,4.,1.);
#488=TOROIDAL_SURFACE('',#6696,7.35,1.);
#489=TOROIDAL_SURFACE('',#6973,3.556,0.381);
#490=TOROIDAL_SURFACE('',#7056,16.38,0.5);
#491=TOROIDAL_SURFACE('',#7060,31.26,0.5);
#492=TOROIDAL_SURFACE('',#7065,16.38,0.5);
#493=TOROIDAL_SURFACE('',#7069,31.26,0.5);
#494=TOROIDAL_SURFACE('',#7137,2.5,0.5);
#495=TOROIDAL_SURFACE('',#7143,2.5,0.5);
#496=TOROIDAL_SURFACE('',#7145,7.44,0.5);
#497=TOROIDAL_SURFACE('',#7149,2.5,0.5);
#498=TOROIDAL_SURFACE('',#7155,2.5,0.5);
#499=TOROIDAL_SURFACE('',#7157,7.44,0.5);
#500=FACE_OUTER_BOUND('',#883,.T.);
#501=FACE_OUTER_BOUND('',#884,.T.);
#502=FACE_OUTER_BOUND('',#885,.T.);
#503=FACE_OUTER_BOUND('',#886,.T.);
#504=FACE_OUTER_BOUND('',#887,.T.);
#505=FACE_OUTER_BOUND('',#888,.T.);
#506=FACE_OUTER_BOUND('',#889,.T.);
#507=FACE_OUTER_BOUND('',#890,.T.);
#508=FACE_OUTER_BOUND('',#891,.T.);
#509=FACE_OUTER_BOUND('',#892,.T.);
#510=FACE_OUTER_BOUND('',#893,.T.);
#511=FACE_OUTER_BOUND('',#894,.T.);
#512=FACE_OUTER_BOUND('',#895,.T.);
#513=FACE_OUTER_BOUND('',#896,.T.);
#514=FACE_OUTER_BOUND('',#897,.T.);
#515=FACE_OUTER_BOUND('',#898,.T.);
#516=FACE_OUTER_BOUND('',#899,.T.);
#517=FACE_OUTER_BOUND('',#900,.T.);
#518=FACE_OUTER_BOUND('',#901,.T.);
#519=FACE_OUTER_BOUND('',#902,.T.);
#520=FACE_OUTER_BOUND('',#903,.T.);
#521=FACE_OUTER_BOUND('',#904,.T.);
#522=FACE_OUTER_BOUND('',#905,.T.);
#523=FACE_OUTER_BOUND('',#906,.T.);
#524=FACE_OUTER_BOUND('',#907,.T.);
#525=FACE_OUTER_BOUND('',#908,.T.);
#526=FACE_OUTER_BOUND('',#909,.T.);
#527=FACE_OUTER_BOUND('',#910,.T.);
#528=FACE_OUTER_BOUND('',#911,.T.);
#529=FACE_OUTER_BOUND('',#912,.T.);
#530=FACE_OUTER_BOUND('',#913,.T.);
#531=FACE_OUTER_BOUND('',#914,.T.);
#532=FACE_OUTER_BOUND('',#915,.T.);
#533=FACE_OUTER_BOUND('',#916,.T.);
#534=FACE_OUTER_BOUND('',#917,.T.);
#535=FACE_OUTER_BOUND('',#918,.T.);
#536=FACE_OUTER_BOUND('',#919,.T.);
#537=FACE_OUTER_BOUND('',#920,.T.);
#538=FACE_OUTER_BOUND('',#923,.T.);
#539=FACE_OUTER_BOUND('',#925,.T.);
#540=FACE_OUTER_BOUND('',#926,.T.);
#541=FACE_OUTER_BOUND('',#927,.T.);
#542=FACE_OUTER_BOUND('',#928,.T.);
#543=FACE_OUTER_BOUND('',#929,.T.);
#544=FACE_OUTER_BOUND('',#930,.T.);
#545=FACE_OUTER_BOUND('',#931,.T.);
#546=FACE_OUTER_BOUND('',#933,.T.);
#547=FACE_OUTER_BOUND('',#934,.T.);
#548=FACE_OUTER_BOUND('',#936,.T.);
#549=FACE_OUTER_BOUND('',#938,.T.);
#550=FACE_OUTER_BOUND('',#939,.T.);
#551=FACE_OUTER_BOUND('',#940,.T.);
#552=FACE_OUTER_BOUND('',#941,.T.);
#553=FACE_OUTER_BOUND('',#942,.T.);
#554=FACE_OUTER_BOUND('',#943,.T.);
#555=FACE_OUTER_BOUND('',#944,.T.);
#556=FACE_OUTER_BOUND('',#946,.T.);
#557=FACE_OUTER_BOUND('',#947,.T.);
#558=FACE_OUTER_BOUND('',#948,.T.);
#559=FACE_OUTER_BOUND('',#949,.T.);
#560=FACE_OUTER_BOUND('',#950,.T.);
#561=FACE_OUTER_BOUND('',#951,.T.);
#562=FACE_OUTER_BOUND('',#952,.T.);
#563=FACE_OUTER_BOUND('',#954,.T.);
#564=FACE_OUTER_BOUND('',#956,.T.);
#565=FACE_OUTER_BOUND('',#957,.T.);
#566=FACE_OUTER_BOUND('',#958,.T.);
#567=FACE_OUTER_BOUND('',#959,.T.);
#568=FACE_OUTER_BOUND('',#960,.T.);
#569=FACE_OUTER_BOUND('',#961,.T.);
#570=FACE_OUTER_BOUND('',#962,.T.);
#571=FACE_OUTER_BOUND('',#964,.T.);
#572=FACE_OUTER_BOUND('',#965,.T.);
#573=FACE_OUTER_BOUND('',#966,.T.);
#574=FACE_OUTER_BOUND('',#967,.T.);
#575=FACE_OUTER_BOUND('',#968,.T.);
#576=FACE_OUTER_BOUND('',#969,.T.);
#577=FACE_OUTER_BOUND('',#970,.T.);
#578=FACE_OUTER_BOUND('',#971,.T.);
#579=FACE_OUTER_BOUND('',#972,.T.);
#580=FACE_OUTER_BOUND('',#973,.T.);
#581=FACE_OUTER_BOUND('',#974,.T.);
#582=FACE_OUTER_BOUND('',#975,.T.);
#583=FACE_OUTER_BOUND('',#976,.T.);
#584=FACE_OUTER_BOUND('',#977,.T.);
#585=FACE_OUTER_BOUND('',#978,.T.);
#586=FACE_OUTER_BOUND('',#980,.T.);
#587=FACE_OUTER_BOUND('',#981,.T.);
#588=FACE_OUTER_BOUND('',#982,.T.);
#589=FACE_OUTER_BOUND('',#983,.T.);
#590=FACE_OUTER_BOUND('',#984,.T.);
#591=FACE_OUTER_BOUND('',#985,.T.);
#592=FACE_OUTER_BOUND('',#986,.T.);
#593=FACE_OUTER_BOUND('',#987,.T.);
#594=FACE_OUTER_BOUND('',#988,.T.);
#595=FACE_OUTER_BOUND('',#989,.T.);
#596=FACE_OUTER_BOUND('',#990,.T.);
#597=FACE_OUTER_BOUND('',#991,.T.);
#598=FACE_OUTER_BOUND('',#992,.T.);
#599=FACE_OUTER_BOUND('',#993,.T.);
#600=FACE_OUTER_BOUND('',#994,.T.);
#601=FACE_OUTER_BOUND('',#995,.T.);
#602=FACE_OUTER_BOUND('',#996,.T.);
#603=FACE_OUTER_BOUND('',#997,.T.);
#604=FACE_OUTER_BOUND('',#998,.T.);
#605=FACE_OUTER_BOUND('',#999,.T.);
#606=FACE_OUTER_BOUND('',#1000,.T.);
#607=FACE_OUTER_BOUND('',#1001,.T.);
#608=FACE_OUTER_BOUND('',#1002,.T.);
#609=FACE_OUTER_BOUND('',#1003,.T.);
#610=FACE_OUTER_BOUND('',#1004,.T.);
#611=FACE_OUTER_BOUND('',#1005,.T.);
#612=FACE_OUTER_BOUND('',#1006,.T.);
#613=FACE_OUTER_BOUND('',#1007,.T.);
#614=FACE_OUTER_BOUND('',#1008,.T.);
#615=FACE_OUTER_BOUND('',#1009,.T.);
#616=FACE_OUTER_BOUND('',#1010,.T.);
#617=FACE_OUTER_BOUND('',#1011,.T.);
#618=FACE_OUTER_BOUND('',#1012,.T.);
#619=FACE_OUTER_BOUND('',#1013,.T.);
#620=FACE_OUTER_BOUND('',#1014,.T.);
#621=FACE_OUTER_BOUND('',#1015,.T.);
#622=FACE_OUTER_BOUND('',#1016,.T.);
#623=FACE_OUTER_BOUND('',#1017,.T.);
#624=FACE_OUTER_BOUND('',#1018,.T.);
#625=FACE_OUTER_BOUND('',#1019,.T.);
#626=FACE_OUTER_BOUND('',#1020,.T.);
#627=FACE_OUTER_BOUND('',#1021,.T.);
#628=FACE_OUTER_BOUND('',#1022,.T.);
#629=FACE_OUTER_BOUND('',#1023,.T.);
#630=FACE_OUTER_BOUND('',#1024,.T.);
#631=FACE_OUTER_BOUND('',#1025,.T.);
#632=FACE_OUTER_BOUND('',#1026,.T.);
#633=FACE_OUTER_BOUND('',#1027,.T.);
#634=FACE_OUTER_BOUND('',#1028,.T.);
#635=FACE_OUTER_BOUND('',#1029,.T.);
#636=FACE_OUTER_BOUND('',#1030,.T.);
#637=FACE_OUTER_BOUND('',#1031,.T.);
#638=FACE_OUTER_BOUND('',#1032,.T.);
#639=FACE_OUTER_BOUND('',#1033,.T.);
#640=FACE_OUTER_BOUND('',#1034,.T.);
#641=FACE_OUTER_BOUND('',#1035,.T.);
#642=FACE_OUTER_BOUND('',#1036,.T.);
#643=FACE_OUTER_BOUND('',#1037,.T.);
#644=FACE_OUTER_BOUND('',#1038,.T.);
#645=FACE_OUTER_BOUND('',#1039,.T.);
#646=FACE_OUTER_BOUND('',#1040,.T.);
#647=FACE_OUTER_BOUND('',#1041,.T.);
#648=FACE_OUTER_BOUND('',#1042,.T.);
#649=FACE_OUTER_BOUND('',#1043,.T.);
#650=FACE_OUTER_BOUND('',#1044,.T.);
#651=FACE_OUTER_BOUND('',#1045,.T.);
#652=FACE_OUTER_BOUND('',#1046,.T.);
#653=FACE_OUTER_BOUND('',#1047,.T.);
#654=FACE_OUTER_BOUND('',#1048,.T.);
#655=FACE_OUTER_BOUND('',#1049,.T.);
#656=FACE_OUTER_BOUND('',#1050,.T.);
#657=FACE_OUTER_BOUND('',#1051,.T.);
#658=FACE_OUTER_BOUND('',#1052,.T.);
#659=FACE_OUTER_BOUND('',#1053,.T.);
#660=FACE_OUTER_BOUND('',#1054,.T.);
#661=FACE_OUTER_BOUND('',#1055,.T.);
#662=FACE_OUTER_BOUND('',#1056,.T.);
#663=FACE_OUTER_BOUND('',#1057,.T.);
#664=FACE_OUTER_BOUND('',#1058,.T.);
#665=FACE_OUTER_BOUND('',#1059,.T.);
#666=FACE_OUTER_BOUND('',#1060,.T.);
#667=FACE_OUTER_BOUND('',#1061,.T.);
#668=FACE_OUTER_BOUND('',#1062,.T.);
#669=FACE_OUTER_BOUND('',#1063,.T.);
#670=FACE_OUTER_BOUND('',#1064,.T.);
#671=FACE_OUTER_BOUND('',#1065,.T.);
#672=FACE_OUTER_BOUND('',#1066,.T.);
#673=FACE_OUTER_BOUND('',#1067,.T.);
#674=FACE_OUTER_BOUND('',#1068,.T.);
#675=FACE_OUTER_BOUND('',#1069,.T.);
#676=FACE_OUTER_BOUND('',#1070,.T.);
#677=FACE_OUTER_BOUND('',#1071,.T.);
#678=FACE_OUTER_BOUND('',#1072,.T.);
#679=FACE_OUTER_BOUND('',#1073,.T.);
#680=FACE_OUTER_BOUND('',#1074,.T.);
#681=FACE_OUTER_BOUND('',#1075,.T.);
#682=FACE_OUTER_BOUND('',#1076,.T.);
#683=FACE_OUTER_BOUND('',#1078,.T.);
#684=FACE_OUTER_BOUND('',#1080,.T.);
#685=FACE_OUTER_BOUND('',#1082,.T.);
#686=FACE_OUTER_BOUND('',#1083,.T.);
#687=FACE_OUTER_BOUND('',#1084,.T.);
#688=FACE_OUTER_BOUND('',#1085,.T.);
#689=FACE_OUTER_BOUND('',#1087,.T.);
#690=FACE_OUTER_BOUND('',#1088,.T.);
#691=FACE_OUTER_BOUND('',#1089,.T.);
#692=FACE_OUTER_BOUND('',#1090,.T.);
#693=FACE_OUTER_BOUND('',#1091,.T.);
#694=FACE_OUTER_BOUND('',#1092,.T.);
#695=FACE_OUTER_BOUND('',#1093,.T.);
#696=FACE_OUTER_BOUND('',#1095,.T.);
#697=FACE_OUTER_BOUND('',#1096,.T.);
#698=FACE_OUTER_BOUND('',#1097,.T.);
#699=FACE_OUTER_BOUND('',#1098,.T.);
#700=FACE_OUTER_BOUND('',#1099,.T.);
#701=FACE_OUTER_BOUND('',#1100,.T.);
#702=FACE_OUTER_BOUND('',#1101,.T.);
#703=FACE_OUTER_BOUND('',#1102,.T.);
#704=FACE_OUTER_BOUND('',#1103,.T.);
#705=FACE_OUTER_BOUND('',#1104,.T.);
#706=FACE_OUTER_BOUND('',#1105,.T.);
#707=FACE_OUTER_BOUND('',#1106,.T.);
#708=FACE_OUTER_BOUND('',#1107,.T.);
#709=FACE_OUTER_BOUND('',#1108,.T.);
#710=FACE_OUTER_BOUND('',#1109,.T.);
#711=FACE_OUTER_BOUND('',#1110,.T.);
#712=FACE_OUTER_BOUND('',#1111,.T.);
#713=FACE_OUTER_BOUND('',#1112,.T.);
#714=FACE_OUTER_BOUND('',#1113,.T.);
#715=FACE_OUTER_BOUND('',#1114,.T.);
#716=FACE_OUTER_BOUND('',#1115,.T.);
#717=FACE_OUTER_BOUND('',#1116,.T.);
#718=FACE_OUTER_BOUND('',#1117,.T.);
#719=FACE_OUTER_BOUND('',#1118,.T.);
#720=FACE_OUTER_BOUND('',#1119,.T.);
#721=FACE_OUTER_BOUND('',#1120,.T.);
#722=FACE_OUTER_BOUND('',#1121,.T.);
#723=FACE_OUTER_BOUND('',#1122,.T.);
#724=FACE_OUTER_BOUND('',#1123,.T.);
#725=FACE_OUTER_BOUND('',#1124,.T.);
#726=FACE_OUTER_BOUND('',#1125,.T.);
#727=FACE_OUTER_BOUND('',#1126,.T.);
#728=FACE_OUTER_BOUND('',#1127,.T.);
#729=FACE_OUTER_BOUND('',#1129,.T.);
#730=FACE_OUTER_BOUND('',#1131,.T.);
#731=FACE_OUTER_BOUND('',#1132,.T.);
#732=FACE_OUTER_BOUND('',#1133,.T.);
#733=FACE_OUTER_BOUND('',#1134,.T.);
#734=FACE_OUTER_BOUND('',#1135,.T.);
#735=FACE_OUTER_BOUND('',#1136,.T.);
#736=FACE_OUTER_BOUND('',#1137,.T.);
#737=FACE_OUTER_BOUND('',#1138,.T.);
#738=FACE_OUTER_BOUND('',#1139,.T.);
#739=FACE_OUTER_BOUND('',#1140,.T.);
#740=FACE_OUTER_BOUND('',#1141,.T.);
#741=FACE_OUTER_BOUND('',#1142,.T.);
#742=FACE_OUTER_BOUND('',#1143,.T.);
#743=FACE_OUTER_BOUND('',#1144,.T.);
#744=FACE_OUTER_BOUND('',#1145,.T.);
#745=FACE_OUTER_BOUND('',#1146,.T.);
#746=FACE_OUTER_BOUND('',#1148,.T.);
#747=FACE_OUTER_BOUND('',#1149,.T.);
#748=FACE_OUTER_BOUND('',#1150,.T.);
#749=FACE_OUTER_BOUND('',#1151,.T.);
#750=FACE_OUTER_BOUND('',#1152,.T.);
#751=FACE_OUTER_BOUND('',#1153,.T.);
#752=FACE_OUTER_BOUND('',#1154,.T.);
#753=FACE_OUTER_BOUND('',#1155,.T.);
#754=FACE_OUTER_BOUND('',#1156,.T.);
#755=FACE_OUTER_BOUND('',#1157,.T.);
#756=FACE_OUTER_BOUND('',#1158,.T.);
#757=FACE_OUTER_BOUND('',#1159,.T.);
#758=FACE_OUTER_BOUND('',#1160,.T.);
#759=FACE_OUTER_BOUND('',#1161,.T.);
#760=FACE_OUTER_BOUND('',#1162,.T.);
#761=FACE_OUTER_BOUND('',#1163,.T.);
#762=FACE_OUTER_BOUND('',#1164,.T.);
#763=FACE_OUTER_BOUND('',#1165,.T.);
#764=FACE_OUTER_BOUND('',#1166,.T.);
#765=FACE_OUTER_BOUND('',#1167,.T.);
#766=FACE_OUTER_BOUND('',#1168,.T.);
#767=FACE_OUTER_BOUND('',#1169,.T.);
#768=FACE_OUTER_BOUND('',#1170,.T.);
#769=FACE_OUTER_BOUND('',#1171,.T.);
#770=FACE_OUTER_BOUND('',#1172,.T.);
#771=FACE_OUTER_BOUND('',#1173,.T.);
#772=FACE_OUTER_BOUND('',#1174,.T.);
#773=FACE_OUTER_BOUND('',#1175,.T.);
#774=FACE_OUTER_BOUND('',#1176,.T.);
#775=FACE_OUTER_BOUND('',#1177,.T.);
#776=FACE_OUTER_BOUND('',#1178,.T.);
#777=FACE_OUTER_BOUND('',#1179,.T.);
#778=FACE_OUTER_BOUND('',#1180,.T.);
#779=FACE_OUTER_BOUND('',#1181,.T.);
#780=FACE_OUTER_BOUND('',#1182,.T.);
#781=FACE_OUTER_BOUND('',#1183,.T.);
#782=FACE_OUTER_BOUND('',#1184,.T.);
#783=FACE_OUTER_BOUND('',#1185,.T.);
#784=FACE_OUTER_BOUND('',#1186,.T.);
#785=FACE_OUTER_BOUND('',#1187,.T.);
#786=FACE_OUTER_BOUND('',#1188,.T.);
#787=FACE_OUTER_BOUND('',#1189,.T.);
#788=FACE_OUTER_BOUND('',#1190,.T.);
#789=FACE_OUTER_BOUND('',#1191,.T.);
#790=FACE_OUTER_BOUND('',#1192,.T.);
#791=FACE_OUTER_BOUND('',#1193,.T.);
#792=FACE_OUTER_BOUND('',#1194,.T.);
#793=FACE_OUTER_BOUND('',#1195,.T.);
#794=FACE_OUTER_BOUND('',#1196,.T.);
#795=FACE_OUTER_BOUND('',#1198,.T.);
#796=FACE_OUTER_BOUND('',#1199,.T.);
#797=FACE_OUTER_BOUND('',#1200,.T.);
#798=FACE_OUTER_BOUND('',#1201,.T.);
#799=FACE_OUTER_BOUND('',#1202,.T.);
#800=FACE_OUTER_BOUND('',#1203,.T.);
#801=FACE_OUTER_BOUND('',#1204,.T.);
#802=FACE_OUTER_BOUND('',#1205,.T.);
#803=FACE_OUTER_BOUND('',#1206,.T.);
#804=FACE_OUTER_BOUND('',#1207,.T.);
#805=FACE_OUTER_BOUND('',#1208,.T.);
#806=FACE_OUTER_BOUND('',#1209,.T.);
#807=FACE_OUTER_BOUND('',#1210,.T.);
#808=FACE_OUTER_BOUND('',#1211,.T.);
#809=FACE_OUTER_BOUND('',#1212,.T.);
#810=FACE_OUTER_BOUND('',#1213,.T.);
#811=FACE_OUTER_BOUND('',#1214,.T.);
#812=FACE_OUTER_BOUND('',#1215,.T.);
#813=FACE_OUTER_BOUND('',#1216,.T.);
#814=FACE_OUTER_BOUND('',#1217,.T.);
#815=FACE_OUTER_BOUND('',#1218,.T.);
#816=FACE_OUTER_BOUND('',#1219,.T.);
#817=FACE_OUTER_BOUND('',#1220,.T.);
#818=FACE_OUTER_BOUND('',#1221,.T.);
#819=FACE_OUTER_BOUND('',#1222,.T.);
#820=FACE_OUTER_BOUND('',#1223,.T.);
#821=FACE_OUTER_BOUND('',#1224,.T.);
#822=FACE_OUTER_BOUND('',#1225,.T.);
#823=FACE_OUTER_BOUND('',#1226,.T.);
#824=FACE_OUTER_BOUND('',#1228,.T.);
#825=FACE_OUTER_BOUND('',#1229,.T.);
#826=FACE_OUTER_BOUND('',#1231,.T.);
#827=FACE_OUTER_BOUND('',#1232,.T.);
#828=FACE_OUTER_BOUND('',#1233,.T.);
#829=FACE_OUTER_BOUND('',#1234,.T.);
#830=FACE_OUTER_BOUND('',#1235,.T.);
#831=FACE_OUTER_BOUND('',#1236,.T.);
#832=FACE_OUTER_BOUND('',#1237,.T.);
#833=FACE_OUTER_BOUND('',#1238,.T.);
#834=FACE_OUTER_BOUND('',#1239,.T.);
#835=FACE_OUTER_BOUND('',#1240,.T.);
#836=FACE_OUTER_BOUND('',#1242,.T.);
#837=FACE_OUTER_BOUND('',#1243,.T.);
#838=FACE_OUTER_BOUND('',#1245,.T.);
#839=FACE_OUTER_BOUND('',#1246,.T.);
#840=FACE_OUTER_BOUND('',#1247,.T.);
#841=FACE_OUTER_BOUND('',#1248,.T.);
#842=FACE_OUTER_BOUND('',#1249,.T.);
#843=FACE_OUTER_BOUND('',#1250,.T.);
#844=FACE_OUTER_BOUND('',#1251,.T.);
#845=FACE_OUTER_BOUND('',#1252,.T.);
#846=FACE_OUTER_BOUND('',#1253,.T.);
#847=FACE_OUTER_BOUND('',#1254,.T.);
#848=FACE_OUTER_BOUND('',#1255,.T.);
#849=FACE_OUTER_BOUND('',#1256,.T.);
#850=FACE_OUTER_BOUND('',#1257,.T.);
#851=FACE_OUTER_BOUND('',#1258,.T.);
#852=FACE_OUTER_BOUND('',#1259,.T.);
#853=FACE_OUTER_BOUND('',#1260,.T.);
#854=FACE_OUTER_BOUND('',#1261,.T.);
#855=FACE_OUTER_BOUND('',#1262,.T.);
#856=FACE_OUTER_BOUND('',#1263,.T.);
#857=FACE_OUTER_BOUND('',#1264,.T.);
#858=FACE_OUTER_BOUND('',#1265,.T.);
#859=FACE_OUTER_BOUND('',#1266,.T.);
#860=FACE_OUTER_BOUND('',#1267,.T.);
#861=FACE_OUTER_BOUND('',#1273,.T.);
#862=FACE_OUTER_BOUND('',#1279,.T.);
#863=FACE_OUTER_BOUND('',#1280,.T.);
#864=FACE_OUTER_BOUND('',#1281,.T.);
#865=FACE_OUTER_BOUND('',#1282,.T.);
#866=FACE_OUTER_BOUND('',#1283,.T.);
#867=FACE_OUTER_BOUND('',#1284,.T.);
#868=FACE_OUTER_BOUND('',#1285,.T.);
#869=FACE_OUTER_BOUND('',#1286,.T.);
#870=FACE_OUTER_BOUND('',#1287,.T.);
#871=FACE_OUTER_BOUND('',#1288,.T.);
#872=FACE_OUTER_BOUND('',#1289,.T.);
#873=FACE_OUTER_BOUND('',#1290,.T.);
#874=FACE_OUTER_BOUND('',#1291,.T.);
#875=FACE_OUTER_BOUND('',#1292,.T.);
#876=FACE_OUTER_BOUND('',#1293,.T.);
#877=FACE_OUTER_BOUND('',#1294,.T.);
#878=FACE_OUTER_BOUND('',#1295,.T.);
#879=FACE_OUTER_BOUND('',#1296,.T.);
#880=FACE_OUTER_BOUND('',#1297,.T.);
#881=FACE_OUTER_BOUND('',#1298,.T.);
#882=FACE_OUTER_BOUND('',#1299,.T.);
#883=EDGE_LOOP('',(#3944,#3945,#3946,#3947,#3948,#3949,#3950,#3951));
#884=EDGE_LOOP('',(#3952,#3953,#3954,#3955));
#885=EDGE_LOOP('',(#3956,#3957,#3958,#3959));
#886=EDGE_LOOP('',(#3960,#3961,#3962,#3963));
#887=EDGE_LOOP('',(#3964,#3965,#3966,#3967));
#888=EDGE_LOOP('',(#3968,#3969,#3970,#3971));
#889=EDGE_LOOP('',(#3972,#3973,#3974,#3975));
#890=EDGE_LOOP('',(#3976,#3977,#3978,#3979));
#891=EDGE_LOOP('',(#3980,#3981,#3982,#3983));
#892=EDGE_LOOP('',(#3984,#3985,#3986,#3987));
#893=EDGE_LOOP('',(#3988,#3989,#3990,#3991));
#894=EDGE_LOOP('',(#3992,#3993,#3994,#3995));
#895=EDGE_LOOP('',(#3996,#3997,#3998,#3999));
#896=EDGE_LOOP('',(#4000,#4001,#4002,#4003));
#897=EDGE_LOOP('',(#4004,#4005,#4006,#4007));
#898=EDGE_LOOP('',(#4008,#4009,#4010,#4011));
#899=EDGE_LOOP('',(#4012,#4013,#4014,#4015));
#900=EDGE_LOOP('',(#4016,#4017,#4018,#4019));
#901=EDGE_LOOP('',(#4020,#4021,#4022,#4023));
#902=EDGE_LOOP('',(#4024,#4025,#4026,#4027));
#903=EDGE_LOOP('',(#4028,#4029,#4030,#4031));
#904=EDGE_LOOP('',(#4032,#4033,#4034,#4035));
#905=EDGE_LOOP('',(#4036,#4037,#4038,#4039,#4040));
#906=EDGE_LOOP('',(#4041,#4042,#4043,#4044,#4045));
#907=EDGE_LOOP('',(#4046,#4047,#4048,#4049));
#908=EDGE_LOOP('',(#4050,#4051,#4052,#4053,#4054));
#909=EDGE_LOOP('',(#4055,#4056,#4057,#4058));
#910=EDGE_LOOP('',(#4059,#4060,#4061,#4062));
#911=EDGE_LOOP('',(#4063,#4064,#4065,#4066,#4067));
#912=EDGE_LOOP('',(#4068,#4069,#4070,#4071));
#913=EDGE_LOOP('',(#4072,#4073,#4074,#4075,#4076,#4077,#4078));
#914=EDGE_LOOP('',(#4079,#4080,#4081,#4082,#4083));
#915=EDGE_LOOP('',(#4084,#4085,#4086,#4087));
#916=EDGE_LOOP('',(#4088,#4089,#4090,#4091));
#917=EDGE_LOOP('',(#4092,#4093,#4094,#4095));
#918=EDGE_LOOP('',(#4096,#4097,#4098,#4099));
#919=EDGE_LOOP('',(#4100,#4101,#4102,#4103));
#920=EDGE_LOOP('',(#4104,#4105,#4106,#4107,#4108,#4109,#4110,#4111,#4112,
#4113,#4114,#4115,#4116,#4117));
#921=EDGE_LOOP('',(#4118,#4119,#4120,#4121));
#922=EDGE_LOOP('',(#4122,#4123,#4124,#4125));
#923=EDGE_LOOP('',(#4126,#4127,#4128,#4129,#4130,#4131));
#924=EDGE_LOOP('',(#4132));
#925=EDGE_LOOP('',(#4133,#4134,#4135,#4136,#4137));
#926=EDGE_LOOP('',(#4138,#4139,#4140,#4141,#4142));
#927=EDGE_LOOP('',(#4143,#4144,#4145,#4146,#4147));
#928=EDGE_LOOP('',(#4148,#4149,#4150,#4151,#4152));
#929=EDGE_LOOP('',(#4153,#4154,#4155,#4156,#4157));
#930=EDGE_LOOP('',(#4158,#4159,#4160,#4161,#4162));
#931=EDGE_LOOP('',(#4163));
#932=EDGE_LOOP('',(#4164,#4165,#4166));
#933=EDGE_LOOP('',(#4167,#4168,#4169,#4170,#4171,#4172));
#934=EDGE_LOOP('',(#4173,#4174,#4175,#4176,#4177,#4178));
#935=EDGE_LOOP('',(#4179));
#936=EDGE_LOOP('',(#4180,#4181,#4182,#4183,#4184,#4185));
#937=EDGE_LOOP('',(#4186));
#938=EDGE_LOOP('',(#4187,#4188,#4189,#4190));
#939=EDGE_LOOP('',(#4191,#4192,#4193,#4194));
#940=EDGE_LOOP('',(#4195,#4196,#4197,#4198));
#941=EDGE_LOOP('',(#4199,#4200,#4201,#4202));
#942=EDGE_LOOP('',(#4203,#4204,#4205,#4206));
#943=EDGE_LOOP('',(#4207,#4208,#4209,#4210,#4211,#4212,#4213,#4214));
#944=EDGE_LOOP('',(#4215,#4216,#4217,#4218,#4219,#4220));
#945=EDGE_LOOP('',(#4221));
#946=EDGE_LOOP('',(#4222,#4223,#4224,#4225));
#947=EDGE_LOOP('',(#4226,#4227,#4228,#4229));
#948=EDGE_LOOP('',(#4230,#4231,#4232,#4233));
#949=EDGE_LOOP('',(#4234,#4235,#4236,#4237));
#950=EDGE_LOOP('',(#4238,#4239,#4240,#4241));
#951=EDGE_LOOP('',(#4242,#4243,#4244,#4245,#4246,#4247,#4248,#4249));
#952=EDGE_LOOP('',(#4250,#4251,#4252,#4253,#4254,#4255));
#953=EDGE_LOOP('',(#4256));
#954=EDGE_LOOP('',(#4257,#4258,#4259,#4260,#4261,#4262));
#955=EDGE_LOOP('',(#4263));
#956=EDGE_LOOP('',(#4264,#4265,#4266,#4267));
#957=EDGE_LOOP('',(#4268,#4269,#4270,#4271));
#958=EDGE_LOOP('',(#4272,#4273,#4274,#4275));
#959=EDGE_LOOP('',(#4276,#4277,#4278,#4279));
#960=EDGE_LOOP('',(#4280,#4281,#4282,#4283));
#961=EDGE_LOOP('',(#4284,#4285,#4286,#4287,#4288,#4289,#4290,#4291));
#962=EDGE_LOOP('',(#4292,#4293,#4294,#4295,#4296,#4297));
#963=EDGE_LOOP('',(#4298));
#964=EDGE_LOOP('',(#4299,#4300,#4301,#4302,#4303));
#965=EDGE_LOOP('',(#4304,#4305,#4306,#4307,#4308));
#966=EDGE_LOOP('',(#4309,#4310,#4311,#4312,#4313));
#967=EDGE_LOOP('',(#4314,#4315,#4316,#4317,#4318));
#968=EDGE_LOOP('',(#4319,#4320,#4321,#4322,#4323));
#969=EDGE_LOOP('',(#4324,#4325,#4326,#4327,#4328));
#970=EDGE_LOOP('',(#4329,#4330,#4331,#4332));
#971=EDGE_LOOP('',(#4333,#4334,#4335,#4336,#4337,#4338,#4339));
#972=EDGE_LOOP('',(#4340,#4341,#4342,#4343,#4344,#4345));
#973=EDGE_LOOP('',(#4346,#4347,#4348,#4349,#4350));
#974=EDGE_LOOP('',(#4351,#4352,#4353,#4354,#4355));
#975=EDGE_LOOP('',(#4356,#4357,#4358,#4359,#4360,#4361,#4362,#4363,#4364,
#4365,#4366,#4367,#4368,#4369,#4370,#4371,#4372,#4373,#4374,#4375,#4376,
#4377,#4378,#4379,#4380,#4381,#4382));
#976=EDGE_LOOP('',(#4383,#4384,#4385,#4386,#4387));
#977=EDGE_LOOP('',(#4388,#4389,#4390,#4391,#4392,#4393,#4394,#4395,#4396,
#4397,#4398,#4399,#4400,#4401,#4402,#4403,#4404,#4405,#4406,#4407,#4408,
#4409,#4410,#4411,#4412,#4413));
#978=EDGE_LOOP('',(#4414));
#979=EDGE_LOOP('',(#4415,#4416,#4417,#4418,#4419,#4420,#4421,#4422,#4423,
#4424,#4425,#4426));
#980=EDGE_LOOP('',(#4427,#4428,#4429,#4430));
#981=EDGE_LOOP('',(#4431,#4432,#4433,#4434));
#982=EDGE_LOOP('',(#4435,#4436,#4437,#4438));
#983=EDGE_LOOP('',(#4439,#4440,#4441,#4442));
#984=EDGE_LOOP('',(#4443,#4444,#4445,#4446));
#985=EDGE_LOOP('',(#4447,#4448,#4449,#4450));
#986=EDGE_LOOP('',(#4451,#4452,#4453,#4454));
#987=EDGE_LOOP('',(#4455,#4456,#4457,#4458));
#988=EDGE_LOOP('',(#4459,#4460,#4461,#4462));
#989=EDGE_LOOP('',(#4463,#4464,#4465,#4466));
#990=EDGE_LOOP('',(#4467,#4468,#4469,#4470));
#991=EDGE_LOOP('',(#4471,#4472,#4473,#4474));
#992=EDGE_LOOP('',(#4475,#4476,#4477,#4478));
#993=EDGE_LOOP('',(#4479,#4480,#4481,#4482));
#994=EDGE_LOOP('',(#4483,#4484,#4485,#4486));
#995=EDGE_LOOP('',(#4487,#4488,#4489,#4490));
#996=EDGE_LOOP('',(#4491,#4492,#4493,#4494));
#997=EDGE_LOOP('',(#4495,#4496,#4497,#4498));
#998=EDGE_LOOP('',(#4499,#4500,#4501,#4502));
#999=EDGE_LOOP('',(#4503,#4504,#4505,#4506));
#1000=EDGE_LOOP('',(#4507,#4508,#4509,#4510));
#1001=EDGE_LOOP('',(#4511,#4512,#4513,#4514));
#1002=EDGE_LOOP('',(#4515,#4516,#4517,#4518));
#1003=EDGE_LOOP('',(#4519,#4520,#4521,#4522));
#1004=EDGE_LOOP('',(#4523,#4524,#4525,#4526));
#1005=EDGE_LOOP('',(#4527,#4528,#4529));
#1006=EDGE_LOOP('',(#4530,#4531,#4532,#4533));
#1007=EDGE_LOOP('',(#4534,#4535,#4536));
#1008=EDGE_LOOP('',(#4537,#4538,#4539,#4540));
#1009=EDGE_LOOP('',(#4541,#4542,#4543,#4544));
#1010=EDGE_LOOP('',(#4545,#4546,#4547));
#1011=EDGE_LOOP('',(#4548,#4549,#4550,#4551));
#1012=EDGE_LOOP('',(#4552,#4553,#4554));
#1013=EDGE_LOOP('',(#4555,#4556,#4557,#4558));
#1014=EDGE_LOOP('',(#4559,#4560,#4561));
#1015=EDGE_LOOP('',(#4562,#4563,#4564,#4565));
#1016=EDGE_LOOP('',(#4566,#4567,#4568,#4569));
#1017=EDGE_LOOP('',(#4570,#4571,#4572));
#1018=EDGE_LOOP('',(#4573,#4574,#4575,#4576));
#1019=EDGE_LOOP('',(#4577,#4578,#4579));
#1020=EDGE_LOOP('',(#4580,#4581,#4582,#4583));
#1021=EDGE_LOOP('',(#4584,#4585,#4586));
#1022=EDGE_LOOP('',(#4587,#4588,#4589,#4590));
#1023=EDGE_LOOP('',(#4591,#4592,#4593,#4594));
#1024=EDGE_LOOP('',(#4595,#4596,#4597));
#1025=EDGE_LOOP('',(#4598,#4599,#4600,#4601));
#1026=EDGE_LOOP('',(#4602,#4603,#4604,#4605));
#1027=EDGE_LOOP('',(#4606,#4607,#4608,#4609));
#1028=EDGE_LOOP('',(#4610,#4611,#4612,#4613));
#1029=EDGE_LOOP('',(#4614,#4615,#4616));
#1030=EDGE_LOOP('',(#4617,#4618,#4619));
#1031=EDGE_LOOP('',(#4620,#4621,#4622,#4623));
#1032=EDGE_LOOP('',(#4624,#4625,#4626,#4627));
#1033=EDGE_LOOP('',(#4628,#4629,#4630,#4631));
#1034=EDGE_LOOP('',(#4632,#4633,#4634));
#1035=EDGE_LOOP('',(#4635,#4636,#4637));
#1036=EDGE_LOOP('',(#4638,#4639,#4640,#4641));
#1037=EDGE_LOOP('',(#4642,#4643,#4644,#4645));
#1038=EDGE_LOOP('',(#4646,#4647,#4648));
#1039=EDGE_LOOP('',(#4649,#4650,#4651,#4652));
#1040=EDGE_LOOP('',(#4653,#4654,#4655));
#1041=EDGE_LOOP('',(#4656,#4657,#4658,#4659));
#1042=EDGE_LOOP('',(#4660,#4661,#4662));
#1043=EDGE_LOOP('',(#4663,#4664,#4665,#4666));
#1044=EDGE_LOOP('',(#4667,#4668,#4669,#4670));
#1045=EDGE_LOOP('',(#4671,#4672,#4673,#4674));
#1046=EDGE_LOOP('',(#4675,#4676,#4677,#4678));
#1047=EDGE_LOOP('',(#4679,#4680,#4681,#4682));
#1048=EDGE_LOOP('',(#4683,#4684,#4685,#4686));
#1049=EDGE_LOOP('',(#4687,#4688,#4689,#4690));
#1050=EDGE_LOOP('',(#4691,#4692,#4693));
#1051=EDGE_LOOP('',(#4694,#4695,#4696));
#1052=EDGE_LOOP('',(#4697,#4698,#4699,#4700));
#1053=EDGE_LOOP('',(#4701,#4702,#4703,#4704));
#1054=EDGE_LOOP('',(#4705,#4706,#4707,#4708));
#1055=EDGE_LOOP('',(#4709,#4710,#4711,#4712));
#1056=EDGE_LOOP('',(#4713,#4714,#4715,#4716));
#1057=EDGE_LOOP('',(#4717,#4718,#4719,#4720));
#1058=EDGE_LOOP('',(#4721,#4722,#4723,#4724));
#1059=EDGE_LOOP('',(#4725,#4726,#4727));
#1060=EDGE_LOOP('',(#4728,#4729,#4730));
#1061=EDGE_LOOP('',(#4731,#4732,#4733,#4734));
#1062=EDGE_LOOP('',(#4735,#4736,#4737,#4738));
#1063=EDGE_LOOP('',(#4739,#4740,#4741,#4742));
#1064=EDGE_LOOP('',(#4743,#4744,#4745,#4746));
#1065=EDGE_LOOP('',(#4747,#4748,#4749,#4750));
#1066=EDGE_LOOP('',(#4751,#4752,#4753,#4754));
#1067=EDGE_LOOP('',(#4755,#4756,#4757));
#1068=EDGE_LOOP('',(#4758,#4759,#4760,#4761,#4762,#4763));
#1069=EDGE_LOOP('',(#4764,#4765,#4766,#4767,#4768,#4769));
#1070=EDGE_LOOP('',(#4770,#4771,#4772));
#1071=EDGE_LOOP('',(#4773,#4774,#4775,#4776,#4777,#4778,#4779,#4780,#4781,
#4782));
#1072=EDGE_LOOP('',(#4783,#4784,#4785,#4786,#4787));
#1073=EDGE_LOOP('',(#4788,#4789,#4790,#4791));
#1074=EDGE_LOOP('',(#4792,#4793,#4794,#4795,#4796));
#1075=EDGE_LOOP('',(#4797,#4798,#4799,#4800));
#1076=EDGE_LOOP('',(#4801,#4802,#4803,#4804,#4805,#4806,#4807,#4808,#4809,
#4810,#4811));
#1077=EDGE_LOOP('',(#4812,#4813,#4814,#4815));
#1078=EDGE_LOOP('',(#4816));
#1079=EDGE_LOOP('',(#4817));
#1080=EDGE_LOOP('',(#4818,#4819,#4820));
#1081=EDGE_LOOP('',(#4821));
#1082=EDGE_LOOP('',(#4822,#4823,#4824,#4825));
#1083=EDGE_LOOP('',(#4826,#4827,#4828,#4829));
#1084=EDGE_LOOP('',(#4830,#4831,#4832,#4833));
#1085=EDGE_LOOP('',(#4834,#4835,#4836));
#1086=EDGE_LOOP('',(#4837));
#1087=EDGE_LOOP('',(#4838,#4839,#4840,#4841,#4842,#4843));
#1088=EDGE_LOOP('',(#4844,#4845,#4846,#4847,#4848,#4849));
#1089=EDGE_LOOP('',(#4850,#4851,#4852,#4853,#4854,#4855));
#1090=EDGE_LOOP('',(#4856,#4857,#4858,#4859,#4860,#4861));
#1091=EDGE_LOOP('',(#4862,#4863,#4864,#4865,#4866,#4867));
#1092=EDGE_LOOP('',(#4868,#4869,#4870,#4871,#4872,#4873));
#1093=EDGE_LOOP('',(#4874));
#1094=EDGE_LOOP('',(#4875,#4876,#4877,#4878,#4879,#4880));
#1095=EDGE_LOOP('',(#4881,#4882,#4883));
#1096=EDGE_LOOP('',(#4884,#4885,#4886));
#1097=EDGE_LOOP('',(#4887,#4888,#4889));
#1098=EDGE_LOOP('',(#4890,#4891,#4892));
#1099=EDGE_LOOP('',(#4893,#4894,#4895));
#1100=EDGE_LOOP('',(#4896,#4897,#4898,#4899,#4900,#4901,#4902,#4903,#4904,
#4905,#4906,#4907));
#1101=EDGE_LOOP('',(#4908,#4909,#4910,#4911,#4912,#4913));
#1102=EDGE_LOOP('',(#4914,#4915,#4916,#4917,#4918,#4919));
#1103=EDGE_LOOP('',(#4920,#4921,#4922,#4923));
#1104=EDGE_LOOP('',(#4924,#4925,#4926,#4927));
#1105=EDGE_LOOP('',(#4928,#4929,#4930,#4931,#4932,#4933));
#1106=EDGE_LOOP('',(#4934,#4935,#4936,#4937,#4938));
#1107=EDGE_LOOP('',(#4939,#4940,#4941,#4942,#4943,#4944));
#1108=EDGE_LOOP('',(#4945,#4946,#4947,#4948,#4949));
#1109=EDGE_LOOP('',(#4950,#4951,#4952,#4953,#4954,#4955));
#1110=EDGE_LOOP('',(#4956,#4957,#4958,#4959,#4960));
#1111=EDGE_LOOP('',(#4961,#4962,#4963,#4964,#4965,#4966));
#1112=EDGE_LOOP('',(#4967,#4968,#4969,#4970,#4971));
#1113=EDGE_LOOP('',(#4972,#4973,#4974,#4975,#4976,#4977));
#1114=EDGE_LOOP('',(#4978,#4979,#4980,#4981,#4982));
#1115=EDGE_LOOP('',(#4983,#4984,#4985,#4986,#4987,#4988));
#1116=EDGE_LOOP('',(#4989,#4990,#4991,#4992,#4993));
#1117=EDGE_LOOP('',(#4994,#4995,#4996,#4997,#4998));
#1118=EDGE_LOOP('',(#4999,#5000,#5001,#5002,#5003));
#1119=EDGE_LOOP('',(#5004,#5005,#5006,#5007,#5008));
#1120=EDGE_LOOP('',(#5009,#5010,#5011,#5012,#5013));
#1121=EDGE_LOOP('',(#5014,#5015,#5016,#5017,#5018,#5019));
#1122=EDGE_LOOP('',(#5020,#5021,#5022,#5023,#5024,#5025));
#1123=EDGE_LOOP('',(#5026,#5027,#5028,#5029,#5030,#5031));
#1124=EDGE_LOOP('',(#5032,#5033,#5034,#5035,#5036,#5037));
#1125=EDGE_LOOP('',(#5038,#5039,#5040,#5041,#5042,#5043));
#1126=EDGE_LOOP('',(#5044,#5045,#5046,#5047,#5048,#5049));
#1127=EDGE_LOOP('',(#5050,#5051,#5052,#5053,#5054,#5055));
#1128=EDGE_LOOP('',(#5056));
#1129=EDGE_LOOP('',(#5057,#5058,#5059,#5060,#5061,#5062));
#1130=EDGE_LOOP('',(#5063));
#1131=EDGE_LOOP('',(#5064,#5065,#5066));
#1132=EDGE_LOOP('',(#5067,#5068,#5069));
#1133=EDGE_LOOP('',(#5070,#5071,#5072));
#1134=EDGE_LOOP('',(#5073,#5074,#5075));
#1135=EDGE_LOOP('',(#5076,#5077,#5078));
#1136=EDGE_LOOP('',(#5079,#5080,#5081));
#1137=EDGE_LOOP('',(#5082,#5083,#5084));
#1138=EDGE_LOOP('',(#5085,#5086,#5087));
#1139=EDGE_LOOP('',(#5088,#5089,#5090));
#1140=EDGE_LOOP('',(#5091,#5092,#5093));
#1141=EDGE_LOOP('',(#5094,#5095,#5096));
#1142=EDGE_LOOP('',(#5097,#5098,#5099));
#1143=EDGE_LOOP('',(#5100,#5101,#5102,#5103));
#1144=EDGE_LOOP('',(#5104));
#1145=EDGE_LOOP('',(#5105));
#1146=EDGE_LOOP('',(#5106));
#1147=EDGE_LOOP('',(#5107));
#1148=EDGE_LOOP('',(#5108,#5109,#5110,#5111,#5112));
#1149=EDGE_LOOP('',(#5113,#5114,#5115,#5116,#5117,#5118));
#1150=EDGE_LOOP('',(#5119,#5120,#5121,#5122,#5123,#5124));
#1151=EDGE_LOOP('',(#5125,#5126,#5127,#5128,#5129,#5130));
#1152=EDGE_LOOP('',(#5131,#5132,#5133,#5134,#5135,#5136));
#1153=EDGE_LOOP('',(#5137,#5138,#5139,#5140,#5141,#5142));
#1154=EDGE_LOOP('',(#5143,#5144,#5145,#5146,#5147,#5148));
#1155=EDGE_LOOP('',(#5149,#5150,#5151,#5152,#5153,#5154));
#1156=EDGE_LOOP('',(#5155,#5156,#5157,#5158,#5159,#5160));
#1157=EDGE_LOOP('',(#5161,#5162,#5163,#5164,#5165,#5166));
#1158=EDGE_LOOP('',(#5167,#5168,#5169,#5170,#5171,#5172));
#1159=EDGE_LOOP('',(#5173,#5174,#5175,#5176,#5177,#5178));
#1160=EDGE_LOOP('',(#5179,#5180,#5181,#5182,#5183,#5184));
#1161=EDGE_LOOP('',(#5185,#5186,#5187,#5188,#5189,#5190));
#1162=EDGE_LOOP('',(#5191,#5192,#5193,#5194,#5195,#5196));
#1163=EDGE_LOOP('',(#5197,#5198,#5199,#5200,#5201,#5202));
#1164=EDGE_LOOP('',(#5203,#5204,#5205,#5206,#5207,#5208));
#1165=EDGE_LOOP('',(#5209,#5210,#5211,#5212,#5213,#5214));
#1166=EDGE_LOOP('',(#5215,#5216,#5217,#5218,#5219,#5220));
#1167=EDGE_LOOP('',(#5221,#5222,#5223,#5224,#5225,#5226));
#1168=EDGE_LOOP('',(#5227,#5228,#5229,#5230,#5231,#5232));
#1169=EDGE_LOOP('',(#5233,#5234,#5235,#5236,#5237,#5238));
#1170=EDGE_LOOP('',(#5239,#5240,#5241,#5242,#5243,#5244));
#1171=EDGE_LOOP('',(#5245,#5246,#5247,#5248,#5249,#5250));
#1172=EDGE_LOOP('',(#5251,#5252,#5253,#5254,#5255,#5256));
#1173=EDGE_LOOP('',(#5257,#5258,#5259,#5260,#5261,#5262));
#1174=EDGE_LOOP('',(#5263,#5264,#5265,#5266,#5267,#5268));
#1175=EDGE_LOOP('',(#5269,#5270,#5271,#5272,#5273,#5274));
#1176=EDGE_LOOP('',(#5275,#5276,#5277,#5278,#5279,#5280));
#1177=EDGE_LOOP('',(#5281,#5282,#5283,#5284,#5285,#5286));
#1178=EDGE_LOOP('',(#5287,#5288,#5289,#5290,#5291,#5292));
#1179=EDGE_LOOP('',(#5293,#5294,#5295,#5296,#5297,#5298));
#1180=EDGE_LOOP('',(#5299,#5300,#5301,#5302,#5303,#5304));
#1181=EDGE_LOOP('',(#5305,#5306,#5307,#5308,#5309,#5310));
#1182=EDGE_LOOP('',(#5311,#5312,#5313,#5314,#5315,#5316));
#1183=EDGE_LOOP('',(#5317,#5318,#5319,#5320,#5321,#5322));
#1184=EDGE_LOOP('',(#5323,#5324,#5325,#5326,#5327,#5328));
#1185=EDGE_LOOP('',(#5329,#5330,#5331,#5332,#5333,#5334));
#1186=EDGE_LOOP('',(#5335,#5336,#5337,#5338,#5339,#5340));
#1187=EDGE_LOOP('',(#5341,#5342,#5343,#5344,#5345,#5346));
#1188=EDGE_LOOP('',(#5347,#5348,#5349,#5350,#5351,#5352));
#1189=EDGE_LOOP('',(#5353,#5354,#5355,#5356,#5357,#5358));
#1190=EDGE_LOOP('',(#5359,#5360,#5361,#5362,#5363,#5364));
#1191=EDGE_LOOP('',(#5365,#5366,#5367,#5368,#5369,#5370));
#1192=EDGE_LOOP('',(#5371,#5372,#5373,#5374,#5375,#5376));
#1193=EDGE_LOOP('',(#5377,#5378,#5379,#5380,#5381));
#1194=EDGE_LOOP('',(#5382,#5383,#5384,#5385,#5386,#5387,#5388,#5389,#5390));
#1195=EDGE_LOOP('',(#5391,#5392,#5393,#5394,#5395,#5396));
#1196=EDGE_LOOP('',(#5397));
#1197=EDGE_LOOP('',(#5398));
#1198=EDGE_LOOP('',(#5399,#5400,#5401));
#1199=EDGE_LOOP('',(#5402,#5403,#5404));
#1200=EDGE_LOOP('',(#5405,#5406,#5407));
#1201=EDGE_LOOP('',(#5408,#5409,#5410));
#1202=EDGE_LOOP('',(#5411,#5412,#5413));
#1203=EDGE_LOOP('',(#5414,#5415,#5416));
#1204=EDGE_LOOP('',(#5417,#5418,#5419,#5420,#5421,#5422));
#1205=EDGE_LOOP('',(#5423,#5424,#5425));
#1206=EDGE_LOOP('',(#5426,#5427,#5428));
#1207=EDGE_LOOP('',(#5429,#5430,#5431));
#1208=EDGE_LOOP('',(#5432,#5433,#5434));
#1209=EDGE_LOOP('',(#5435,#5436,#5437));
#1210=EDGE_LOOP('',(#5438,#5439,#5440));
#1211=EDGE_LOOP('',(#5441,#5442,#5443,#5444,#5445,#5446));
#1212=EDGE_LOOP('',(#5447,#5448,#5449,#5450,#5451,#5452));
#1213=EDGE_LOOP('',(#5453,#5454,#5455,#5456,#5457,#5458));
#1214=EDGE_LOOP('',(#5459,#5460,#5461,#5462,#5463,#5464));
#1215=EDGE_LOOP('',(#5465,#5466,#5467,#5468,#5469,#5470));
#1216=EDGE_LOOP('',(#5471,#5472,#5473,#5474,#5475,#5476));
#1217=EDGE_LOOP('',(#5477));
#1218=EDGE_LOOP('',(#5478,#5479,#5480,#5481));
#1219=EDGE_LOOP('',(#5482,#5483,#5484,#5485));
#1220=EDGE_LOOP('',(#5486,#5487,#5488,#5489));
#1221=EDGE_LOOP('',(#5490,#5491,#5492,#5493));
#1222=EDGE_LOOP('',(#5494,#5495,#5496,#5497));
#1223=EDGE_LOOP('',(#5498,#5499,#5500,#5501));
#1224=EDGE_LOOP('',(#5502,#5503,#5504,#5505));
#1225=EDGE_LOOP('',(#5506,#5507,#5508,#5509));
#1226=EDGE_LOOP('',(#5510,#5511,#5512,#5513));
#1227=EDGE_LOOP('',(#5514));
#1228=EDGE_LOOP('',(#5515,#5516,#5517,#5518));
#1229=EDGE_LOOP('',(#5519,#5520,#5521,#5522));
#1230=EDGE_LOOP('',(#5523));
#1231=EDGE_LOOP('',(#5524,#5525,#5526,#5527));
#1232=EDGE_LOOP('',(#5528,#5529,#5530,#5531));
#1233=EDGE_LOOP('',(#5532,#5533,#5534,#5535));
#1234=EDGE_LOOP('',(#5536,#5537,#5538,#5539));
#1235=EDGE_LOOP('',(#5540,#5541,#5542,#5543));
#1236=EDGE_LOOP('',(#5544,#5545,#5546,#5547));
#1237=EDGE_LOOP('',(#5548,#5549,#5550,#5551));
#1238=EDGE_LOOP('',(#5552,#5553,#5554,#5555));
#1239=EDGE_LOOP('',(#5556,#5557,#5558,#5559));
#1240=EDGE_LOOP('',(#5560,#5561,#5562,#5563));
#1241=EDGE_LOOP('',(#5564));
#1242=EDGE_LOOP('',(#5565,#5566,#5567,#5568));
#1243=EDGE_LOOP('',(#5569,#5570,#5571,#5572));
#1244=EDGE_LOOP('',(#5573));
#1245=EDGE_LOOP('',(#5574,#5575,#5576,#5577));
#1246=EDGE_LOOP('',(#5578,#5579,#5580,#5581));
#1247=EDGE_LOOP('',(#5582,#5583,#5584,#5585));
#1248=EDGE_LOOP('',(#5586,#5587,#5588,#5589));
#1249=EDGE_LOOP('',(#5590,#5591,#5592,#5593));
#1250=EDGE_LOOP('',(#5594,#5595,#5596,#5597,#5598));
#1251=EDGE_LOOP('',(#5599,#5600,#5601,#5602));
#1252=EDGE_LOOP('',(#5603,#5604,#5605,#5606,#5607));
#1253=EDGE_LOOP('',(#5608,#5609,#5610,#5611));
#1254=EDGE_LOOP('',(#5612,#5613,#5614,#5615,#5616));
#1255=EDGE_LOOP('',(#5617,#5618,#5619,#5620));
#1256=EDGE_LOOP('',(#5621,#5622,#5623,#5624,#5625));
#1257=EDGE_LOOP('',(#5626,#5627,#5628,#5629));
#1258=EDGE_LOOP('',(#5630,#5631,#5632,#5633,#5634));
#1259=EDGE_LOOP('',(#5635,#5636,#5637,#5638));
#1260=EDGE_LOOP('',(#5639,#5640,#5641,#5642,#5643));
#1261=EDGE_LOOP('',(#5644,#5645,#5646,#5647,#5648));
#1262=EDGE_LOOP('',(#5649,#5650,#5651,#5652,#5653));
#1263=EDGE_LOOP('',(#5654,#5655,#5656,#5657,#5658));
#1264=EDGE_LOOP('',(#5659,#5660,#5661,#5662,#5663));
#1265=EDGE_LOOP('',(#5664,#5665,#5666,#5667));
#1266=EDGE_LOOP('',(#5668,#5669,#5670,#5671));
#1267=EDGE_LOOP('',(#5672,#5673,#5674,#5675,#5676,#5677,#5678,#5679,#5680));
#1268=EDGE_LOOP('',(#5681));
#1269=EDGE_LOOP('',(#5682));
#1270=EDGE_LOOP('',(#5683));
#1271=EDGE_LOOP('',(#5684));
#1272=EDGE_LOOP('',(#5685));
#1273=EDGE_LOOP('',(#5686,#5687,#5688,#5689,#5690,#5691,#5692,#5693,#5694));
#1274=EDGE_LOOP('',(#5695));
#1275=EDGE_LOOP('',(#5696));
#1276=EDGE_LOOP('',(#5697));
#1277=EDGE_LOOP('',(#5698));
#1278=EDGE_LOOP('',(#5699));
#1279=EDGE_LOOP('',(#5700,#5701,#5702,#5703));
#1280=EDGE_LOOP('',(#5704,#5705,#5706,#5707));
#1281=EDGE_LOOP('',(#5708,#5709,#5710,#5711));
#1282=EDGE_LOOP('',(#5712,#5713,#5714,#5715));
#1283=EDGE_LOOP('',(#5716,#5717,#5718,#5719));
#1284=EDGE_LOOP('',(#5720,#5721,#5722,#5723));
#1285=EDGE_LOOP('',(#5724,#5725,#5726,#5727));
#1286=EDGE_LOOP('',(#5728,#5729,#5730,#5731));
#1287=EDGE_LOOP('',(#5732,#5733,#5734,#5735));
#1288=EDGE_LOOP('',(#5736,#5737,#5738,#5739));
#1289=EDGE_LOOP('',(#5740,#5741,#5742,#5743));
#1290=EDGE_LOOP('',(#5744,#5745,#5746,#5747));
#1291=EDGE_LOOP('',(#5748,#5749,#5750,#5751));
#1292=EDGE_LOOP('',(#5752,#5753,#5754,#5755));
#1293=EDGE_LOOP('',(#5756,#5757,#5758,#5759));
#1294=EDGE_LOOP('',(#5760,#5761,#5762,#5763));
#1295=EDGE_LOOP('',(#5764,#5765,#5766,#5767));
#1296=EDGE_LOOP('',(#5768,#5769,#5770,#5771));
#1297=EDGE_LOOP('',(#5772,#5773,#5774,#5775));
#1298=EDGE_LOOP('',(#5776,#5777,#5778,#5779));
#1299=EDGE_LOOP('',(#5780,#5781,#5782,#5783));
#1300=CIRCLE('',#6398,8.326);
#1301=CIRCLE('',#6399,8.326);
#1302=CIRCLE('',#6421,8.326);
#1303=CIRCLE('',#6423,19.05);
#1304=CIRCLE('',#6424,19.05);
#1305=CIRCLE('',#6425,1.);
#1306=CIRCLE('',#6426,18.05);
#1307=CIRCLE('',#6428,18.05);
#1308=CIRCLE('',#6429,1.);
#1309=CIRCLE('',#6430,19.05);
#1310=CIRCLE('',#6431,19.05);
#1311=CIRCLE('',#6433,4.);
#1312=CIRCLE('',#6434,0.999999999999999);
#1313=CIRCLE('',#6435,5.);
#1314=CIRCLE('',#6436,1.);
#1315=CIRCLE('',#6438,5.);
#1316=CIRCLE('',#6441,5.);
#1317=CIRCLE('',#6443,5.);
#1318=CIRCLE('',#6444,5.);
#1319=CIRCLE('',#6447,5.);
#1320=CIRCLE('',#6449,8.82600000000003);
#1321=CIRCLE('',#6451,19.05);
#1322=CIRCLE('',#6452,19.55);
#1323=CIRCLE('',#6454,19.55);
#1324=CIRCLE('',#6455,19.05);
#1325=CIRCLE('',#6456,19.05);
#1326=CIRCLE('',#6458,19.55);
#1327=CIRCLE('',#6459,19.05);
#1328=CIRCLE('',#6462,3.2);
#1329=CIRCLE('',#6463,3.2);
#1330=CIRCLE('',#6465,3.2);
#1331=CIRCLE('',#6466,3.2);
#1332=CIRCLE('',#6468,3.2);
#1333=CIRCLE('',#6469,3.2);
#1334=CIRCLE('',#6471,19.05);
#1335=CIRCLE('',#6472,19.05);
#1336=CIRCLE('',#6473,19.05);
#1337=CIRCLE('',#6474,19.05);
#1338=CIRCLE('',#6476,10.9985226280624);
#1339=CIRCLE('',#6477,10.9985226280624);
#1340=CIRCLE('',#6478,10.9985226280624);
#1341=CIRCLE('',#6479,10.9985226280624);
#1342=CIRCLE('',#6480,10.9985226280624);
#1343=CIRCLE('',#6481,10.9985226280624);
#1344=CIRCLE('',#6489,8.82600000000001);
#1345=CIRCLE('',#6496,19.55);
#1346=CIRCLE('',#6498,3.);
#1347=CIRCLE('',#6499,3.);
#1348=CIRCLE('',#6502,5.);
#1349=CIRCLE('',#6503,5.);
#1350=CIRCLE('',#6506,7.35);
#1351=CIRCLE('',#6507,4.);
#1352=CIRCLE('',#6508,4.);
#1353=CIRCLE('',#6509,7.35);
#1354=CIRCLE('',#6513,19.55);
#1355=CIRCLE('',#6515,3.);
#1356=CIRCLE('',#6516,3.);
#1357=CIRCLE('',#6519,5.);
#1358=CIRCLE('',#6520,5.);
#1359=CIRCLE('',#6523,7.35);
#1360=CIRCLE('',#6524,4.);
#1361=CIRCLE('',#6525,7.35);
#1362=CIRCLE('',#6532,3.);
#1363=CIRCLE('',#6533,3.);
#1364=CIRCLE('',#6536,5.);
#1365=CIRCLE('',#6537,5.);
#1366=CIRCLE('',#6540,19.55);
#1367=CIRCLE('',#6541,7.35);
#1368=CIRCLE('',#6542,4.);
#1369=CIRCLE('',#6543,4.);
#1370=CIRCLE('',#6544,7.35);
#1371=CIRCLE('',#6548,6.35);
#1372=CIRCLE('',#6550,6.35);
#1373=CIRCLE('',#6552,6.35);
#1374=CIRCLE('',#6554,6.35);
#1375=CIRCLE('',#6556,6.35);
#1376=CIRCLE('',#6558,6.35);
#1377=CIRCLE('',#6564,3.);
#1378=CIRCLE('',#6565,3.);
#1379=CIRCLE('',#6566,3.);
#1380=CIRCLE('',#6567,3.);
#1381=CIRCLE('',#6568,3.);
#1382=CIRCLE('',#6569,3.);
#1383=CIRCLE('',#6577,2.);
#1384=CIRCLE('',#6579,2.);
#1385=CIRCLE('',#6581,2.);
#1386=CIRCLE('',#6583,2.);
#1387=CIRCLE('',#6585,2.);
#1388=CIRCLE('',#6587,2.);
#1389=CIRCLE('',#6589,1.);
#1390=CIRCLE('',#6590,1.);
#1391=CIRCLE('',#6592,1.);
#1392=CIRCLE('',#6594,1.);
#1393=CIRCLE('',#6596,1.);
#1394=CIRCLE('',#6598,1.);
#1395=CIRCLE('',#6600,1.);
#1396=CIRCLE('',#6602,1.);
#1397=CIRCLE('',#6604,1.);
#1398=CIRCLE('',#6606,1.);
#1399=CIRCLE('',#6608,1.);
#1400=CIRCLE('',#6610,1.);
#1401=CIRCLE('',#6613,5.);
#1402=CIRCLE('',#6614,5.);
#1403=CIRCLE('',#6616,5.);
#1404=CIRCLE('',#6619,5.);
#1405=CIRCLE('',#6620,5.);
#1406=CIRCLE('',#6622,5.);
#1407=CIRCLE('',#6623,5.);
#1408=CIRCLE('',#6625,5.);
#1409=CIRCLE('',#6628,5.);
#1410=CIRCLE('',#6629,5.);
#1411=CIRCLE('',#6631,5.);
#1412=CIRCLE('',#6632,5.);
#1413=CIRCLE('',#6634,5.);
#1414=CIRCLE('',#6637,5.);
#1415=CIRCLE('',#6638,5.);
#1416=CIRCLE('',#6639,5.);
#1417=CIRCLE('',#6640,5.);
#1418=CIRCLE('',#6645,5.);
#1419=CIRCLE('',#6646,5.);
#1420=CIRCLE('',#6647,5.);
#1421=CIRCLE('',#6648,5.);
#1422=CIRCLE('',#6651,5.);
#1423=CIRCLE('',#6653,5.);
#1424=CIRCLE('',#6655,5.);
#1425=CIRCLE('',#6656,1.);
#1426=CIRCLE('',#6658,1.);
#1427=CIRCLE('',#6660,1.);
#1428=CIRCLE('',#6662,1.);
#1429=CIRCLE('',#6664,1.);
#1430=CIRCLE('',#6666,1.);
#1431=CIRCLE('',#6668,1.);
#1432=CIRCLE('',#6670,1.);
#1433=CIRCLE('',#6671,1.);
#1434=CIRCLE('',#6673,1.);
#1435=CIRCLE('',#6675,1.);
#1436=CIRCLE('',#6677,0.999999999999998);
#1437=CIRCLE('',#6679,1.);
#1438=CIRCLE('',#6681,1.);
#1439=CIRCLE('',#6683,1.);
#1440=CIRCLE('',#6685,1.);
#1441=CIRCLE('',#6686,1.);
#1442=CIRCLE('',#6688,1.);
#1443=CIRCLE('',#6691,1.);
#1444=CIRCLE('',#6693,1.);
#1445=CIRCLE('',#6695,1.);
#1446=CIRCLE('',#6697,0.999999999999999);
#1447=CIRCLE('',#6699,0.5);
#1448=CIRCLE('',#6700,0.5);
#1449=CIRCLE('',#6701,0.500000000000002);
#1450=CIRCLE('',#6702,5.39635281288848);
#1451=CIRCLE('',#6703,0.499999999999999);
#1452=CIRCLE('',#6705,11.7);
#1453=CIRCLE('',#6709,7.4375);
#1454=CIRCLE('',#6710,7.4375);
#1455=CIRCLE('',#6711,7.4375);
#1456=CIRCLE('',#6714,12.7);
#1457=CIRCLE('',#6715,12.7);
#1458=CIRCLE('',#6716,11.7);
#1459=CIRCLE('',#6718,7.70000000000001);
#1460=CIRCLE('',#6719,7.7);
#1461=CIRCLE('',#6721,12.7);
#1462=CIRCLE('',#6722,5.31464415841409);
#1463=CIRCLE('',#6734,11.7);
#1464=CIRCLE('',#6736,11.7);
#1465=CIRCLE('',#6738,11.7);
#1466=CIRCLE('',#6740,11.7);
#1467=CIRCLE('',#6742,11.7);
#1468=CIRCLE('',#6746,4.975);
#1469=CIRCLE('',#6747,4.975);
#1470=CIRCLE('',#6748,4.975);
#1471=CIRCLE('',#6750,4.975);
#1472=CIRCLE('',#6751,4.975);
#1473=CIRCLE('',#6752,4.975);
#1474=CIRCLE('',#6756,2.5527);
#1475=CIRCLE('',#6757,3.175);
#1476=CIRCLE('',#6758,3.175);
#1477=CIRCLE('',#6760,2.5527);
#1478=CIRCLE('',#6761,2.5527);
#1479=CIRCLE('',#6763,2.5527);
#1480=CIRCLE('',#6764,3.175);
#1481=CIRCLE('',#6765,3.175);
#1482=CIRCLE('',#6767,2.5527);
#1483=CIRCLE('',#6768,2.5527);
#1484=CIRCLE('',#6770,2.5527);
#1485=CIRCLE('',#6771,3.175);
#1486=CIRCLE('',#6772,3.175);
#1487=CIRCLE('',#6774,2.5527);
#1488=CIRCLE('',#6775,2.5527);
#1489=CIRCLE('',#6777,2.5527);
#1490=CIRCLE('',#6778,3.175);
#1491=CIRCLE('',#6779,3.175);
#1492=CIRCLE('',#6781,3.15686252031437);
#1493=CIRCLE('',#6782,3.15686252031437);
#1494=CIRCLE('',#6784,3.175);
#1495=CIRCLE('',#6785,3.175);
#1496=CIRCLE('',#6786,3.175);
#1497=CIRCLE('',#6788,2.5527);
#1498=CIRCLE('',#6789,2.5527);
#1499=CIRCLE('',#6791,3.175);
#1500=CIRCLE('',#6803,5.55625);
#1501=CIRCLE('',#6804,5.55625);
#1502=CIRCLE('',#6805,5.55625);
#1503=CIRCLE('',#6806,5.55625);
#1504=CIRCLE('',#6807,5.55625);
#1505=CIRCLE('',#6808,5.55625);
#1506=CIRCLE('',#6810,5.55625);
#1507=CIRCLE('',#6811,5.55625);
#1508=CIRCLE('',#6812,5.55625);
#1509=CIRCLE('',#6813,5.55625);
#1510=CIRCLE('',#6814,5.55625);
#1511=CIRCLE('',#6815,5.55625);
#1512=CIRCLE('',#6830,3.302);
#1513=CIRCLE('',#6831,3.302);
#1514=CIRCLE('',#6833,7.11199999999999);
#1515=CIRCLE('',#6838,3.16631763274988);
#1516=CIRCLE('',#6839,3.16631763274988);
#1517=CIRCLE('',#6840,2.41935);
#1518=CIRCLE('',#6842,3.175);
#1519=CIRCLE('',#6843,3.175);
#1520=CIRCLE('',#6844,2.41935);
#1521=CIRCLE('',#6845,2.41935);
#1522=CIRCLE('',#6848,3.175);
#1523=CIRCLE('',#6849,3.175);
#1524=CIRCLE('',#6851,3.175);
#1525=CIRCLE('',#6852,3.175);
#1526=CIRCLE('',#6853,2.41935);
#1527=CIRCLE('',#6854,2.41935);
#1528=CIRCLE('',#6857,3.175);
#1529=CIRCLE('',#6858,3.175);
#1530=CIRCLE('',#6860,3.175);
#1531=CIRCLE('',#6861,3.175);
#1532=CIRCLE('',#6862,2.41935);
#1533=CIRCLE('',#6863,2.41935);
#1534=CIRCLE('',#6866,3.175);
#1535=CIRCLE('',#6867,3.175);
#1536=CIRCLE('',#6869,3.175);
#1537=CIRCLE('',#6870,3.175);
#1538=CIRCLE('',#6871,2.41935);
#1539=CIRCLE('',#6872,2.41935);
#1540=CIRCLE('',#6875,3.175);
#1541=CIRCLE('',#6876,3.175);
#1542=CIRCLE('',#6878,3.175);
#1543=CIRCLE('',#6879,3.175);
#1544=CIRCLE('',#6880,2.41935);
#1545=CIRCLE('',#6881,2.41935);
#1546=CIRCLE('',#6884,3.175);
#1547=CIRCLE('',#6885,3.175);
#1548=CIRCLE('',#6887,3.175);
#1549=CIRCLE('',#6888,3.175);
#1550=CIRCLE('',#6889,2.41935);
#1551=CIRCLE('',#6890,2.41935);
#1552=CIRCLE('',#6893,3.175);
#1553=CIRCLE('',#6894,3.175);
#1554=CIRCLE('',#6896,3.175);
#1555=CIRCLE('',#6897,3.175);
#1556=CIRCLE('',#6898,2.41935);
#1557=CIRCLE('',#6899,2.41935);
#1558=CIRCLE('',#6902,3.175);
#1559=CIRCLE('',#6903,3.175);
#1560=CIRCLE('',#6905,3.175);
#1561=CIRCLE('',#6906,3.175);
#1562=CIRCLE('',#6907,2.41935);
#1563=CIRCLE('',#6908,2.41935);
#1564=CIRCLE('',#6911,3.175);
#1565=CIRCLE('',#6912,3.175);
#1566=CIRCLE('',#6914,3.175);
#1567=CIRCLE('',#6915,3.175);
#1568=CIRCLE('',#6916,2.41935);
#1569=CIRCLE('',#6917,2.41935);
#1570=CIRCLE('',#6920,3.175);
#1571=CIRCLE('',#6921,3.175);
#1572=CIRCLE('',#6923,3.175);
#1573=CIRCLE('',#6924,3.175);
#1574=CIRCLE('',#6925,2.41935);
#1575=CIRCLE('',#6926,2.41935);
#1576=CIRCLE('',#6929,3.175);
#1577=CIRCLE('',#6930,3.175);
#1578=CIRCLE('',#6932,3.175);
#1579=CIRCLE('',#6933,3.175);
#1580=CIRCLE('',#6934,2.41935);
#1581=CIRCLE('',#6935,2.41935);
#1582=CIRCLE('',#6938,3.175);
#1583=CIRCLE('',#6939,3.175);
#1584=CIRCLE('',#6941,3.175);
#1585=CIRCLE('',#6942,3.175);
#1586=CIRCLE('',#6943,2.41935);
#1587=CIRCLE('',#6944,2.41935);
#1588=CIRCLE('',#6947,3.175);
#1589=CIRCLE('',#6948,3.175);
#1590=CIRCLE('',#6950,3.175);
#1591=CIRCLE('',#6951,3.175);
#1592=CIRCLE('',#6952,2.41935);
#1593=CIRCLE('',#6953,2.41935);
#1594=CIRCLE('',#6956,3.175);
#1595=CIRCLE('',#6957,3.175);
#1596=CIRCLE('',#6959,3.175);
#1597=CIRCLE('',#6960,3.175);
#1598=CIRCLE('',#6961,2.41935);
#1599=CIRCLE('',#6962,2.41935);
#1600=CIRCLE('',#6965,3.175);
#1601=CIRCLE('',#6966,3.175);
#1602=CIRCLE('',#6968,3.175);
#1603=CIRCLE('',#6969,3.175);
#1604=CIRCLE('',#6970,2.41935);
#1605=CIRCLE('',#6971,2.41935);
#1606=CIRCLE('',#6974,3.175);
#1607=CIRCLE('',#6975,3.175);
#1608=CIRCLE('',#6976,0.381);
#1609=CIRCLE('',#6977,3.556);
#1610=CIRCLE('',#6979,5.5626);
#1611=CIRCLE('',#6980,5.5626);
#1612=CIRCLE('',#6981,5.5626);
#1613=CIRCLE('',#6982,5.5626);
#1614=CIRCLE('',#6983,5.5626);
#1615=CIRCLE('',#6984,5.5626);
#1616=CIRCLE('',#6985,5.5626);
#1617=CIRCLE('',#6995,5.5626);
#1618=CIRCLE('',#6996,5.5626);
#1619=CIRCLE('',#6997,5.5626);
#1620=CIRCLE('',#6998,5.5626);
#1621=CIRCLE('',#6999,5.5626);
#1622=CIRCLE('',#7000,5.5626);
#1623=CIRCLE('',#7016,3.175);
#1624=CIRCLE('',#7017,3.175);
#1625=CIRCLE('',#7019,7.94000000000001);
#1626=CIRCLE('',#7020,7.94000000000001);
#1627=CIRCLE('',#7022,3.175);
#1628=CIRCLE('',#7023,3.175);
#1629=CIRCLE('',#7029,7.94000000000001);
#1630=CIRCLE('',#7030,7.94000000000001);
#1631=CIRCLE('',#7036,0.7366);
#1632=CIRCLE('',#7037,7.0866);
#1633=CIRCLE('',#7039,0.7366);
#1634=CIRCLE('',#7040,7.0866);
#1635=CIRCLE('',#7044,7.0866);
#1636=CIRCLE('',#7045,0.7366);
#1637=CIRCLE('',#7047,7.0866);
#1638=CIRCLE('',#7048,0.7366);
#1639=CIRCLE('',#7057,16.38);
#1640=CIRCLE('',#7058,15.88);
#1641=CIRCLE('',#7059,0.5);
#1642=CIRCLE('',#7061,31.76);
#1643=CIRCLE('',#7062,0.500000000000001);
#1644=CIRCLE('',#7063,31.26);
#1645=CIRCLE('',#7064,0.5);
#1646=CIRCLE('',#7066,15.88);
#1647=CIRCLE('',#7067,16.38);
#1648=CIRCLE('',#7068,0.5);
#1649=CIRCLE('',#7070,31.26);
#1650=CIRCLE('',#7071,0.500000000000001);
#1651=CIRCLE('',#7072,31.76);
#1652=CIRCLE('',#7073,0.5);
#1653=CIRCLE('',#7075,3.5);
#1654=CIRCLE('',#7076,3.5);
#1655=CIRCLE('',#7077,4.00000000000003);
#1656=CIRCLE('',#7079,3.5);
#1657=CIRCLE('',#7080,3.99999999999998);
#1658=CIRCLE('',#7082,3.5);
#1659=CIRCLE('',#7083,3.5);
#1660=CIRCLE('',#7084,4.00000000000003);
#1661=CIRCLE('',#7086,3.5);
#1662=CIRCLE('',#7087,4.);
#1663=CIRCLE('',#7089,3.5);
#1664=CIRCLE('',#7090,3.5);
#1665=CIRCLE('',#7091,4.00000000000003);
#1666=CIRCLE('',#7093,3.5);
#1667=CIRCLE('',#7094,4.);
#1668=CIRCLE('',#7096,3.49999999999999);
#1669=CIRCLE('',#7097,3.49999999999999);
#1670=CIRCLE('',#7098,4.00000000000003);
#1671=CIRCLE('',#7100,3.49999999999999);
#1672=CIRCLE('',#7101,4.);
#1673=CIRCLE('',#7103,3.49999999999999);
#1674=CIRCLE('',#7104,3.49999999999999);
#1675=CIRCLE('',#7105,4.00000000000003);
#1676=CIRCLE('',#7107,3.49999999999999);
#1677=CIRCLE('',#7108,3.99999999999998);
#1678=CIRCLE('',#7115,3.);
#1679=CIRCLE('',#7116,3.);
#1680=CIRCLE('',#7118,7.94);
#1681=CIRCLE('',#7119,7.94);
#1682=CIRCLE('',#7121,7.44);
#1683=CIRCLE('',#7122,2.5);
#1684=CIRCLE('',#7123,2.5);
#1685=CIRCLE('',#7125,2.5);
#1686=CIRCLE('',#7126,2.5);
#1687=CIRCLE('',#7127,7.44);
#1688=CIRCLE('',#7131,3.);
#1689=CIRCLE('',#7132,3.);
#1690=CIRCLE('',#7138,0.500000000000002);
#1691=CIRCLE('',#7140,0.500000000000002);
#1692=CIRCLE('',#7142,0.5);
#1693=CIRCLE('',#7144,0.499999999999993);
#1694=CIRCLE('',#7146,0.5);
#1695=CIRCLE('',#7150,0.500000000000002);
#1696=CIRCLE('',#7152,0.500000000000002);
#1697=CIRCLE('',#7154,0.5);
#1698=CIRCLE('',#7156,0.499999999999992);
#1699=CIRCLE('',#7158,0.5);
#1700=B_SPLINE_CURVE_WITH_KNOTS('',3,(#9090,#9091,#9092,#9093,#9094,#9095,
#9096,#9097,#9098,#9099,#9100,#9101,#9102,#9103,#9104,#9105,#9106,#9107,
#9108,#9109,#9110,#9111,#9112,#9113,#9114,#9115,#9116,#9117,#9118,#9119,
#9120,#9121,#9122,#9123,#9124,#9125),.UNSPECIFIED.,.F.,.F.,(4,2,2,2,2,2,
2,2,2,2,2,2,2,2,2,2,2,4),(112.722377729167,112.935814461693,113.265902169001,
113.583624527612,113.914511948724,114.240430230342,114.556670232197,114.887643864478,
115.209930389785,115.530836781107,115.86192664675,116.180533848522,116.512423873419,
116.839241033721,117.155181879653,117.486063018035,117.671271477257,117.853108376992),
 .UNSPECIFIED.);
#1701=B_SPLINE_CURVE_WITH_KNOTS('',3,(#9129,#9130,#9131,#9132,#9133,#9134,
#9135,#9136),.UNSPECIFIED.,.F.,.F.,(4,2,2,4),(1.00000004377154E-6,0.311560962486637,
0.633359069276319,0.894813729390518),.UNSPECIFIED.);
#1702=B_SPLINE_CURVE_WITH_KNOTS('',3,(#9140,#9141,#9142,#9143,#9144,#9145,
#9146,#9147,#9148,#9149,#9150,#9151,#9152,#9153,#9154,#9155,#9156,#9157,
#9158,#9159,#9160,#9161,#9162,#9163,#9164,#9165,#9166,#9167,#9168,#9169,
#9170,#9171,#9172,#9173,#9174,#9175),.UNSPECIFIED.,.F.,.F.,(4,2,2,2,2,2,
2,2,2,2,2,2,2,2,2,2,2,4),(0.894813729390518,0.961776507644016,1.28158051477554,
1.61400438298121,1.93318237682149,2.25667496672185,2.5877852199457,2.90394552078605,
3.23108964694769,3.56286934127997,3.88178044788897,4.21319355178493,4.53413520601621,
4.85672792330627,5.1879222585641,5.50433651680187,5.83056456912644,6.14552138395939),
 .UNSPECIFIED.);
#1703=B_SPLINE_CURVE_WITH_KNOTS('',3,(#9180,#9181,#9182,#9183,#9184,#9185,
#9186,#9187,#9188,#9189,#9190,#9191,#9192,#9193,#9194,#9195,#9196,#9197,
#9198,#9199,#9200,#9201,#9202,#9203,#9204,#9205,#9206,#9207,#9208,#9209,
#9210,#9211,#9212,#9213,#9214,#9215),.UNSPECIFIED.,.F.,.F.,(4,2,2,2,2,2,
2,2,2,2,2,2,2,2,2,2,2,4),(107.474251326802,107.742071039885,108.06977773657,
108.385852662872,108.716717431421,109.040756337916,109.358660344358,109.691706511941,
110.012041848036,110.33795465052,110.666813251939,110.983551519639,111.314497909285,
111.639657257904,111.956665800719,112.290935661215,112.612354232963,112.722377729167),
 .UNSPECIFIED.);
#1704=B_SPLINE_CURVE_WITH_KNOTS('',3,(#9216,#9217,#9218,#9219,#9220,#9221,
#9222,#9223,#9224,#9225,#9226,#9227,#9228,#9229,#9230,#9231,#9232,#9233,
#9234,#9235,#9236,#9237,#9238,#9239,#9240,#9241,#9242,#9243,#9244,#9245,
#9246,#9247,#9248,#9249,#9250,#9251,#9252,#9253),.UNSPECIFIED.,.F.,.F.,
(4,2,2,2,2,2,2,2,2,2,2,2,2,2,2,2,2,2,4),(6.14552138395939,6.1616825653315,
6.47970395444461,6.8101094302656,7.1335439556076,7.45526154677082,7.7898524160329,
8.10698412287342,8.43244913677209,8.76360062205182,9.08061784409396,9.40978773389439,
9.73561249179691,10.0562385787091,10.3895966470178,10.7075686732502,11.0319035622572,
11.3629629626413,11.3974419742764),.UNSPECIFIED.);
#1705=B_SPLINE_CURVE_WITH_KNOTS('',3,(#9258,#9259,#9260,#9261,#9262,#9263,
#9264,#9265,#9266,#9267,#9268,#9269,#9270,#9271,#9272,#9273,#9274,#9275,
#9276,#9277,#9278,#9279,#9280,#9281,#9282,#9283,#9284,#9285,#9286,#9287,
#9288,#9289,#9290,#9291,#9292,#9293),.UNSPECIFIED.,.F.,.F.,(4,2,2,2,2,2,
2,2,2,2,2,2,2,2,2,2,2,4),(102.227174401341,102.547743819964,102.873542639389,
103.189851102933,103.520835959175,103.843004394828,104.164180871344,104.495136940484,
104.813625411964,105.146003499125,105.472676947349,105.78862297816,106.119503302266,
106.442532643452,106.761857523774,107.09378555739,107.413132348819,107.474251326802),
 .UNSPECIFIED.);
#1706=B_SPLINE_CURVE_WITH_KNOTS('',3,(#9294,#9295,#9296,#9297,#9298,#9299,
#9300,#9301,#9302,#9303,#9304,#9305,#9306,#9307,#9308,#9309,#9310,#9311,
#9312,#9313,#9314,#9315,#9316,#9317,#9318,#9319,#9320,#9321,#9322,#9323,
#9324,#9325,#9326,#9327,#9328,#9329),.UNSPECIFIED.,.F.,.F.,(4,2,2,2,2,2,
2,2,2,2,2,2,2,2,2,2,2,4),(11.3974419742764,11.6792630801897,12.00727075871,
12.3360711634136,12.6556969312119,12.9879236571427,13.3072671073346,13.6305788486675,
13.9616444153745,14.2777621917807,14.6047221098277,14.9369312253169,15.2556834570718,
15.5869211480732,15.9080804574186,16.2305142097752,16.5616756401567,16.6472530619074),
 .UNSPECIFIED.);
#1707=B_SPLINE_CURVE_WITH_KNOTS('',3,(#9334,#9335,#9336,#9337,#9338,#9339,
#9340,#9341,#9342,#9343,#9344,#9345,#9346,#9347,#9348,#9349,#9350,#9351,
#9352,#9353,#9354,#9355,#9356,#9357,#9358,#9359,#9360,#9361,#9362,#9363,
#9364,#9365,#9366,#9367,#9368,#9369,#9370,#9371),.UNSPECIFIED.,.F.,.F.,
(4,2,2,2,2,2,2,2,2,2,2,2,2,2,2,2,2,2,4),(96.9781059936184,97.0189343553572,
97.349846603863,97.673784838871,97.9919085061954,98.3248402945117,98.6450784360225,
98.9714378399046,99.3001783979141,99.6168395678662,99.9478190660389,100.272864605671,
100.590015158421,100.924158382915,101.245468653185,101.569287291419,101.899248610767,
102.216858851709,102.227174401341),.UNSPECIFIED.);
#1708=B_SPLINE_CURVE_WITH_KNOTS('',3,(#9372,#9373,#9374,#9375,#9376,#9377,
#9378,#9379,#9380,#9381,#9382,#9383,#9384,#9385,#9386,#9387,#9388,#9389,
#9390,#9391,#9392,#9393,#9394,#9395,#9396,#9397,#9398,#9399,#9400,#9401,
#9402,#9403,#9404,#9405,#9406,#9407),.UNSPECIFIED.,.F.,.F.,(4,2,2,2,2,2,
2,2,2,2,2,2,2,2,2,2,2,4),(16.6472530619074,16.8781103297922,17.2041774694477,
17.5352488180356,17.8531174701921,18.1833544127834,18.5070934055145,18.8286613021236,
19.1630825685098,19.4803064183847,19.8056156297394,20.1367557994998,20.4536485378793,
20.7826578839162,21.108875414935,21.4293624838375,21.7625626929516,21.8990645150227),
 .UNSPECIFIED.);
#1709=B_SPLINE_CURVE_WITH_KNOTS('',3,(#9412,#9413,#9414,#9415,#9416,#9417,
#9418,#9419,#9420,#9421,#9422,#9423,#9424,#9425,#9426,#9427,#9428,#9429,
#9430,#9431,#9432,#9433,#9434,#9435,#9436,#9437,#9438,#9439,#9440,#9441,
#9442,#9443,#9444,#9445,#9446,#9447),.UNSPECIFIED.,.F.,.F.,(4,2,2,2,2,2,
2,2,2,2,2,2,2,2,2,2,2,4),(91.7303443229,91.8216652436239,92.1527227435167,
92.4748328043334,92.7963468711931,93.1272302292321,93.4456586663009,93.7785962802266,
94.1051857365978,94.4212037762885,94.7521445950755,95.0750919614189,95.394705394427,
95.7265371665394,96.0458029110323,96.3752586155109,96.7028613061121,96.9781059936184),
 .UNSPECIFIED.);
#1710=B_SPLINE_CURVE_WITH_KNOTS('',3,(#9448,#9449,#9450,#9451,#9452,#9453,
#9454,#9455,#9456,#9457,#9458,#9459,#9460,#9461,#9462,#9463,#9464,#9465,
#9466,#9467,#9468,#9469,#9470,#9471,#9472,#9473,#9474,#9475,#9476,#9477,
#9478,#9479,#9480,#9481,#9482,#9483),.UNSPECIFIED.,.F.,.F.,(4,2,2,2,2,2,
2,2,2,2,2,2,2,2,2,2,2,4),(21.8990645150227,22.080704098049,22.404895807676,
22.7359583196053,23.052208146303,23.3800687533882,23.7093337294194,24.0288361082048,
24.3609225018898,24.6805048958586,25.0036915857874,25.3347732880507,25.6509147409374,
25.9777469929682,26.310465518035,26.6291148632443,26.9602352134497,27.1490940819086),
 .UNSPECIFIED.);
#1711=B_SPLINE_CURVE_WITH_KNOTS('',3,(#9488,#9489,#9490,#9491,#9492,#9493,
#9494,#9495,#9496,#9497,#9498,#9499,#9500,#9501,#9502,#9503,#9504,#9505,
#9506,#9507,#9508,#9509,#9510,#9511,#9512,#9513,#9514,#9515,#9516,#9517,
#9518,#9519,#9520,#9521,#9522,#9523),.UNSPECIFIED.,.F.,.F.,(4,2,2,2,2,2,
2,2,2,2,2,2,2,2,2,2,2,4),(86.4798314140111,86.6227800760488,86.9556609508597,
87.2758626652495,87.6027341887179,87.9314188779159,88.2480710512407,88.5791451872703,
88.904138285101,89.2214976252686,89.5555772220635,89.8768395886157,90.2010842871321,
90.5309809091133,90.848538274585,91.1794826620175,91.5052225752388,91.7303443229),
 .UNSPECIFIED.);
#1712=B_SPLINE_CURVE_WITH_KNOTS('',3,(#9524,#9525,#9526,#9527,#9528,#9529,
#9530,#9531,#9532,#9533,#9534,#9535,#9536,#9537,#9538,#9539,#9540,#9541,
#9542,#9543,#9544,#9545,#9546,#9547,#9548,#9549,#9550,#9551,#9552,#9553,
#9554,#9555,#9556,#9557,#9558,#9559),.UNSPECIFIED.,.F.,.F.,(4,2,2,2,2,2,
2,2,2,2,2,2,2,2,2,2,2,4),(27.1490940819086,27.2816841559646,27.6040159460672,
27.935205618183,28.2517271794494,28.5776912122136,28.9087772011457,29.2265497511765,
29.5566769523901,29.8807942522771,30.2022702407119,30.5365819291874,30.8539667784873,
31.1791788250368,31.5103692663226,31.82720356108,32.1561117178664,32.4014535157498),
 .UNSPECIFIED.);
#1713=B_SPLINE_CURVE_WITH_KNOTS('',3,(#9564,#9565,#9566,#9567,#9568,#9569,
#9570,#9571,#9572,#9573,#9574,#9575,#9576,#9577,#9578,#9579,#9580,#9581,
#9582,#9583,#9584,#9585,#9586,#9587,#9588,#9589,#9590,#9591,#9592,#9593,
#9594,#9595,#9596,#9597,#9598,#9599),.UNSPECIFIED.,.F.,.F.,(4,2,2,2,2,2,
2,2,2,2,2,2,2,2,2,2,2,4),(81.2303172007343,81.4251321858443,81.7560069702517,
82.0744367502896,82.4079916863948,82.7345602143883,83.0507161535853,83.3817783439728,
83.7047059180943,84.0246708033549,84.3564702037923,84.6757160394563,85.0057507119943,
85.3333120660503,85.6494509767062,85.9804718601221,86.3043712286969,86.4798314140111),
 .UNSPECIFIED.);
#1714=B_SPLINE_CURVE_WITH_KNOTS('',3,(#9600,#9601,#9602,#9603,#9604,#9605,
#9606,#9607,#9608,#9609,#9610,#9611,#9612,#9613,#9614,#9615,#9616,#9617,
#9618,#9619,#9620,#9621,#9622,#9623,#9624,#9625,#9626,#9627,#9628,#9629,
#9630,#9631,#9632,#9633,#9634,#9635),.UNSPECIFIED.,.F.,.F.,(4,2,2,2,2,2,
2,2,2,2,2,2,2,2,2,2,2,4),(32.4014535157498,32.4827954803396,32.8032018866308,
33.1363049419288,33.4546849111464,33.7787927583837,34.1099198526596,34.4261866157241,
34.7539602528262,35.0837611091104,35.4031991295255,35.735206665648,36.0550960135157,
36.3782177053124,36.709376966425,37.0256089756814,37.352374450904,37.6524303097187),
 .UNSPECIFIED.);
#1715=B_SPLINE_CURVE_WITH_KNOTS('',3,(#9640,#9641,#9642,#9643,#9644,#9645,
#9646,#9647,#9648,#9649,#9650,#9651,#9652,#9653,#9654,#9655,#9656,#9657,
#9658,#9659,#9660,#9661,#9662,#9663,#9664,#9665,#9666,#9667,#9668,#9669,
#9670,#9671,#9672,#9673,#9674,#9675),.UNSPECIFIED.,.F.,.F.,(4,2,2,2,2,2,
2,2,2,2,2,2,2,2,2,2,2,4),(75.9777376249721,76.2296477532921,76.5583412626286,
76.8750533353474,77.2062822942674,77.531286732469,77.8489168802109,78.1829985904649,
78.5042757431245,78.8290038626106,79.158900305632,79.4764665215315,79.8075318515091,
80.1332760850523,80.4499160587139,80.7811068885252,81.1032209347659,81.2303172007343),
 .UNSPECIFIED.);
#1716=B_SPLINE_CURVE_WITH_KNOTS('',3,(#9676,#9677,#9678,#9679,#9680,#9681,
#9682,#9683,#9684,#9685,#9686,#9687,#9688,#9689,#9690,#9691,#9692,#9693,
#9694,#9695,#9696,#9697,#9698,#9699,#9700,#9701,#9702,#9703,#9704,#9705,
#9706,#9707,#9708,#9709,#9710,#9711,#9712,#9713),.UNSPECIFIED.,.F.,.F.,
(4,2,2,2,2,2,2,2,2,2,2,2,2,2,2,2,2,2,4),(37.6524303097187,37.6856703367532,
38.0042764730292,38.3353416640884,38.6571458291731,38.9794363498445,39.3107157137369,
39.6273894493943,39.9533119208669,40.2844745667797,40.6022111901814,40.932291381766,
41.256852033589,41.5782973531143,41.9125634479899,42.2301750011463,42.5553521316008,
42.886654185985,42.9060171593307),.UNSPECIFIED.);
#1717=B_SPLINE_CURVE_WITH_KNOTS('',3,(#9718,#9719,#9720,#9721,#9722,#9723,
#9724,#9725,#9726,#9727,#9728,#9729,#9730,#9731,#9732,#9733,#9734,#9735,
#9736,#9737,#9738,#9739,#9740,#9741,#9742,#9743,#9744,#9745,#9746,#9747,
#9748,#9749,#9750,#9751,#9752,#9753),.UNSPECIFIED.,.F.,.F.,(4,2,2,2,2,2,
2,2,2,2,2,2,2,2,2,2,2,4),(70.7257701778119,71.0320289658823,71.3586411516273,
71.6749977042479,72.0062401831685,72.3292116408242,72.6495824341981,72.981415199054,
73.3007037729756,73.6313652344112,73.9589500206666,74.2752212361238,74.60641024243,
74.9303345803813,75.2490873252793,75.5819831233109,75.902211150012,75.9777376249721),
 .UNSPECIFIED.);
#1718=B_SPLINE_CURVE_WITH_KNOTS('',3,(#9754,#9755,#9756,#9757,#9758,#9759,
#9760,#9761,#9762,#9763,#9764,#9765,#9766,#9767,#9768,#9769,#9770,#9771,
#9772,#9773,#9774,#9775,#9776,#9777,#9778,#9779,#9780,#9781,#9782,#9783,
#9784,#9785,#9786,#9787,#9788,#9789),.UNSPECIFIED.,.F.,.F.,(4,2,2,2,2,2,
2,2,2,2,2,2,2,2,2,2,2,4),(42.9060171593307,43.2034986491151,43.5323687043631,
43.8595809104928,44.1799681785184,44.5130384264816,44.8317208112402,45.1558073806985,
45.4870599295524,45.8034112826383,46.1311614264702,46.4615563210303,46.7809917528282,
47.1129850599791,47.4332420968641,47.7563616063971,48.0876589350017,48.1589956367661),
 .UNSPECIFIED.);
#1719=B_SPLINE_CURVE_WITH_KNOTS('',3,(#9794,#9795,#9796,#9797,#9798,#9799,
#9800,#9801,#9802,#9803,#9804,#9805,#9806,#9807,#9808,#9809,#9810,#9811,
#9812,#9813,#9814,#9815,#9816,#9817,#9818,#9819,#9820,#9821,#9822,#9823,
#9824,#9825,#9826,#9827,#9828,#9829,#9830,#9831),.UNSPECIFIED.,.F.,.F.,
(4,2,2,2,2,2,2,2,2,2,2,2,2,2,2,2,2,2,4),(65.4704662597666,65.495672175373,
65.8271134020289,66.152193527227,66.4701500123141,66.804300390124,67.1256555179792,
67.4509129283782,67.7808746179128,68.0985120833682,68.4297579283883,68.7555705314816,
69.0724663315543,69.4038489357916,69.7260301625157,70.0483887785603,70.3793203104939,
70.6978137297548,70.7257701778119),.UNSPECIFIED.);
#1720=B_SPLINE_CURVE_WITH_KNOTS('',3,(#9832,#9833,#9834,#9835,#9836,#9837,
#9838,#9839,#9840,#9841,#9842,#9843,#9844,#9845,#9846,#9847,#9848,#9849,
#9850,#9851,#9852,#9853,#9854,#9855,#9856,#9857,#9858,#9859,#9860,#9861,
#9862,#9863,#9864,#9865,#9866,#9867),.UNSPECIFIED.,.F.,.F.,(4,2,2,2,2,2,
2,2,2,2,2,2,2,2,2,2,2,4),(48.1589956367661,48.4040467523655,48.7308091602174,
49.0647361611568,49.3833609345423,49.7144356594085,50.0366521626909,50.3589642243882,
50.6903935164885,51.0072814592698,51.333226046925,51.6645265155671,51.9822893424162,
52.3123875254735,52.6374457953631,52.9589234957672,53.2816759952905,53.4142923811308),
 .UNSPECIFIED.);
#1721=B_SPLINE_CURVE_WITH_KNOTS('',3,(#9872,#9873,#9874,#9875,#9876,#9877,
#9878,#9879,#9880,#9881,#9882,#9883,#9884,#9885,#9886,#9887,#9888,#9889,
#9890,#9891,#9892,#9893,#9894,#9895,#9896,#9897,#9898,#9899,#9900,#9901,
#9902,#9903,#9904,#9905,#9906,#9907),.UNSPECIFIED.,.F.,.F.,(4,2,2,2,2,2,
2,2,2,2,2,2,2,2,2,2,2,4),(60.2150166643538,60.2919896896549,60.623468135119,
60.946546784158,61.2673685979683,61.5993003656792,61.9186940219388,62.2500158622836,
62.5776890328341,62.8941555378412,63.225569156602,63.5495824617272,63.8687296591539,
64.2017066441746,64.5220238831432,64.8500653079831,65.1788329505325,65.4704662597666),
 .UNSPECIFIED.);
#1722=B_SPLINE_CURVE_WITH_KNOTS('',3,(#9908,#9909,#9910,#9911,#9912,#9913,
#9914,#9915,#9916,#9917,#9918,#9919,#9920,#9921,#9922,#9923,#9924,#9925,
#9926,#9927,#9928,#9929,#9930,#9931,#9932,#9933,#9934,#9935,#9936,#9937,
#9938,#9939,#9940,#9941,#9942,#9943),.UNSPECIFIED.,.F.,.F.,(4,2,2,2,2,2,
2,2,2,2,2,2,2,2,2,2,2,4),(53.4142923811308,53.6035626727488,53.9351146179854,
54.2541797621075,54.5873610415979,54.9146187411077,55.2311787077779,55.5626980944589,
55.8863055375212,56.2063209314299,56.5388391129682,56.8587574511558,57.1884786504444,
57.5167651433843,57.8334302207767,58.1649297922668,58.4895427229089,58.6712567519585),
 .UNSPECIFIED.);
#1723=B_SPLINE_CURVE_WITH_KNOTS('',3,(#9948,#9949,#9950,#9951,#9952,#9953,
#9954,#9955,#9956,#9957,#9958,#9959,#9960,#9961,#9962,#9963,#9964,#9965,
#9966,#9967,#9968,#9969,#9970,#9971,#9972,#9973,#9974,#9975,#9976,#9977,
#9978,#9979,#9980,#9981,#9982,#9983),.UNSPECIFIED.,.F.,.F.,(4,2,2,2,2,2,
2,2,2,2,2,2,2,2,2,2,2,4),(54.958820463279,55.0853253597811,55.4191724857657,
55.7402468059445,56.0656389533752,56.3952984859766,56.7127551628249,57.0441447347562,
57.3700887293421,57.6872929598775,58.0189223071554,58.3412329272213,58.6640792208409,
58.9951320971355,59.3137505884142,59.6486547000943,59.9753747519229,60.2150166643538),
 .UNSPECIFIED.);
#1724=B_SPLINE_CURVE_WITH_KNOTS('',3,(#9984,#9985,#9986,#9987,#9988,#9989,
#9990,#9991,#9992,#9993,#9994,#9995,#9996,#9997,#9998,#9999,#10000,#10001,
#10002,#10003,#10004,#10005,#10006,#10007,#10008,#10009,#10010,#10011,#10012,
#10013,#10014,#10015,#10016,#10017,#10018,#10019),.UNSPECIFIED.,.F.,.F.,
(4,2,2,2,2,2,2,2,2,2,2,2,2,2,2,2,2,4),(58.6712567519585,58.8081120487695,
59.1417446836893,59.4626482699573,59.789314753556,60.1187508570411,60.4360562388358,
60.7676329075686,61.0933642112501,61.4110112022744,61.7458659425563,62.0678512720903,
62.3920318907359,62.7226968235716,63.0409778752441,63.3724839946026,63.6989739681192,
63.9299842069763),.UNSPECIFIED.);
#1725=B_SPLINE_CURVE_WITH_KNOTS('',3,(#10024,#10025,#10026,#10027,#10028,
#10029,#10030,#10031,#10032,#10033,#10034,#10035,#10036,#10037,#10038,#10039,
#10040,#10041,#10042,#10043,#10044,#10045,#10046,#10047,#10048,#10049,#10050,
#10051,#10052,#10053,#10054,#10055,#10056,#10057,#10058,#10059),
 .UNSPECIFIED.,.F.,.F.,(4,2,2,2,2,2,2,2,2,2,2,2,2,2,2,2,2,4),(49.7053427805776,
49.8946649833997,50.2193889038838,50.5506783072757,50.8672681505552,51.1956719499015,
51.5241929101829,51.8441827696492,52.176801691369,52.4961122101446,52.8197929106681,
53.1510737257235,53.4673975704681,53.7947321500115,54.1113468652774,54.4426191551792,
54.7674124920873,54.958820463279),.UNSPECIFIED.);
#1726=B_SPLINE_CURVE_WITH_KNOTS('',3,(#10060,#10061,#10062,#10063,#10064,
#10065,#10066,#10067,#10068,#10069,#10070,#10071,#10072,#10073,#10074,#10075,
#10076,#10077,#10078,#10079,#10080,#10081,#10082,#10083,#10084,#10085,#10086,
#10087,#10088,#10089,#10090,#10091,#10092,#10093,#10094,#10095),
 .UNSPECIFIED.,.F.,.F.,(4,2,2,2,2,2,2,2,2,2,2,2,2,2,2,2,2,4),(63.9299842069763,
64.0158273939492,64.3474243448431,64.6702762228065,64.9918697143397,65.3235363775539,
65.6427018726441,65.9753696656186,66.3027524871346,66.6192856711435,66.9507860810698,
67.2745160647127,67.5942889179192,67.926944884661,68.2469841445378,68.576236629585,
68.9046677223753,69.1866887443586),.UNSPECIFIED.);
#1727=B_SPLINE_CURVE_WITH_KNOTS('',3,(#10100,#10101,#10102,#10103,#10104,
#10105,#10106,#10107,#10108,#10109,#10110,#10111,#10112,#10113,#10114,#10115,
#10116,#10117,#10118,#10119,#10120,#10121,#10122,#10123,#10124,#10125,#10126,
#10127,#10128,#10129,#10130,#10131,#10132,#10133,#10134,#10135),
 .UNSPECIFIED.,.F.,.F.,(4,2,2,2,2,2,2,2,2,2,2,2,2,2,2,2,2,4),(44.4491313433541,
44.6870015935932,45.0136378977987,45.3450417551313,45.6634567886658,45.9942822750444,
46.3176176911724,46.639728628672,46.9747441773675,47.2920071882406,47.61787524196,
47.949273189522,48.2666625046887,48.5962434167468,48.921870506651,49.2428780108371,
49.5766476892823,49.7053427805776),.UNSPECIFIED.);
#1728=B_SPLINE_CURVE_WITH_KNOTS('',3,(#10136,#10137,#10138,#10139,#10140,
#10141,#10142,#10143,#10144,#10145,#10146,#10147,#10148,#10149,#10150,#10151,
#10152,#10153,#10154,#10155,#10156,#10157,#10158,#10159,#10160,#10161,#10162,
#10163,#10164,#10165,#10166,#10167,#10168,#10169,#10170,#10171,#10172,#10173),
 .UNSPECIFIED.,.F.,.F.,(4,2,2,2,2,2,2,2,2,2,2,2,2,2,2,2,2,2,4),(69.1866887443586,
69.2213801122111,69.5528737530356,69.8776274198326,70.1960238834839,70.5298118984127,
70.8508520952963,71.1771217050446,71.5067159395957,71.8241430246874,72.1557282115081,
72.4816129287093,72.7991644584063,73.1341863748964,73.4563190370224,73.7801912419322,
74.1110223351671,74.429453819747,74.4454842874606),.UNSPECIFIED.);
#1729=B_SPLINE_CURVE_WITH_KNOTS('',3,(#10178,#10179,#10180,#10181,#10182,
#10183,#10184,#10185,#10186,#10187,#10188,#10189,#10190,#10191,#10192,#10193,
#10194,#10195,#10196,#10197,#10198,#10199,#10200,#10201,#10202,#10203,#10204,
#10205,#10206,#10207,#10208,#10209,#10210,#10211,#10212,#10213),
 .UNSPECIFIED.,.F.,.F.,(4,2,2,2,2,2,2,2,2,2,2,2,2,2,2,2,2,4),(39.1940267703943,
39.4837106853752,39.8123739358409,40.140615639691,40.4608409439614,40.7937158675648,
41.112947714973,41.4368674212289,41.768260888568,42.0847004092134,42.4122780772443,
42.7438288668753,43.0631402657561,43.3949808385494,43.7159177151437,44.0389137877124,
44.3703784563307,44.4491313433541),.UNSPECIFIED.);
#1730=B_SPLINE_CURVE_WITH_KNOTS('',3,(#10214,#10215,#10216,#10217,#10218,
#10219,#10220,#10221,#10222,#10223,#10224,#10225,#10226,#10227,#10228,#10229,
#10230,#10231,#10232,#10233,#10234,#10235,#10236,#10237,#10238,#10239,#10240,
#10241,#10242,#10243,#10244,#10245,#10246,#10247,#10248,#10249),
 .UNSPECIFIED.,.F.,.F.,(4,2,2,2,2,2,2,2,2,2,2,2,2,2,2,2,2,4),(74.4454842874606,
74.7610038707573,75.0876524143285,75.4044823371837,75.7361094557603,76.059117988834,
76.3804901299688,76.7123298778693,77.0316519837141,77.3638858973244,77.6914506845162,
78.0080234552417,78.3395658510996,78.6634744683095,78.98307823724,79.3159291149286,
79.636144436891,79.7030451201867),.UNSPECIFIED.);
#1731=B_SPLINE_CURVE_WITH_KNOTS('',3,(#10254,#10255,#10256,#10257,#10258,
#10259,#10260,#10261,#10262,#10263,#10264,#10265,#10266,#10267,#10268,#10269,
#10270,#10271,#10272,#10273,#10274,#10275,#10276,#10277,#10278,#10279,#10280,
#10281,#10282,#10283,#10284,#10285,#10286,#10287,#10288,#10289,#10290,#10291),
 .UNSPECIFIED.,.F.,.F.,(4,2,2,2,2,2,2,2,2,2,2,2,2,2,2,2,2,2,4),(33.9358727252235,
33.9621245083147,34.2809288568771,34.6121781063724,34.9350748526361,35.2575723609102,
35.5893508296672,35.9066695684309,36.2328023369551,36.5643384731628,36.881976653502,
37.2118280837638,37.5372450060053,37.8585010955848,38.1925414770318,38.510544921809,
38.8355231435545,39.1669372659656,39.1940267703943),.UNSPECIFIED.);
#1732=B_SPLINE_CURVE_WITH_KNOTS('',3,(#10292,#10293,#10294,#10295,#10296,
#10297,#10298,#10299,#10300,#10301,#10302,#10303,#10304,#10305,#10306,#10307,
#10308,#10309,#10310,#10311,#10312,#10313,#10314,#10315,#10316,#10317,#10318,
#10319,#10320,#10321,#10322,#10323,#10324,#10325,#10326,#10327),
 .UNSPECIFIED.,.F.,.F.,(4,2,2,2,2,2,2,2,2,2,2,2,2,2,2,2,2,4),(79.7030451201867,
79.9650097989887,80.2936411166196,80.6104655377856,80.9420139501394,81.2669633105644,
81.5852589459215,81.9192583194259,82.2404892582695,82.5664436673889,82.896250644087,
83.2138610400208,83.5455152139737,83.8716073734113,84.189133085679,84.5243772521638,
84.8467106050261,84.9624042671722),.UNSPECIFIED.);
#1733=B_SPLINE_CURVE_WITH_KNOTS('',3,(#10332,#10333,#10334,#10335,#10336,
#10337,#10338,#10339,#10340,#10341,#10342,#10343,#10344,#10345,#10346,#10347,
#10348,#10349,#10350,#10351,#10352,#10353,#10354,#10355,#10356,#10357,#10358,
#10359,#10360,#10361,#10362,#10363,#10364,#10365,#10366,#10367),
 .UNSPECIFIED.,.F.,.F.,(4,2,2,2,2,2,2,2,2,2,2,2,2,2,2,2,2,4),(28.6778433505252,
28.751513892831,29.0720320491282,29.4052222858157,29.7244522500093,30.0486692456809,
30.3802402592666,30.6968635486887,31.0247433023543,31.356055628844,31.6756433970708,
32.0077807707016,32.3286652307542,32.6519398567504,32.9835714209526,33.3003193076007,
33.6272377323579,33.9358727252235),.UNSPECIFIED.);
#1734=B_SPLINE_CURVE_WITH_KNOTS('',3,(#10368,#10369,#10370,#10371,#10372,
#10373,#10374,#10375,#10376,#10377,#10378,#10379,#10380,#10381,#10382,#10383,
#10384,#10385,#10386,#10387,#10388,#10389,#10390,#10391,#10392,#10393,#10394,
#10395,#10396,#10397,#10398,#10399,#10400,#10401,#10402,#10403),
 .UNSPECIFIED.,.F.,.F.,(4,2,2,2,2,2,2,2,2,2,2,2,2,2,2,2,2,4),(84.9624042671722,
85.1703540448489,85.5014052173264,85.8200393157319,86.1516925680166,86.4785528419088,
86.7954247866363,87.1271416154083,87.4503592344816,87.7715856592211,88.1036516073096,
88.4231817863373,88.7550702706801,89.0828684670286,89.3995444073536,89.7311877492214,
90.0553258055558,90.2220141793614),.UNSPECIFIED.);
#1735=B_SPLINE_CURVE_WITH_KNOTS('',3,(#10408,#10409,#10410,#10411,#10412,
#10413,#10414,#10415,#10416,#10417,#10418,#10419,#10420,#10421,#10422,#10423,
#10424,#10425,#10426,#10427,#10428,#10429,#10430,#10431,#10432,#10433,#10434,
#10435,#10436,#10437,#10438,#10439,#10440,#10441,#10442,#10443),
 .UNSPECIFIED.,.F.,.F.,(4,2,2,2,2,2,2,2,2,2,2,2,2,2,2,2,2,4),(23.4194570300931,
23.5448375458363,23.8672296315852,24.1987821581931,24.5158120140399,24.8418376691952,
25.1732575822623,25.4911009723972,25.8212799176309,26.1465728220054,26.468133988391,
26.8025033396155,27.1205676123453,27.4458573583117,27.777460695228,28.0944829929136,
28.423463545569,28.6778433505252),.UNSPECIFIED.);
#1736=B_SPLINE_CURVE_WITH_KNOTS('',3,(#10444,#10445,#10446,#10447,#10448,
#10449,#10450,#10451,#10452,#10453,#10454,#10455,#10456,#10457,#10458,#10459,
#10460,#10461,#10462,#10463,#10464,#10465,#10466,#10467,#10468,#10469,#10470,
#10471,#10472,#10473,#10474,#10475,#10476,#10477,#10478,#10479),
 .UNSPECIFIED.,.F.,.F.,(4,2,2,2,2,2,2,2,2,2,2,2,2,2,2,2,2,4),(90.2220141793614,
90.3748353736429,90.7079326119538,91.0283739647954,91.3569409816704,91.6858224287003,
92.0028189133833,92.3344804973216,92.6596749253133,92.9779419941321,93.3122027564306,
93.633673155364,93.959399049641,94.2894674880067,94.6073164436775,94.9390974276225,
95.2654453128683,95.4826145482641),.UNSPECIFIED.);
#1737=B_SPLINE_CURVE_WITH_KNOTS('',3,(#10484,#10485,#10486,#10487,#10488,
#10489,#10490,#10491,#10492,#10493,#10494,#10495,#10496,#10497,#10498,#10499,
#10500,#10501,#10502,#10503,#10504,#10505,#10506,#10507,#10508,#10509,#10510,
#10511,#10512,#10513,#10514,#10515,#10516,#10517,#10518,#10519),
 .UNSPECIFIED.,.F.,.F.,(4,2,2,2,2,2,2,2,2,2,2,2,2,2,2,2,2,4),(18.1643899839031,
18.3379240397195,18.6620768943873,18.9934447562906,19.3098966760481,19.6377132453628,
19.9683761687022,20.2878829729932,20.6199467688078,20.9403963553448,21.2635882727924,
21.5950049811214,21.9115161728676,22.2383515620108,22.5725584681035,22.8912614297431,
23.2224142667495,23.4194570300931),.UNSPECIFIED.);
#1738=B_SPLINE_CURVE_WITH_KNOTS('',3,(#10520,#10521,#10522,#10523,#10524,
#10525,#10526,#10527,#10528,#10529,#10530,#10531,#10532,#10533,#10534,#10535,
#10536,#10537,#10538,#10539,#10540,#10541,#10542,#10543,#10544,#10545,#10546,
#10547,#10548,#10549,#10550,#10551,#10552,#10553,#10554,#10555),
 .UNSPECIFIED.,.F.,.F.,(4,2,2,2,2,2,2,2,2,2,2,2,2,2,2,2,2,4),(95.4826145482641,
95.5830131784909,95.9150352583438,96.2377453618514,96.5609337305379,96.8923988013166,
97.2114126750681,97.5466420806929,97.873770877236,98.1907566599105,98.5226293845204,
98.8461121465705,99.1672791546219,99.4996279190605,99.8194212411041,100.151068073815,
100.47915443311,100.745055882445),.UNSPECIFIED.);
#1739=B_SPLINE_CURVE_WITH_KNOTS('',3,(#10560,#10561,#10562,#10563,#10564,
#10565,#10566,#10567,#10568,#10569,#10570,#10571,#10572,#10573,#10574,#10575,
#10576,#10577,#10578,#10579,#10580,#10581,#10582,#10583,#10584,#10585,#10586,
#10587,#10588,#10589,#10590,#10591,#10592,#10593,#10594,#10595),
 .UNSPECIFIED.,.F.,.F.,(4,2,2,2,2,2,2,2,2,2,2,2,2,2,2,2,2,4),(12.9085896449044,
13.1319654813851,13.4579477094742,13.7892099133384,14.1070063349617,14.4371455212647,
14.7619252560797,15.0834330090954,15.4177596038885,15.7355181257431,16.0607572042731,
16.3921701425435,16.7090911171914,17.0380229391824,17.3654819678967,17.6859353124529,
18.0190701048524,18.1643899839031),.UNSPECIFIED.);
#1740=B_SPLINE_CURVE_WITH_KNOTS('',3,(#10596,#10597,#10598,#10599,#10600,
#10601,#10602,#10603,#10604,#10605,#10606,#10607,#10608,#10609,#10610,#10611,
#10612,#10613,#10614,#10615,#10616,#10617,#10618,#10619,#10620,#10621,#10622,
#10623,#10624,#10625,#10626,#10627,#10628,#10629,#10630,#10631,#10632,#10633),
 .UNSPECIFIED.,.F.,.F.,(4,2,2,2,2,2,2,2,2,2,2,2,2,2,2,2,2,2,4),(100.745055882445,
100.796001734715,101.127811382384,101.452233014914,101.771732249291,102.105130527508,
102.425851249821,102.754222181351,103.083406799012,103.400638353147,103.732477635844,
104.057969677998,104.37628762465,104.710862903123,105.032624730452,105.358220131125,
105.688601838775,106.006642269571,106.007580002483),.UNSPECIFIED.);
#1741=B_SPLINE_CURVE_WITH_KNOTS('',3,(#10638,#10639,#10640,#10641,#10642,
#10643,#10644,#10645,#10646,#10647,#10648,#10649,#10650,#10651,#10652,#10653,
#10654,#10655,#10656,#10657,#10658,#10659,#10660,#10661,#10662,#10663,#10664,
#10665,#10666,#10667,#10668,#10669,#10670,#10671,#10672,#10673),
 .UNSPECIFIED.,.F.,.F.,(4,2,2,2,2,2,2,2,2,2,2,2,2,2,2,2,2,4),(7.65580643120489,
7.92903377067465,8.25685231429426,8.586904928944,8.90639349536678,9.23844967293158,
9.55851322774851,9.88168615770634,10.2129451312994,10.5292795485054,10.8560965326263,
11.1896576540031,11.508321254098,11.8394428317127,12.1614368336248,12.4837863523509,
12.8151694339259,12.9085896449044),.UNSPECIFIED.);
#1742=B_SPLINE_CURVE_WITH_KNOTS('',3,(#10674,#10675,#10676,#10677,#10678,
#10679,#10680,#10681,#10682,#10683,#10684,#10685,#10686,#10687,#10688,#10689,
#10690,#10691,#10692,#10693,#10694,#10695,#10696,#10697,#10698,#10699,#10700,
#10701,#10702,#10703,#10704,#10705,#10706,#10707,#10708,#10709),
 .UNSPECIFIED.,.F.,.F.,(4,2,2,2,2,2,2,2,2,2,2,2,2,2,2,2,2,4),(106.007580002483,
106.338291050777,106.664517770686,106.981785151794,107.313569075925,107.63615988381,
107.958865999156,108.290220246233,108.609119030096,108.943662487344,109.270693914527,
109.587430237008,109.919075729356,110.242461649198,110.563183930418,110.895444456502,
111.215142893136,111.266831993831),.UNSPECIFIED.);
#1743=B_SPLINE_CURVE_WITH_KNOTS('',3,(#10715,#10716,#10717,#10718,#10719,
#10720,#10721,#10722,#10723,#10724,#10725,#10726),.UNSPECIFIED.,.F.,.F.,
(4,2,2,2,2,4),(116.52588314767,116.750177738512,117.080505043093,117.398484542365,
117.660053024643,117.93068616261),.UNSPECIFIED.);
#1744=B_SPLINE_CURVE_WITH_KNOTS('',3,(#10729,#10730,#10731,#10732,#10733,
#10734,#10735,#10736,#10737,#10738,#10739,#10740,#10741,#10742,#10743,#10744,
#10745,#10746),.UNSPECIFIED.,.F.,.F.,(4,2,2,2,2,2,2,2,4),(1.00000002753453E-6,
0.230913164999998,0.461176488336289,0.782795083268026,1.10516503507019,
1.43643805917748,1.75306071300765,2.07906337640022,2.40199466308743),
 .UNSPECIFIED.);
#1745=B_SPLINE_CURVE_WITH_KNOTS('',3,(#10781,#10782,#10783,#10784,#10785,
#10786,#10787,#10788,#10789,#10790,#10791,#10792,#10793,#10794,#10795,#10796,
#10797,#10798,#10799,#10800,#10801,#10802,#10803,#10804,#10805,#10806,#10807,
#10808,#10809,#10810,#10811,#10812,#10813,#10814,#10815,#10816,#10817,#10818,
#10819,#10820,#10821,#10822,#10823,#10824,#10825,#10826,#10827,#10828,#10829,
#10830,#10831,#10832,#10833,#10834,#10835),.UNSPECIFIED.,.F.,.F.,(4,3,3,
3,3,3,3,3,3,3,3,3,3,3,3,3,3,3,4),(1.5707963267949,1.64242105278282,1.71479015258711,
1.78837553839344,1.86258767446152,1.93745389192044,1.96813996588655,2.04189099921108,
2.1192539697587,2.19381715259638,2.26806604838722,2.34147638917228,2.35134288140155,
2.42596150493344,2.50323613885248,2.57624208460566,2.64856017426106,2.72000077351568,
2.73506004060959),.UNSPECIFIED.);
#1746=B_SPLINE_CURVE_WITH_KNOTS('',3,(#10854,#10855,#10856,#10857,#10858,
#10859,#10860,#10861,#10862,#10863,#10864,#10865,#10866,#10867,#10868,#10869,
#10870,#10871,#10872,#10873,#10874,#10875,#10876,#10877,#10878,#10879,#10880,
#10881,#10882,#10883,#10884,#10885,#10886,#10887,#10888,#10889,#10890,#10891,
#10892,#10893,#10894,#10895,#10896,#10897,#10898,#10899,#10900,#10901,#10902,
#10903,#10904,#10905,#10906,#10907,#10908),.UNSPECIFIED.,.F.,.F.,(4,3,3,
3,3,3,3,3,3,3,3,3,3,3,3,3,3,3,4),(1.5707963267949,1.64242105278141,1.71479015258438,
1.78837553839004,1.86258767445774,1.93745389191671,1.96813996588634,2.04189099921108,
2.11925396975866,2.19381715259688,2.26806604838803,2.34147638917343,2.35134288140141,
2.42596150493384,2.50323613885278,2.57624208460631,2.64856017426199,2.72000077351667,
2.73506004060958),.UNSPECIFIED.);
#1747=B_SPLINE_CURVE_WITH_KNOTS('',3,(#10922,#10923,#10924,#10925,#10926,
#10927,#10928,#10929,#10930,#10931,#10932,#10933,#10934,#10935,#10936,#10937,
#10938,#10939,#10940,#10941,#10942,#10943,#10944,#10945,#10946,#10947,#10948,
#10949,#10950,#10951,#10952,#10953,#10954,#10955,#10956,#10957,#10958,#10959,
#10960,#10961,#10962,#10963,#10964,#10965,#10966,#10967),.UNSPECIFIED.,
 .F.,.F.,(4,3,3,3,3,3,3,3,3,3,3,3,3,3,3,4),(0.,0.000102625409859305,0.000209255998910644,
0.000322661982762533,0.000440290006433478,0.000564825588011048,0.000629111603363879,
0.00077150452647986,0.0008514190604454,0.0009068473692292,0.000932968415359167,
0.00114800502221307,0.00137019159493578,0.00141082079820418,0.00163330152526633,
0.00183019574357075),.UNSPECIFIED.);
#1748=B_SPLINE_CURVE_WITH_KNOTS('',3,(#10969,#10970,#10971,#10972,#10973,
#10974,#10975,#10976,#10977,#10978,#10979,#10980,#10981,#10982,#10983,#10984,
#10985,#10986,#10987,#10988,#10989,#10990,#10991,#10992,#10993,#10994,#10995,
#10996,#10997,#10998,#10999,#11000,#11001,#11002,#11003,#11004,#11005,#11006,
#11007,#11008,#11009,#11010,#11011,#11012,#11013,#11014,#11015,#11016,#11017,
#11018,#11019,#11020),.UNSPECIFIED.,.F.,.F.,(4,3,3,3,3,3,3,3,3,3,3,3,3,
3,3,3,3,4),(0.00183019700058168,0.0021246721247389,0.00232004474458504,
0.00265469094004782,0.0030060000015604,0.00333449619907014,0.00369804959273491,
0.00408054678755802,0.00447405832991094,0.00488126280004193,0.00494084368376952,
0.00544455820475954,0.00560720862373659,0.00609214785612222,0.00662068586019803,
0.00717627308542189,0.00775568315893149,0.00805149036695734),
 .UNSPECIFIED.);
#1749=B_SPLINE_CURVE_WITH_KNOTS('',3,(#11024,#11025,#11026,#11027,#11028,
#11029,#11030,#11031,#11032,#11033,#11034,#11035,#11036,#11037,#11038,#11039,
#11040,#11041,#11042,#11043,#11044,#11045,#11046,#11047,#11048,#11049,#11050,
#11051,#11052,#11053,#11054,#11055,#11056,#11057,#11058,#11059,#11060,#11061,
#11062,#11063,#11064,#11065,#11066,#11067,#11068,#11069,#11070,#11071,#11072,
#11073,#11074,#11075,#11076,#11077,#11078,#11079,#11080,#11081,#11082,#11083,
#11084,#11085,#11086,#11087,#11088,#11089,#11090,#11091,#11092,#11093,#11094,
#11095,#11096,#11097,#11098,#11099,#11100,#11101,#11102,#11103,#11104,#11105,
#11106,#11107,#11108,#11109,#11110,#11111,#11112,#11113,#11114),
 .UNSPECIFIED.,.F.,.F.,(4,3,3,3,3,3,3,3,3,3,3,3,3,3,3,3,3,3,3,3,3,3,3,3,
3,3,3,3,3,3,4),(-2.02092030439988E-5,0.000556049295526959,0.0011217165797188,
0.00167096865970714,0.00219205980753922,0.00242674993854338,0.00286892709473989,
0.00328265444055326,0.00359051333580498,0.00399833809851151,0.00437342345628195,
0.00468974844460364,0.00504885723392668,0.00539155487814984,0.0057022315709967,
0.00596953869846673,0.00600761174928926,0.00621566605302231,0.00641489721149064,
0.00660361036059914,0.00661412836995897,0.00681882170159619,0.00701224857467813,
0.00717494882539777,0.007333188837526,0.00739068892409821,0.0075472380430904,
0.00769433317592032,0.00783806436270165,0.00797708941084355,0.008016885400067),
 .UNSPECIFIED.);
#1750=B_SPLINE_CURVE_WITH_KNOTS('',3,(#11116,#11117,#11118,#11119,#11120,
#11121,#11122),.UNSPECIFIED.,.F.,.F.,(4,3,4),(0.,0.000319771717876966,0.000495697630009108),
 .UNSPECIFIED.);
#1751=B_SPLINE_CURVE_WITH_KNOTS('',3,(#11125,#11126,#11127,#11128,#11129,
#11130,#11131),.UNSPECIFIED.,.F.,.F.,(4,3,4),(0.,0.000319771718042548,0.000495697630009101),
 .UNSPECIFIED.);
#1752=B_SPLINE_CURVE_WITH_KNOTS('',3,(#11137,#11138,#11139,#11140,#11141,
#11142,#11143,#11144,#11145,#11146,#11147,#11148,#11149,#11150,#11151,#11152,
#11153,#11154,#11155,#11156,#11157,#11158,#11159,#11160,#11161,#11162,#11163,
#11164,#11165,#11166,#11167,#11168,#11169,#11170,#11171,#11172,#11173,#11174,
#11175,#11176),.UNSPECIFIED.,.F.,.F.,(4,3,3,3,3,3,3,3,3,3,3,3,3,4),(4.33680868994202E-19,
0.000224425374774483,0.000451595406483904,0.000691860819919334,0.000897701499097931,
0.000980242722923433,0.00133024746973674,0.00170122585014586,0.00187037776501358,
0.00196048544584687,0.00235337437521485,0.00279968089622725,0.00329820841760096,
0.00392097089169373),.UNSPECIFIED.);
#1753=B_SPLINE_CURVE_WITH_KNOTS('',3,(#11181,#11182,#11183,#11184,#11185,
#11186,#11187,#11188,#11189,#11190,#11191,#11192,#11193,#11194,#11195,#11196,
#11197,#11198,#11199,#11200,#11201,#11202,#11203,#11204,#11205,#11206,#11207,
#11208,#11209,#11210,#11211,#11212,#11213,#11214,#11215,#11216,#11217,#11218,
#11219,#11220,#11221,#11222,#11223),.UNSPECIFIED.,.F.,.F.,(4,3,3,3,3,3,
3,3,3,3,3,3,3,3,4),(-1.52431972735595E-5,0.000577208203721174,0.00105830978507474,
0.00150240305417916,0.00189185074719465,0.00194649632328358,0.00203665697126435,
0.00241070485831859,0.0027626461229275,0.00292736608356214,0.00300995787129902,
0.00325030870484351,0.00348216857793155,0.00370167549193661,0.00390823584384071),
 .UNSPECIFIED.);
#1754=B_SPLINE_CURVE_WITH_KNOTS('',3,(#11229,#11230,#11231,#11232,#11233,
#11234,#11235,#11236,#11237,#11238,#11239,#11240,#11241,#11242,#11243,#11244,
#11245,#11246,#11247,#11248,#11249,#11250,#11251,#11252,#11253,#11254,#11255,
#11256,#11257,#11258,#11259,#11260,#11261,#11262,#11263,#11264,#11265,#11266,
#11267,#11268),.UNSPECIFIED.,.F.,.F.,(4,3,3,3,3,3,3,3,3,3,3,3,3,4),(0.,
0.000224425374774487,0.000451595406490086,0.000691860819931689,0.000897701499097949,
0.000980242722923432,0.00133024746979985,0.0017012258502438,0.00187037776501362,
0.00196048544584686,0.00235337437512353,0.00279968089602665,0.00329820841722131,
0.00392097089169373),.UNSPECIFIED.);
#1755=B_SPLINE_CURVE_WITH_KNOTS('',3,(#11271,#11272,#11273,#11274,#11275,
#11276,#11277,#11278,#11279,#11280,#11281,#11282,#11283,#11284,#11285,#11286,
#11287,#11288,#11289,#11290,#11291,#11292,#11293,#11294,#11295,#11296,#11297,
#11298,#11299,#11300,#11301,#11302,#11303,#11304,#11305,#11306,#11307,#11308,
#11309,#11310,#11311,#11312,#11313),.UNSPECIFIED.,.F.,.F.,(4,3,3,3,3,3,
3,3,3,3,3,3,3,3,4),(-1.52431972735601E-5,0.000577208204035659,0.00105830978563783,
0.0015024030544607,0.0018918507477027,0.00194649632328357,0.00203665697126436,
0.00241070485830986,0.00276264612288319,0.00292736608356214,0.00300995787129895,
0.00325030870484637,0.00348216857793754,0.00370167549194714,0.0039082358438407),
 .UNSPECIFIED.);
#1756=B_SPLINE_CURVE_WITH_KNOTS('',3,(#11315,#11316,#11317,#11318,#11319,
#11320,#11321,#11322,#11323,#11324,#11325,#11326,#11327,#11328,#11329,#11330,
#11331,#11332,#11333,#11334,#11335,#11336,#11337,#11338,#11339,#11340,#11341,
#11342,#11343,#11344,#11345,#11346,#11347,#11348,#11349,#11350,#11351,#11352),
 .UNSPECIFIED.,.F.,.F.,(4,2,2,2,2,2,2,2,2,2,2,2,2,2,2,2,2,2,4),(2.40199466308743,
2.41022829061081,2.72804014342947,3.05820492223309,3.38252194159165,3.70403954337583,
4.03838990610341,4.3559009458349,4.68115375921356,5.01243500977675,5.32932288323347,
5.65827132582605,5.98518396240259,6.30563559995583,6.63878133247469,6.95731312617532,
7.28146604930193,7.6126886063725,7.65580643120489),.UNSPECIFIED.);
#1757=B_SPLINE_CURVE_WITH_KNOTS('',3,(#11353,#11354,#11355,#11356,#11357,
#11358,#11359,#11360,#11361,#11362,#11363,#11364,#11365,#11366,#11367,#11368,
#11369,#11370,#11371,#11372,#11373,#11374,#11375,#11376,#11377,#11378,#11379,
#11380,#11381,#11382,#11383,#11384,#11385,#11386,#11387,#11388),
 .UNSPECIFIED.,.F.,.F.,(4,2,2,2,2,2,2,2,2,2,2,2,2,2,2,2,2,4),(111.266831993831,
111.546133142784,111.874141801841,112.19080377709,112.52239771137,112.846740900166,
113.165853021345,113.499181039949,113.819822891596,114.147593945405,114.476715222664,
114.793830501138,115.125466606025,115.450893587892,115.768893554885,116.103411184789,
116.425105464923,116.52588314767),.UNSPECIFIED.);
#1758=B_SPLINE_CURVE_WITH_KNOTS('',3,(#11527,#11528,#11529,#11530,#11531,
#11532,#11533,#11534,#11535,#11536,#11537,#11538,#11539,#11540),
 .UNSPECIFIED.,.F.,.F.,(4,2,2,2,2,2,4),(-1.10452810243334,-0.974933410506299,
-0.837207473665695,-0.613047163496973,-0.39375324246162,-0.222767201532269,
-1.00000002589695E-6),.UNSPECIFIED.);
#1759=B_SPLINE_CURVE_WITH_KNOTS('',3,(#11542,#11543,#11544,#11545,#11546,
#11547,#11548,#11549,#11550,#11551,#11552,#11553,#11554,#11555),
 .UNSPECIFIED.,.F.,.F.,(4,2,2,2,2,2,4),(-1.30358759250105,-1.10825126792048,
-0.956598415540384,-0.727542338165497,-0.426865540585114,-0.212508103920413,
-1.35447209004269E-14),.UNSPECIFIED.);
#1760=B_SPLINE_CURVE_WITH_KNOTS('',3,(#11559,#11560,#11561,#11562,#11563,
#11564,#11565,#11566,#11567,#11568,#11569,#11570,#11571,#11572,#11573,#11574,
#11575,#11576),.UNSPECIFIED.,.F.,.F.,(4,2,2,2,2,2,2,2,4),(9.99983121677346E-7,
0.000271322710449146,0.000517114380161633,0.000867591142278511,0.00130908967571248,
0.00208383766110333,0.00540070491534943,0.0164991372137869,0.0397725131276181),
 .UNSPECIFIED.);
#1761=B_SPLINE_CURVE_WITH_KNOTS('',3,(#11577,#11578,#11579,#11580,#11581,
#11582),.UNSPECIFIED.,.F.,.F.,(4,2,4),(0.,0.271067367187735,0.499520314311641),
 .UNSPECIFIED.);
#1762=B_SPLINE_CURVE_WITH_KNOTS('',3,(#11584,#11585,#11586,#11587,#11588,
#11589,#11590,#11591,#11592,#11593,#11594,#11595,#11596,#11597,#11598,#11599),
 .UNSPECIFIED.,.F.,.F.,(4,2,2,2,2,2,2,4),(1.00000001479692E-6,0.262243555324206,
0.507346056711276,0.828287498988696,0.998760751432299,1.30961651062506,
1.47837958130377,1.65229555251206),.UNSPECIFIED.);
#1763=B_SPLINE_CURVE_WITH_KNOTS('',3,(#11600,#11601,#11602,#11603,#11604,
#11605),.UNSPECIFIED.,.F.,.F.,(4,2,4),(0.,0.172721058240164,0.344957068700543),
 .UNSPECIFIED.);
#1764=B_SPLINE_CURVE_WITH_KNOTS('',3,(#11802,#11803,#11804,#11805,#11806,
#11807,#11808,#11809,#11810,#11811,#11812,#11813,#11814,#11815,#11816,#11817,
#11818,#11819,#11820,#11821,#11822,#11823,#11824,#11825,#11826,#11827,#11828,
#11829,#11830,#11831,#11832,#11833,#11834,#11835,#11836,#11837,#11838,#11839,
#11840,#11841),.UNSPECIFIED.,.F.,.F.,(4,3,3,3,3,3,3,3,3,3,3,3,3,4),(-1.31423244832839E-5,
0.000535751919476727,0.00105440309977669,0.00152703982999462,0.00193278669513403,
0.00195362085609606,0.00231730204515171,0.00265300264582922,0.00290575120494268,
0.00292287708750121,0.00323755006403241,0.00353412708051367,0.00381242976596417,
0.00387871571475133),.UNSPECIFIED.);
#1765=B_SPLINE_CURVE_WITH_KNOTS('',3,(#11843,#11844,#11845,#11846,#11847,
#11848,#11849,#11850,#11851,#11852,#11853,#11854,#11855,#11856,#11857,#11858,
#11859,#11860,#11861,#11862,#11863,#11864,#11865,#11866,#11867,#11868,#11869,
#11870,#11871,#11872,#11873,#11874,#11875,#11876,#11877,#11878,#11879,#11880,
#11881,#11882,#11883,#11884,#11885,#11886,#11887,#11888,#11889,#11890,#11891,
#11892,#11893,#11894,#11895,#11896,#11897,#11898,#11899,#11900,#11901,#11902,
#11903,#11904,#11905,#11906,#11907,#11908,#11909,#11910,#11911,#11912,#11913,
#11914,#11915,#11916,#11917,#11918,#11919,#11920,#11921),.UNSPECIFIED.,
 .F.,.F.,(4,3,3,3,3,3,3,3,3,3,3,3,3,3,3,3,3,3,3,3,3,3,3,3,3,3,4),(8.67361737988404E-19,
0.000202743010865249,0.000410514286400591,0.000626630076752085,0.000743751984502465,
0.000896895697750054,0.00116850905342267,0.00144756822847459,0.00154043258165819,
0.00179379139550011,0.00205677592735176,0.00233242599985497,0.00239862131095936,
0.00272711606086079,0.00307220744579522,0.003305634398149,0.00358758279100021,
0.00401837140737556,0.00424614693708929,0.00468203334964349,0.00515625220928118,
0.00521101431097261,0.00538137418650031,0.0060186616833771,0.00627826988425036,
0.00676573329680739,0.00717516558200042),.UNSPECIFIED.);
#1766=B_SPLINE_CURVE_WITH_KNOTS('',3,(#11925,#11926,#11927,#11928,#11929,
#11930,#11931,#11932,#11933,#11934,#11935,#11936,#11937,#11938,#11939,#11940,
#11941,#11942,#11943,#11944,#11945,#11946,#11947,#11948,#11949,#11950,#11951,
#11952,#11953,#11954,#11955,#11956,#11957,#11958,#11959,#11960,#11961,#11962,
#11963,#11964),.UNSPECIFIED.,.F.,.F.,(4,3,3,3,3,3,3,3,3,3,3,3,3,4),(4.33680868994202E-19,
0.000280621540973947,0.000573887525893564,0.000891635349190541,0.000951755207402115,
0.000968821950376569,0.00129993329989977,0.00165663590864014,0.00191687066807321,
0.00193764390075314,0.00253097521482023,0.00313046488108132,0.00374040674088882,
0.00387528780150628),.UNSPECIFIED.);
#1767=B_SPLINE_CURVE_WITH_KNOTS('',3,(#11965,#11966,#11967,#11968,#11969,
#11970,#11971,#11972,#11973,#11974,#11975,#11976,#11977,#11978,#11979,#11980,
#11981,#11982,#11983,#11984,#11985,#11986,#11987,#11988,#11989,#11990,#11991,
#11992,#11993,#11994,#11995,#11996,#11997,#11998,#11999,#12000,#12001,#12002,
#12003,#12004,#12005,#12006,#12007,#12008,#12009,#12010,#12011,#12012,#12013,
#12014,#12015,#12016,#12017,#12018,#12019,#12020,#12021,#12022,#12023,#12024,
#12025,#12026,#12027,#12028,#12029,#12030,#12031,#12032,#12033,#12034,#12035,
#12036,#12037,#12038,#12039,#12040),.UNSPECIFIED.,.F.,.F.,(4,3,3,3,3,3,
3,3,3,3,3,3,3,3,3,3,3,3,3,3,3,3,3,3,3,4),(-1.48622659852799E-5,0.000610199395319616,
0.00119886177892042,0.00174545418326133,0.00178752416252122,0.00196068261362535,
0.00248416090974261,0.00298752987926026,0.00346663178416926,0.00358991059102772,
0.00387008960346663,0.0042497114937252,0.00449110380528096,0.00477985713902406,
0.00508715459760339,0.00539229701953421,0.00564558051974503,0.00589575931921666,
0.00613544593423836,0.00629349023378746,0.00645448223380467,0.00664036590499829,
0.00682033260015863,0.006994867143252,0.00716251291548491,0.00719468344804071),
 .UNSPECIFIED.);
#1768=B_SPLINE_CURVE_WITH_KNOTS('',3,(#12043,#12044,#12045,#12046,#12047,
#12048,#12049,#12050,#12051,#12052,#12053,#12054,#12055,#12056,#12057,#12058,
#12059,#12060,#12061,#12062,#12063,#12064,#12065,#12066,#12067,#12068,#12069,
#12070,#12071,#12072,#12073,#12074,#12075,#12076,#12077,#12078,#12079,#12080,
#12081,#12082),.UNSPECIFIED.,.F.,.F.,(4,3,3,3,3,3,3,3,3,3,3,3,3,4),(-1.31423244832953E-5,
0.000535751918458696,0.00105440310099963,0.00152703983355165,0.00193278669513403,
0.00195362085609607,0.00231730204521729,0.00265300264592743,0.00290575120494269,
0.00292287708750123,0.00323755006402069,0.00353412708048685,0.00381242976591801,
0.00387871571475135),.UNSPECIFIED.);
#1769=B_SPLINE_CURVE_WITH_KNOTS('',3,(#12084,#12085,#12086,#12087,#12088,
#12089,#12090,#12091,#12092,#12093,#12094,#12095,#12096,#12097,#12098,#12099,
#12100,#12101,#12102,#12103,#12104,#12105,#12106,#12107,#12108,#12109,#12110,
#12111,#12112,#12113,#12114,#12115,#12116,#12117,#12118,#12119,#12120,#12121,
#12122,#12123,#12124,#12125,#12126,#12127,#12128,#12129,#12130,#12131,#12132,
#12133,#12134,#12135,#12136,#12137,#12138,#12139,#12140,#12141,#12142,#12143,
#12144,#12145,#12146,#12147,#12148,#12149,#12150,#12151,#12152,#12153,#12154,
#12155,#12156,#12157,#12158,#12159,#12160,#12161,#12162),.UNSPECIFIED.,
 .F.,.F.,(4,3,3,3,3,3,3,3,3,3,3,3,3,3,3,3,3,3,3,3,3,3,3,3,3,3,4),(0.,0.000202743010861385,
0.000410514286393132,0.000626630076741744,0.000743751984502566,0.000896895697750052,
0.00116850905341496,0.00144756822846688,0.00154043258165826,0.0017937913955001,
0.00205677592735273,0.00233242599985535,0.00239862131095943,0.00272711606085617,
0.00307220744578745,0.00330563439814887,0.00358758279100021,0.00401837140748574,
0.00424614693708857,0.0046820333497003,0.0051562522094217,0.00521101431097235,
0.00538137418650031,0.00601866167817585,0.00627826988425036,0.00676573329750569,
0.00717516558200041),.UNSPECIFIED.);
#1770=B_SPLINE_CURVE_WITH_KNOTS('',3,(#12166,#12167,#12168,#12169,#12170,
#12171,#12172,#12173,#12174,#12175,#12176,#12177,#12178,#12179,#12180,#12181,
#12182,#12183,#12184,#12185,#12186,#12187,#12188,#12189,#12190,#12191,#12192,
#12193,#12194,#12195,#12196,#12197,#12198,#12199,#12200,#12201,#12202,#12203,
#12204,#12205),.UNSPECIFIED.,.F.,.F.,(4,3,3,3,3,3,3,3,3,3,3,3,3,4),(8.67361737988404E-19,
0.000280621540991916,0.000573887525927214,0.000891635349236454,0.000951755207402113,
0.000968821950376574,0.00129993329989704,0.00165663590861034,0.00191687066807323,
0.00193764390075315,0.00253097520314591,0.00313046485777404,0.0037404067077475,
0.00387528780150629),.UNSPECIFIED.);
#1771=B_SPLINE_CURVE_WITH_KNOTS('',3,(#12206,#12207,#12208,#12209,#12210,
#12211,#12212,#12213,#12214,#12215,#12216,#12217,#12218,#12219,#12220,#12221,
#12222,#12223,#12224,#12225,#12226,#12227,#12228,#12229,#12230,#12231,#12232,
#12233,#12234,#12235,#12236,#12237,#12238,#12239,#12240,#12241,#12242,#12243,
#12244,#12245,#12246,#12247,#12248,#12249,#12250,#12251,#12252,#12253,#12254,
#12255,#12256,#12257,#12258,#12259,#12260,#12261,#12262,#12263,#12264,#12265,
#12266,#12267,#12268,#12269,#12270,#12271,#12272,#12273,#12274,#12275,#12276,
#12277,#12278,#12279,#12280,#12281),.UNSPECIFIED.,.F.,.F.,(4,3,3,3,3,3,
3,3,3,3,3,3,3,3,3,3,3,3,3,3,3,3,3,3,3,4),(-1.48622659852334E-5,0.000610199394906132,
0.00119886177871369,0.00174545418209242,0.00178752416252126,0.0019606826136253,
0.00248416090948471,0.00298752987876159,0.00346663178346203,0.00358991059102774,
0.00387008960346665,0.0042497114937369,0.00449110380528099,0.00477985713902429,
0.00508715459758098,0.00539229701953424,0.0056455805197453,0.00589575931922801,
0.00613544593426095,0.00629349023378748,0.00645448223380473,0.00664036590499971,
0.00682033260016142,0.00699486714325674,0.00716251291549094,0.00719468344804073),
 .UNSPECIFIED.);
#1772=B_SPLINE_CURVE_WITH_KNOTS('',3,(#12284,#12285,#12286,#12287,#12288,
#12289,#12290,#12291,#12292,#12293,#12294,#12295,#12296,#12297,#12298,#12299,
#12300,#12301,#12302,#12303,#12304,#12305,#12306,#12307,#12308,#12309,#12310,
#12311,#12312,#12313,#12314,#12315,#12316,#12317,#12318,#12319,#12320,#12321,
#12322,#12323),.UNSPECIFIED.,.F.,.F.,(4,3,3,3,3,3,3,3,3,3,3,3,3,4),(-1.31423244832926E-5,
0.000535751919828975,0.00105440309942062,0.00152703982893435,0.00193278669513403,
0.00195362085609607,0.0023173020450886,0.00265300264570622,0.00290575120494269,
0.00292287708750123,0.00323755006398503,0.00353412708041696,0.00381242976581613,
0.00387871571475135),.UNSPECIFIED.);
#1773=B_SPLINE_CURVE_WITH_KNOTS('',3,(#12325,#12326,#12327,#12328,#12329,
#12330,#12331,#12332,#12333,#12334,#12335,#12336,#12337,#12338,#12339,#12340,
#12341,#12342,#12343,#12344,#12345,#12346,#12347,#12348,#12349,#12350,#12351,
#12352,#12353,#12354,#12355,#12356,#12357,#12358,#12359,#12360,#12361,#12362,
#12363,#12364,#12365,#12366,#12367,#12368,#12369,#12370,#12371,#12372,#12373,
#12374,#12375,#12376,#12377,#12378,#12379,#12380,#12381,#12382,#12383,#12384,
#12385,#12386,#12387,#12388,#12389,#12390,#12391,#12392,#12393,#12394,#12395,
#12396,#12397,#12398,#12399,#12400,#12401,#12402,#12403),.UNSPECIFIED.,
 .F.,.F.,(4,3,3,3,3,3,3,3,3,3,3,3,3,3,3,3,3,3,3,3,3,3,3,3,3,3,4),(4.33680868994202E-19,
0.00020274301087834,0.000410514286426467,0.0006266300767902,0.000743751984502697,
0.000896895697750054,0.00116850905345097,0.00144756822853142,0.0015404325816583,
0.00179379139550011,0.0020567759273478,0.00233242599984708,0.00239862131095955,
0.0027271160608669,0.00307220744580637,0.003305634398149,0.00358758279100022,
0.00401837140744728,0.00424614693708873,0.00468203334971685,0.00515625220941641,
0.00521101431097258,0.00538137418650032,0.00601866168041985,0.00627826988425037,
0.00676573329696348,0.00717516558200042),.UNSPECIFIED.);
#1774=B_SPLINE_CURVE_WITH_KNOTS('',3,(#12407,#12408,#12409,#12410,#12411,
#12412,#12413,#12414,#12415,#12416,#12417,#12418,#12419,#12420,#12421,#12422,
#12423,#12424,#12425,#12426,#12427,#12428,#12429,#12430,#12431,#12432,#12433,
#12434,#12435,#12436,#12437,#12438,#12439,#12440,#12441,#12442,#12443,#12444,
#12445,#12446),.UNSPECIFIED.,.F.,.F.,(4,3,3,3,3,3,3,3,3,3,3,3,3,4),(0.,
0.000280621541007288,0.000573887525957151,0.000891635349279514,0.000951755207402121,
0.000968821950376574,0.00129993329992634,0.00165663590867474,0.00191687066807322,
0.00193764390075315,0.00253097521731032,0.00313046488602104,0.00374040674787271,
0.00387528780150629),.UNSPECIFIED.);
#1775=B_SPLINE_CURVE_WITH_KNOTS('',3,(#12447,#12448,#12449,#12450,#12451,
#12452,#12453,#12454,#12455,#12456,#12457,#12458,#12459,#12460,#12461,#12462,
#12463,#12464,#12465,#12466,#12467,#12468,#12469,#12470,#12471,#12472,#12473,
#12474,#12475,#12476,#12477,#12478,#12479,#12480,#12481,#12482,#12483,#12484,
#12485,#12486,#12487,#12488,#12489,#12490,#12491,#12492,#12493,#12494,#12495,
#12496,#12497,#12498,#12499,#12500,#12501,#12502,#12503,#12504,#12505,#12506,
#12507,#12508,#12509,#12510,#12511,#12512,#12513,#12514,#12515,#12516,#12517,
#12518,#12519,#12520,#12521,#12522),.UNSPECIFIED.,.F.,.F.,(4,3,3,3,3,3,
3,3,3,3,3,3,3,3,3,3,3,3,3,3,3,3,3,3,3,4),(-1.48622659852434E-5,0.000610199394349477,
0.00119886177843536,0.00174545418627758,0.00178752416252125,0.00196068261362537,
0.00248416090955126,0.00298752987889132,0.00346663178364606,0.00358991059102774,
0.00387008960346671,0.00424971149374217,0.00449110380528099,0.00477985713902425,
0.00508715459758174,0.00539229701953423,0.0056455805197453,0.00589575931922186,
0.00613544593424759,0.00629349023378747,0.00645448223380475,0.00664036590499189,
0.00682033260014577,0.00699486714323308,0.00716251291545963,0.00719468344804072),
 .UNSPECIFIED.);
#1776=B_SPLINE_CURVE_WITH_KNOTS('',3,(#12524,#12525,#12526,#12527,#12528,
#12529,#12530,#12531,#12532,#12533,#12534,#12535,#12536,#12537,#12538,#12539,
#12540,#12541,#12542,#12543,#12544,#12545,#12546,#12547,#12548,#12549,#12550,
#12551,#12552,#12553,#12554,#12555,#12556,#12557,#12558,#12559,#12560,#12561,
#12562,#12563,#12564,#12565,#12566),.UNSPECIFIED.,.F.,.F.,(4,3,3,3,3,3,
3,3,3,3,3,3,3,3,4),(-1.52431972734697E-5,0.000577208204163697,0.00105830978603858,
0.00150240305466112,0.00189185074812808,0.00194649632328366,0.00203665697126444,
0.00241070485830692,0.00276264612286663,0.00292736608356222,0.00300995787129907,
0.0032503087048446,0.00348216857793395,0.00370167549194112,0.00390823584384079),
 .UNSPECIFIED.);
#1777=B_SPLINE_CURVE_WITH_KNOTS('',3,(#12567,#12568,#12569,#12570,#12571,
#12572,#12573,#12574,#12575,#12576,#12577,#12578,#12579,#12580,#12581,#12582,
#12583,#12584,#12585,#12586,#12587,#12588,#12589,#12590,#12591,#12592,#12593,
#12594,#12595,#12596,#12597,#12598,#12599,#12600,#12601,#12602,#12603,#12604,
#12605,#12606),.UNSPECIFIED.,.F.,.F.,(4,3,3,3,3,3,3,3,3,3,3,3,3,4),(0.,
0.000224425374774488,0.000451595406488995,0.000691860819929039,0.000897701499097952,
0.000980242722923431,0.00133024746974078,0.00170122585016282,0.00187037776501363,
0.00196048544584686,0.00235337437541891,0.00279968089665459,0.00329820841838201,
0.00392097089169372),.UNSPECIFIED.);
#1778=B_SPLINE_CURVE_WITH_KNOTS('',3,(#12609,#12610,#12611,#12612,#12613,
#12614,#12615,#12616,#12617,#12618,#12619,#12620,#12621,#12622,#12623,#12624,
#12625,#12626,#12627,#12628,#12629,#12630,#12631,#12632,#12633,#12634,#12635,
#12636,#12637,#12638,#12639,#12640,#12641,#12642,#12643,#12644,#12645,#12646,
#12647,#12648,#12649,#12650,#12651,#12652,#12653,#12654,#12655,#12656,#12657,
#12658,#12659,#12660,#12661,#12662,#12663,#12664,#12665,#12666,#12667,#12668,
#12669,#12670,#12671,#12672,#12673,#12674,#12675,#12676,#12677,#12678,#12679,
#12680,#12681,#12682,#12683,#12684,#12685,#12686,#12687,#12688,#12689,#12690,
#12691,#12692,#12693,#12694,#12695,#12696,#12697,#12698,#12699),
 .UNSPECIFIED.,.F.,.F.,(4,3,3,3,3,3,3,3,3,3,3,3,3,3,3,3,3,3,3,3,3,3,3,3,
3,3,3,3,3,3,4),(-2.02092030442042E-5,0.000556049295986959,0.00112171658044497,
0.00167096866058992,0.00219205980848149,0.00242674993854397,0.00286892709477413,
0.0032826544405976,0.00359051333580462,0.0039983380985113,0.00437342345626924,
0.00468974844460317,0.00504885723393916,0.00539155487817727,0.00570223157099643,
0.00596953869846973,0.00600761174928905,0.00621566605302244,0.00641489721149056,
0.00660361036060121,0.00661412836995868,0.00681882170158418,0.00701224857467793,
0.00717494882538604,0.00733318883750038,0.00739068892409895,0.00754723804309091,
0.00769433317590785,0.00783806436267558,0.00797708941080271,0.0080168854000668),
 .UNSPECIFIED.);
#1779=B_SPLINE_CURVE_WITH_KNOTS('',3,(#12700,#12701,#12702,#12703,#12704,
#12705,#12706),.UNSPECIFIED.,.F.,.F.,(4,3,4),(0.,0.000319771717937602,0.000495697630009084),
 .UNSPECIFIED.);
#1780=B_SPLINE_CURVE_WITH_KNOTS('',3,(#12708,#12709,#12710,#12711,#12712,
#12713,#12714),.UNSPECIFIED.,.F.,.F.,(4,3,4),(0.,0.000319771717612993,0.000495697630009086),
 .UNSPECIFIED.);
#1781=B_SPLINE_CURVE_WITH_KNOTS('',3,(#12715,#12716,#12717,#12718,#12719,
#12720,#12721,#12722,#12723,#12724,#12725,#12726,#12727,#12728,#12729,#12730,
#12731,#12732,#12733,#12734,#12735,#12736,#12737,#12738,#12739,#12740,#12741,
#12742,#12743,#12744,#12745,#12746,#12747,#12748,#12749,#12750,#12751,#12752,
#12753,#12754,#12755,#12756,#12757,#12758,#12759,#12760,#12761,#12762,#12763,
#12764,#12765,#12766,#12767,#12768,#12769,#12770,#12771,#12772,#12773,#12774,
#12775,#12776,#12777,#12778,#12779,#12780,#12781,#12782,#12783,#12784,#12785,
#12786,#12787,#12788,#12789,#12790,#12791,#12792,#12793,#12794,#12795,#12796,
#12797,#12798,#12799,#12800,#12801,#12802,#12803,#12804,#12805),
 .UNSPECIFIED.,.F.,.F.,(4,3,3,3,3,3,3,3,3,3,3,3,3,3,3,3,3,3,3,3,3,3,3,3,
3,3,3,3,3,3,4),(0.,0.000104117546061403,0.000212237259616963,0.000327080569137136,
0.000446149861995263,0.000572039848833935,0.000627770356649805,0.0007725910708947,
0.000921601146177619,0.00100643629586967,0.00123003713212734,0.00141082154631894,
0.00163414234169981,0.00186714353407499,0.00201287259173934,0.00230575771617008,
0.00232230404187754,0.00265209606179006,0.00299833864625774,0.00334106762005192,
0.00370526339370595,0.00402574518347867,0.00448446651998587,0.0049581923982794,
0.00545452540823567,0.00560736333266499,0.00603861777521801,0.00657098900349448,
0.00713145773781003,0.00771983125198687,0.00805149036695735),
 .UNSPECIFIED.);
#1782=B_SPLINE_CURVE_WITH_KNOTS('',3,(#12808,#12809,#12810,#12811,#12812,
#12813,#12814),.UNSPECIFIED.,.F.,.F.,(4,3,4),(4.9065389333868E-18,0.000319771718109916,
0.000495697630009092),.UNSPECIFIED.);
#1783=B_SPLINE_CURVE_WITH_KNOTS('',3,(#12815,#12816,#12817,#12818,#12819,
#12820,#12821,#12822,#12823,#12824,#12825,#12826,#12827,#12828,#12829,#12830,
#12831,#12832,#12833,#12834,#12835,#12836,#12837,#12838,#12839,#12840,#12841,
#12842,#12843,#12844,#12845,#12846,#12847,#12848,#12849,#12850,#12851,#12852,
#12853,#12854,#12855,#12856,#12857,#12858,#12859,#12860,#12861,#12862,#12863,
#12864,#12865,#12866,#12867,#12868,#12869,#12870,#12871,#12872,#12873,#12874,
#12875,#12876,#12877,#12878,#12879,#12880,#12881,#12882,#12883,#12884,#12885,
#12886,#12887,#12888,#12889,#12890,#12891,#12892,#12893,#12894,#12895,#12896,
#12897,#12898,#12899,#12900,#12901,#12902,#12903,#12904,#12905),
 .UNSPECIFIED.,.F.,.F.,(4,3,3,3,3,3,3,3,3,3,3,3,3,3,3,3,3,3,3,3,3,3,3,3,
3,3,3,3,3,3,4),(0.,0.000104117546066811,0.000212237259628058,0.000327080569154219,
0.000446149862018597,0.000572039848863917,0.000627770356652624,0.000772591070908048,
0.00092160114620273,0.00100643629586967,0.00123003713212771,0.00141082154631876,
0.00163414234169305,0.00186714353406425,0.00201287259173934,0.00230575771615584,
0.00232230404187742,0.00265209606176781,0.0029983386462177,0.00334106762005204,
0.0037052633937103,0.00402574518347868,0.00448446651999,0.00495819239828445,
0.00545452540823168,0.00560736333266521,0.00603861777521801,0.00657098900708674,
0.00713145774710329,0.00771983127025435,0.00805149036695735),
 .UNSPECIFIED.);
#1784=B_SPLINE_CURVE_WITH_KNOTS('',3,(#12907,#12908,#12909,#12910,#12911,
#12912,#12913,#12914,#12915,#12916,#12917,#12918,#12919,#12920,#12921,#12922,
#12923,#12924,#12925,#12926,#12927,#12928,#12929,#12930,#12931,#12932,#12933,
#12934,#12935,#12936,#12937,#12938,#12939,#12940,#12941,#12942,#12943,#12944,
#12945,#12946,#12947,#12948,#12949,#12950,#12951,#12952,#12953,#12954,#12955,
#12956,#12957,#12958,#12959,#12960,#12961,#12962,#12963,#12964,#12965,#12966,
#12967,#12968,#12969,#12970,#12971,#12972,#12973,#12974,#12975,#12976,#12977,
#12978,#12979,#12980,#12981,#12982,#12983,#12984,#12985,#12986,#12987,#12988,
#12989,#12990,#12991,#12992,#12993,#12994,#12995,#12996,#12997),
 .UNSPECIFIED.,.F.,.F.,(4,3,3,3,3,3,3,3,3,3,3,3,3,3,3,3,3,3,3,3,3,3,3,3,
3,3,3,3,3,3,4),(-2.02092030439489E-5,0.0005560492961748,0.00112171658075715,
0.00167096866098397,0.00219205980893471,0.00242674993854208,0.00286892709480559,
0.00328265444065681,0.00359051333580469,0.00399833809851155,0.0043734234562713,
0.00468974844460377,0.00504885723393179,0.00539155487816009,0.00570223157099668,
0.00596953869847231,0.0060076117492893,0.00621566605302207,0.00641489721149059,
0.00660361036059884,0.00661412836995911,0.0068188217015917,0.00701224857467817,
0.00717494882540412,0.00733318883753838,0.00739068892409721,0.00754723804308967,
0.0076943331759223,0.00783806436270549,0.0079770894108481,0.00801688540006705),
 .UNSPECIFIED.);
#1785=B_SPLINE_CURVE_WITH_KNOTS('',3,(#12998,#12999,#13000,#13001,#13002,
#13003,#13004),.UNSPECIFIED.,.F.,.F.,(4,3,4),(0.,0.000319771717956473,0.00049569763000909),
 .UNSPECIFIED.);
#1786=B_SPLINE_CURVE_WITH_KNOTS('',3,(#13007,#13008,#13009,#13010,#13011,
#13012),.UNSPECIFIED.,.F.,.F.,(4,2,4),(-0.142729181026185,-0.071107498865174,
-1.0000000814081E-6),.UNSPECIFIED.);
#1787=B_SPLINE_CURVE_WITH_KNOTS('',3,(#13014,#13015,#13016,#13017,#13018,
#13019,#13020,#13021,#13022,#13023,#13024,#13025,#13026,#13027,#13028,#13029),
 .UNSPECIFIED.,.F.,.F.,(4,2,2,2,2,2,2,4),(-2.43104855077894,-1.90349401615095,
-1.45644570848823,-1.0906282720009,-0.723808102624486,-0.376722226194699,
-0.186648168518619,0.),.UNSPECIFIED.);
#1788=B_SPLINE_CURVE_WITH_KNOTS('',3,(#13031,#13032,#13033,#13034,#13035,
#13036,#13037,#13038,#13039,#13040,#13041,#13042,#13043,#13044,#13045,#13046),
 .UNSPECIFIED.,.F.,.F.,(4,2,2,2,2,2,2,4),(-1.61608002817239,-1.45775061306008,
-1.2995571050224,-1.06365376510753,-0.82576780359447,-0.617872986252087,
-0.355668197463031,0.),.UNSPECIFIED.);
#1789=B_SPLINE_CURVE_WITH_KNOTS('',3,(#13047,#13048,#13049,#13050,#13051,
#13052),.UNSPECIFIED.,.F.,.F.,(4,2,4),(-0.152773347352654,-0.0766837717947395,
0.),.UNSPECIFIED.);
#1790=B_SPLINE_CURVE_WITH_KNOTS('',3,(#25576,#25577,#25578,#25579,#25580,
#25581,#25582,#25583,#25584,#25585),.UNSPECIFIED.,.F.,.F.,(4,2,2,2,4),(0.263724731228934,
0.278450074781171,0.366228167882972,0.454006260984773,0.46873160453701),
 .UNSPECIFIED.);
#1791=B_SPLINE_CURVE_WITH_KNOTS('',3,(#25587,#25588,#25589,#25590,#25591,
#25592,#25593,#25594,#25595,#25596),.UNSPECIFIED.,.F.,.F.,(4,2,2,2,4),(0.263724731228934,
0.27845007478117,0.366228167882972,0.454006260984773,0.468731604537009),
 .UNSPECIFIED.);
#1792=B_SPLINE_CURVE_WITH_KNOTS('',3,(#25598,#25599,#25600,#25601,#25602,
#25603,#25604,#25605,#25606,#25607),.UNSPECIFIED.,.F.,.F.,(4,2,2,2,4),(0.263724731228934,
0.27845007478117,0.366228167882972,0.454006260984773,0.468731604537009),
 .UNSPECIFIED.);
#1793=B_SPLINE_CURVE_WITH_KNOTS('',3,(#25609,#25610,#25611,#25612,#25613,
#25614,#25615,#25616,#25617,#25618),.UNSPECIFIED.,.F.,.F.,(4,2,2,2,4),(0.263724731228934,
0.27845007478117,0.366228167882972,0.454006260984773,0.46873160453701),
 .UNSPECIFIED.);
#1794=B_SPLINE_CURVE_WITH_KNOTS('',3,(#25620,#25621,#25622,#25623,#25624,
#25625,#25626,#25627,#25628,#25629),.UNSPECIFIED.,.F.,.F.,(4,2,2,2,4),(0.263724731228934,
0.278450074781171,0.366228167882972,0.454006260984773,0.46873160453701),
 .UNSPECIFIED.);
#1795=B_SPLINE_CURVE_WITH_KNOTS('',3,(#25631,#25632,#25633,#25634,#25635,
#25636,#25637,#25638,#25639,#25640),.UNSPECIFIED.,.F.,.F.,(4,2,2,2,4),(0.263724731228934,
0.27845007478117,0.366228167882972,0.454006260984773,0.46873160453701),
 .UNSPECIFIED.);
#1796=B_SPLINE_CURVE_WITH_KNOTS('',3,(#25683,#25684,#25685,#25686,#25687,
#25688,#25689,#25690,#25691,#25692,#25693,#25694,#25695,#25696,#25697,#25698,
#25699,#25700,#25701,#25702,#25703,#25704,#25705,#25706,#25707,#25708,#25709,
#25710,#25711,#25712,#25713,#25714,#25715,#25716,#25717,#25718,#25719,#25720,
#25721,#25722,#25723,#25724,#25725,#25726,#25727,#25728,#25729,#25730,#25731,
#25732,#25733,#25734,#25735,#25736,#25737,#25738,#25739,#25740,#25741,#25742,
#25743,#25744,#25745,#25746,#25747,#25748,#25749,#25750,#25751,#25752),
 .UNSPECIFIED.,.F.,.F.,(4,3,3,3,3,3,3,3,3,3,3,3,3,3,3,3,3,3,3,3,3,3,3,4),
(3.14159265358979,3.21339939141241,3.28586680785268,3.35121436883213,3.42308378055159,
3.49600214093481,3.54876098024507,3.62076596894727,3.69731507009814,3.77134555075139,
3.84915396215108,3.92696237355076,4.00138616900808,4.07733349290367,4.15127434963696,
4.2282249071137,4.30037597555225,4.30517546459045,4.37937215290707,4.45279559418716,
4.52509277844413,4.59683140040149,4.66795343860946,4.71238898038469),
 .UNSPECIFIED.);
#1797=B_SPLINE_CURVE_WITH_KNOTS('',3,(#25789,#25790,#25791,#25792,#25793,
#25794,#25795,#25796,#25797,#25798,#25799,#25800,#25801,#25802,#25803,#25804,
#25805,#25806,#25807,#25808,#25809,#25810,#25811,#25812,#25813,#25814,#25815,
#25816,#25817,#25818,#25819,#25820,#25821,#25822,#25823,#25824,#25825,#25826,
#25827,#25828,#25829,#25830,#25831,#25832,#25833,#25834,#25835,#25836,#25837,
#25838,#25839,#25840,#25841,#25842,#25843,#25844,#25845,#25846,#25847,#25848,
#25849,#25850,#25851,#25852,#25853,#25854,#25855,#25856,#25857,#25858),
 .UNSPECIFIED.,.F.,.F.,(4,3,3,3,3,3,3,3,3,3,3,3,3,3,3,3,3,3,3,3,3,3,3,4),
(3.14159265358979,3.21339939141199,3.28586680785193,3.35121436883206,3.42308378055094,
3.49600214093364,3.54876098024493,3.62076596894664,3.69731507009761,3.77134555075049,
3.84915396215049,3.92696237355049,4.00138616900755,4.0773334929032,4.15127434963635,
4.22822490711326,4.30037597555205,4.30517546459017,4.37937215290745,4.4527955941884,
4.52509277844676,4.59683140040586,4.6679534386157,4.71238898038469),
 .UNSPECIFIED.);
#1798=B_SPLINE_CURVE_WITH_KNOTS('',3,(#25922,#25923,#25924,#25925,#25926,
#25927,#25928,#25929,#25930,#25931,#25932,#25933,#25934,#25935,#25936,#25937,
#25938,#25939,#25940,#25941,#25942,#25943,#25944,#25945,#25946,#25947,#25948,
#25949,#25950,#25951,#25952,#25953,#25954,#25955,#25956,#25957,#25958,#25959,
#25960,#25961,#25962,#25963,#25964,#25965,#25966,#25967,#25968,#25969,#25970,
#25971,#25972,#25973,#25974,#25975,#25976,#25977,#25978,#25979,#25980,#25981,
#25982,#25983,#25984,#25985,#25986,#25987,#25988,#25989,#25990,#25991),
 .UNSPECIFIED.,.F.,.F.,(4,3,3,3,3,3,3,3,3,3,3,3,3,3,3,3,3,3,3,3,3,3,3,4),
(1.5707963267949,1.64187501429286,1.71337342981178,1.78582694190062,1.8589079472425,
1.93301112893021,1.9780098425893,2.05029693877859,2.12677843749119,2.20103698011073,
2.27862995686985,2.35622293362897,2.43057368240882,2.50653634354026,2.58022474803207,
2.65321980989102,2.72512224828116,2.73442432693459,2.80750100759831,2.87952975922344,
2.93197093834749,3.00457650346194,3.07649190731354,3.14159265358979),
 .UNSPECIFIED.);
#1799=B_SPLINE_CURVE_WITH_KNOTS('',3,(#26028,#26029,#26030,#26031,#26032,
#26033,#26034,#26035,#26036,#26037,#26038,#26039,#26040,#26041,#26042,#26043,
#26044,#26045,#26046,#26047,#26048,#26049,#26050,#26051,#26052,#26053,#26054,
#26055,#26056,#26057,#26058,#26059,#26060,#26061,#26062,#26063,#26064,#26065,
#26066,#26067,#26068,#26069,#26070,#26071,#26072,#26073,#26074,#26075,#26076,
#26077,#26078,#26079,#26080,#26081,#26082,#26083,#26084,#26085,#26086,#26087,
#26088,#26089,#26090,#26091,#26092,#26093,#26094,#26095,#26096,#26097),
 .UNSPECIFIED.,.F.,.F.,(4,3,3,3,3,3,3,3,3,3,3,3,3,3,3,3,3,3,3,3,3,3,3,4),
(1.5707963267949,1.64187501429421,1.71337342981444,1.78582694190426,1.85890794724695,
1.93301112893518,1.97800984258945,2.05029693877866,2.12677843749128,2.20103698011052,
2.27862995686982,2.35622293362912,2.43057368240835,2.50653634353993,2.5802247480312,
2.65321980988953,2.7251222482791,2.73442432693468,2.80750100759807,2.8795297592228,
2.93197093834753,3.00457650346134,3.07649190731224,3.14159265358979),
 .UNSPECIFIED.);
#1800=B_SPLINE_CURVE_WITH_KNOTS('',3,(#26167,#26168,#26169,#26170,#26171,
#26172,#26173,#26174,#26175,#26176,#26177,#26178,#26179,#26180,#26181,#26182,
#26183,#26184,#26185,#26186,#26187,#26188,#26189,#26190,#26191,#26192,#26193,
#26194,#26195,#26196,#26197,#26198,#26199,#26200,#26201,#26202,#26203,#26204,
#26205,#26206,#26207,#26208,#26209,#26210,#26211,#26212,#26213,#26214,#26215,
#26216,#26217,#26218,#26219,#26220,#26221,#26222,#26223,#26224,#26225,#26226,
#26227,#26228,#26229,#26230,#26231,#26232,#26233,#26234,#26235,#26236),
 .UNSPECIFIED.,.F.,.F.,(4,3,3,3,3,3,3,3,3,3,3,3,3,3,3,3,3,3,3,3,3,3,3,4),
(1.5707963267949,1.64187501429494,1.7133734298158,1.78582694190613,1.85890794724926,
1.93301112893768,1.97800984258967,2.0502969387789,2.1267784374915,2.20103698011077,
2.27862995687003,2.35622293362928,2.43057368240896,2.50653634354039,2.58022474803194,
2.65321980989038,2.72512224827995,2.7344243269347,2.80750100759699,2.87952975922006,
2.93197093834751,3.00457650346208,3.07649190731386,3.14159265358979),
 .UNSPECIFIED.);
#1801=B_SPLINE_CURVE_WITH_KNOTS('',3,(#26273,#26274,#26275,#26276,#26277,
#26278,#26279,#26280,#26281,#26282,#26283,#26284,#26285,#26286,#26287,#26288,
#26289,#26290,#26291,#26292,#26293,#26294,#26295,#26296,#26297,#26298,#26299,
#26300,#26301,#26302,#26303,#26304,#26305,#26306,#26307,#26308,#26309,#26310,
#26311,#26312,#26313,#26314,#26315,#26316,#26317,#26318,#26319,#26320,#26321,
#26322,#26323,#26324,#26325,#26326,#26327,#26328,#26329,#26330,#26331,#26332,
#26333,#26334,#26335,#26336,#26337,#26338,#26339,#26340,#26341,#26342),
 .UNSPECIFIED.,.F.,.F.,(4,3,3,3,3,3,3,3,3,3,3,3,3,3,3,3,3,3,3,3,3,3,3,4),
(1.5707963267949,1.64187501429417,1.71337342981437,1.7858269419042,1.85890794724684,
1.9330111289351,1.97800984258951,2.05029693877879,2.12677843749138,2.20103698011076,
2.27862995686996,2.35622293362916,2.43057368240866,2.50653634354016,2.58022474803158,
2.6532198098899,2.72512224827938,2.73442432693467,2.80750100759708,2.87952975922029,
2.93197093834752,3.00457650346242,3.07649190731442,3.14159265358979),
 .UNSPECIFIED.);
#1802=B_SPLINE_CURVE_WITH_KNOTS('',3,(#26463,#26464,#26465,#26466,#26467,
#26468,#26469,#26470,#26471,#26472,#26473,#26474,#26475,#26476,#26477,#26478,
#26479,#26480,#26481,#26482,#26483,#26484,#26485,#26486,#26487,#26488,#26489,
#26490,#26491,#26492,#26493,#26494,#26495,#26496,#26497,#26498,#26499,#26500,
#26501,#26502,#26503,#26504,#26505,#26506,#26507,#26508,#26509,#26510,#26511,
#26512,#26513,#26514,#26515,#26516,#26517,#26518,#26519,#26520,#26521,#26522,
#26523,#26524,#26525,#26526,#26527,#26528,#26529,#26530,#26531,#26532),
 .UNSPECIFIED.,.F.,.F.,(4,3,3,3,3,3,3,3,3,3,3,3,3,3,3,3,3,3,3,3,3,3,3,4),
(1.5707963267949,1.64187501429396,1.71337342981397,1.78582694190369,1.85890794724632,
1.93301112893457,1.97800984258952,2.050296938779,2.12677843749157,2.20103698011112,
2.27862995687019,2.35622293362926,2.43057368240902,2.50653634354047,2.5802247480321,
2.65321980989075,2.72512224828034,2.73442432693481,2.8075010075973,2.87952975922036,
2.93197093834763,3.00457650346015,3.07649190730919,3.14159265358979),
 .UNSPECIFIED.);
#1803=B_SPLINE_CURVE_WITH_KNOTS('',3,(#26607,#26608,#26609,#26610,#26611,
#26612,#26613,#26614,#26615,#26616,#26617,#26618,#26619,#26620,#26621,#26622,
#26623,#26624,#26625,#26626,#26627,#26628,#26629,#26630,#26631,#26632,#26633,
#26634,#26635,#26636,#26637,#26638,#26639,#26640,#26641,#26642,#26643,#26644,
#26645,#26646,#26647,#26648,#26649,#26650,#26651,#26652,#26653,#26654,#26655,
#26656,#26657,#26658,#26659,#26660,#26661,#26662,#26663,#26664,#26665,#26666,
#26667,#26668,#26669,#26670,#26671,#26672,#26673,#26674,#26675,#26676),
 .UNSPECIFIED.,.F.,.F.,(4,3,3,3,3,3,3,3,3,3,3,3,3,3,3,3,3,3,3,3,3,3,3,4),
(1.5707963267949,1.64187501429392,1.7133734298141,1.78582694190386,1.85890794724665,
1.93301112893493,1.97800984258952,2.05029693877883,2.12677843749144,2.20103698011099,
2.27862995687012,2.35622293362926,2.43057368240907,2.50653634354051,2.5802247480322,
2.65321980989064,2.72512224828023,2.73442432693482,2.8075010075969,2.87952975921948,
2.93197093834763,3.00457650346027,3.07649190730933,3.14159265358979),
 .UNSPECIFIED.);
#1804=B_SPLINE_CURVE_WITH_KNOTS('',3,(#26797,#26798,#26799,#26800,#26801,
#26802,#26803,#26804,#26805,#26806,#26807,#26808,#26809,#26810,#26811,#26812,
#26813,#26814,#26815,#26816,#26817,#26818,#26819,#26820,#26821,#26822,#26823,
#26824,#26825,#26826,#26827,#26828,#26829,#26830,#26831,#26832,#26833,#26834,
#26835,#26836,#26837,#26838,#26839,#26840,#26841,#26842,#26843,#26844,#26845,
#26846,#26847,#26848,#26849,#26850,#26851,#26852,#26853,#26854,#26855,#26856,
#26857,#26858,#26859,#26860,#26861,#26862,#26863,#26864,#26865,#26866),
 .UNSPECIFIED.,.F.,.F.,(4,3,3,3,3,3,3,3,3,3,3,3,3,3,3,3,3,3,3,3,3,3,3,4),
(1.5707963267949,1.6418750142939,1.71337342981391,1.78582694190352,1.85890794724598,
1.93301112893406,1.97800984258953,2.05029693877889,2.12677843749147,2.20103698011073,
2.27862995686996,2.3562229336292,2.43057368240849,2.50653634354004,2.58022474803132,
2.65321980988968,2.72512224827939,2.73442432693471,2.80750100759801,2.87952975922287,
2.93197093834755,3.00457650346109,3.07649190731183,3.14159265358979),
 .UNSPECIFIED.);
#1805=B_SPLINE_CURVE_WITH_KNOTS('',3,(#26903,#26904,#26905,#26906,#26907,
#26908,#26909,#26910,#26911,#26912,#26913,#26914,#26915,#26916,#26917,#26918,
#26919,#26920,#26921,#26922,#26923,#26924,#26925,#26926,#26927,#26928,#26929,
#26930,#26931,#26932,#26933,#26934,#26935,#26936,#26937,#26938,#26939,#26940,
#26941,#26942,#26943,#26944,#26945,#26946,#26947,#26948,#26949,#26950,#26951,
#26952,#26953,#26954,#26955,#26956,#26957,#26958,#26959,#26960,#26961,#26962,
#26963,#26964,#26965,#26966,#26967,#26968,#26969,#26970,#26971,#26972),
 .UNSPECIFIED.,.F.,.F.,(4,3,3,3,3,3,3,3,3,3,3,3,3,3,3,3,3,3,3,3,3,3,3,4),
(1.5707963267949,1.64187501429531,1.71337342981643,1.78582694190706,1.85890794725031,
1.9330111289389,1.97800984258968,2.05029693877943,2.12677843749192,2.2010369801112,
2.27862995687028,2.35622293362937,2.4305736824087,2.50653634354023,2.5802247480316,
2.65321980989009,2.72512224827981,2.73442432693483,2.80750100759733,2.87952975922097,
2.93197093834762,3.00457650346007,3.0764919073093,3.14159265358979),
 .UNSPECIFIED.);
#1806=B_SPLINE_CURVE_WITH_KNOTS('',3,(#27294,#27295,#27296,#27297,#27298,
#27299,#27300,#27301,#27302,#27303,#27304,#27305,#27306,#27307,#27308,#27309,
#27310,#27311,#27312,#27313,#27314,#27315,#27316,#27317,#27318,#27319,#27320,
#27321,#27322,#27323,#27324,#27325,#27326,#27327,#27328,#27329,#27330,#27331,
#27332,#27333,#27334,#27335,#27336,#27337,#27338,#27339,#27340,#27341,#27342,
#27343,#27344,#27345,#27346,#27347,#27348,#27349,#27350,#27351,#27352,#27353,
#27354,#27355,#27356,#27357,#27358,#27359,#27360,#27361,#27362,#27363,#27364,
#27365,#27366,#27367,#27368,#27369,#27370,#27371,#27372,#27373,#27374,#27375,
#27376,#27377,#27378,#27379,#27380,#27381,#27382,#27383,#27384,#27385,#27386,
#27387,#27388,#27389,#27390,#27391,#27392,#27393,#27394,#27395,#27396,#27397,
#27398,#27399,#27400,#27401,#27402,#27403,#27404,#27405,#27406,#27407,#27408,
#27409,#27410,#27411,#27412,#27413,#27414,#27415,#27416,#27417,#27418,#27419,
#27420,#27421,#27422,#27423,#27424,#27425,#27426,#27427,#27428,#27429,#27430,
#27431,#27432,#27433,#27434,#27435,#27436,#27437,#27438,#27439,#27440,#27441,
#27442,#27443,#27444,#27445,#27446,#27447,#27448,#27449,#27450,#27451,#27452,
#27453,#27454,#27455,#27456,#27457,#27458,#27459,#27460,#27461,#27462,#27463,
#27464,#27465),.UNSPECIFIED.,.F.,.F.,(4,3,3,3,3,3,3,3,3,3,3,3,3,3,3,3,3,
3,3,3,3,3,3,3,3,3,3,3,3,3,3,3,3,3,3,3,3,3,3,3,3,3,3,3,3,3,3,3,3,3,3,3,3,
3,3,3,3,4),(0.0161972991085284,0.0165394666975099,0.0168809221214402,0.0172044026463048,
0.0176094804041076,0.0180166563712003,0.0182115061840812,0.019004889187358,
0.0192186097218576,0.0195483730729979,0.0198870431663159,0.020225713259634,
0.0205303601960963,0.0208345896758242,0.0211387162338752,0.0212328167974104,
0.0215681677457675,0.0219040440404771,0.0222399203351868,0.0224639690092825,
0.0226878387172806,0.022743472104075,0.0230854328330104,0.0232470238729632,
0.0235831943749047,0.0237505756418514,0.023959762309833,0.0241688808757419,
0.0242541274107396,0.0245936504558835,0.0249356019729133,0.025261230948516,
0.025525825317406,0.0257903817038414,0.026055729922731,0.0262683344862924,
0.0266058569357826,0.0269447878928871,0.0272754380240688,0.0275032853685415,
0.0277312867104389,0.027778989792957,0.0281109815849333,0.0282825415618451,
0.0286824722061837,0.0290770552629352,0.0292896450996216,0.029623506776701,
0.0299601277070495,0.030296748637398,0.0305741027539414,0.0308509225425318,
0.031127629650921,0.0313038521751744,0.0316222885798555,0.0319394577071118,
0.0322532614556433,0.0323109557129508),.UNSPECIFIED.);
#1807=B_SPLINE_CURVE_WITH_KNOTS('',3,(#27469,#27470,#27471,#27472,#27473,
#27474,#27475,#27476,#27477,#27478,#27479,#27480,#27481,#27482,#27483,#27484,
#27485,#27486,#27487,#27488,#27489,#27490,#27491,#27492,#27493,#27494,#27495,
#27496,#27497,#27498,#27499,#27500,#27501,#27502,#27503,#27504,#27505,#27506,
#27507,#27508,#27509,#27510,#27511,#27512,#27513,#27514,#27515,#27516,#27517,
#27518,#27519,#27520,#27521,#27522,#27523,#27524,#27525,#27526,#27527,#27528,
#27529,#27530,#27531,#27532,#27533,#27534,#27535,#27536,#27537,#27538,#27539,
#27540,#27541,#27542,#27543,#27544,#27545,#27546,#27547,#27548,#27549,#27550),
 .UNSPECIFIED.,.F.,.F.,(4,3,3,3,3,3,3,3,3,3,3,3,3,3,3,3,3,3,3,3,3,3,3,3,
3,3,3,4),(0.00890915223960435,0.0094204624297249,0.00946241028514952,0.00998728674902293,
0.0100156683306947,0.0105532850043369,0.0105689263762399,0.0111184026693338,
0.0111221844217851,0.0119717719779961,0.0122287005128754,0.0122437820923162,
0.0128330281524603,0.0133352166039658,0.0133620354339848,0.0140734232108796,
0.0144417326950561,0.0144721766299634,0.0151217140130995,0.0155482487861465,
0.0155745146428516,0.0161015068316917,0.0161230651642655,0.0166190777279675,
0.0166547648772369,0.0166698085595632,0.0173648818539917,0.0177612809683272),
 .UNSPECIFIED.);
#1808=B_SPLINE_CURVE_WITH_KNOTS('',3,(#27552,#27553,#27554,#27555,#27556,
#27557,#27558,#27559,#27560,#27561,#27562,#27563,#27564,#27565,#27566,#27567,
#27568,#27569,#27570,#27571),.UNSPECIFIED.,.F.,.F.,(4,2,2,2,2,2,2,2,2,4),
(0.0355734865786901,0.0366931658727571,0.037812845166824,0.0389325244608909,
0.0400522037549579,0.0406120434019913,0.0411718830490248,0.0422915623430917,
0.0434112416371587,0.0445309209312256),.UNSPECIFIED.);
#1809=B_SPLINE_CURVE_WITH_KNOTS('',3,(#27574,#27575,#27576,#27577),
 .UNSPECIFIED.,.F.,.F.,(4,4),(0.,4.45846292526202E-5),.UNSPECIFIED.);
#1810=B_SPLINE_CURVE_WITH_KNOTS('',3,(#27706,#27707,#27708,#27709,#27710,
#27711,#27712,#27713,#27714,#27715,#27716,#27717,#27718,#27719,#27720,#27721,
#27722,#27723,#27724,#27725,#27726,#27727,#27728,#27729,#27730,#27731,#27732,
#27733,#27734,#27735,#27736,#27737,#27738,#27739,#27740,#27741,#27742,#27743,
#27744,#27745,#27746,#27747,#27748,#27749,#27750,#27751,#27752,#27753,#27754,
#27755,#27756,#27757,#27758,#27759,#27760,#27761,#27762,#27763,#27764,#27765,
#27766,#27767,#27768,#27769,#27770,#27771,#27772,#27773,#27774,#27775,#27776,
#27777,#27778,#27779,#27780,#27781,#27782,#27783,#27784,#27785,#27786,#27787,
#27788,#27789,#27790),.UNSPECIFIED.,.F.,.F.,(4,3,3,3,3,3,3,3,3,3,3,3,3,
3,3,3,3,3,3,3,3,3,3,3,3,3,3,3,4),(0.0163404601436347,0.0173256833684261,
0.0173478922432849,0.0177073599341222,0.0178182949808219,0.0178520374467346,
0.0182545320008027,0.0183109065932176,0.0183567651649381,0.0187303101652621,
0.0191065909074555,0.0192961298180091,0.0193676144802671,0.0197533601995195,
0.0201449367067774,0.0202813530428006,0.0203798282124602,0.021266576267592,
0.0213919424331495,0.0222517994923835,0.0224025672000064,0.0229070517959347,
0.023237022717175,0.0234111125329635,0.0236644536869744,0.0237804896972582,
0.0239146520071729,0.0242030183124513,0.0242222459419665),.UNSPECIFIED.);
#1811=B_SPLINE_CURVE_WITH_KNOTS('',3,(#27794,#27795,#27796,#27797,#27798,
#27799,#27800,#27801,#27802,#27803,#27804,#27805,#27806,#27807,#27808,#27809,
#27810,#27811,#27812,#27813,#27814,#27815,#27816,#27817,#27818,#27819,#27820,
#27821,#27822,#27823,#27824,#27825,#27826,#27827,#27828,#27829,#27830,#27831,
#27832,#27833,#27834,#27835,#27836,#27837,#27838,#27839,#27840,#27841,#27842,
#27843,#27844,#27845,#27846,#27847,#27848,#27849,#27850,#27851,#27852,#27853,
#27854,#27855,#27856,#27857,#27858,#27859,#27860,#27861,#27862,#27863,#27864,
#27865,#27866,#27867,#27868,#27869,#27870,#27871,#27872,#27873,#27874,#27875,
#27876,#27877,#27878,#27879,#27880,#27881,#27882,#27883,#27884,#27885,#27886,
#27887,#27888,#27889,#27890,#27891,#27892,#27893,#27894,#27895,#27896,#27897,
#27898,#27899,#27900,#27901,#27902,#27903,#27904,#27905,#27906,#27907,#27908,
#27909,#27910,#27911,#27912,#27913,#27914,#27915,#27916,#27917,#27918,#27919,
#27920,#27921,#27922,#27923,#27924,#27925,#27926,#27927,#27928,#27929,#27930,
#27931,#27932,#27933,#27934,#27935,#27936,#27937,#27938,#27939,#27940,#27941,
#27942,#27943,#27944,#27945,#27946,#27947,#27948,#27949,#27950,#27951,#27952,
#27953,#27954,#27955,#27956,#27957,#27958,#27959,#27960,#27961,#27962,#27963,
#27964,#27965,#27966,#27967,#27968,#27969,#27970,#27971,#27972,#27973,#27974,
#27975,#27976,#27977,#27978,#27979,#27980,#27981,#27982,#27983,#27984,#27985,
#27986),.UNSPECIFIED.,.F.,.F.,(4,3,3,3,3,3,3,3,3,3,3,3,3,3,3,3,3,3,3,3,
3,3,3,3,3,3,3,3,3,3,3,3,3,3,3,3,3,3,3,3,3,3,3,3,3,3,3,3,3,3,3,3,3,3,3,3,
3,3,3,3,3,3,3,3,4),(0.,0.000476483257676747,0.000920430129810064,0.00110270427003711,
0.0016586651891166,0.00205477723046485,0.00220540854007422,0.00261403414264452,
0.00302622462762113,0.00318437350442038,0.00330811281011133,0.00369591663725892,
0.00408676590346633,0.00430673855116764,0.00441081708014843,0.0048197443595792,
0.00486501447903157,0.00496216921516699,0.00531164477891051,0.00542124469901969,
0.00551352135018555,0.00602068054519799,0.00652783974021042,0.00661622562022266,
0.00701845057040251,0.00743031416521327,0.00762708503273923,0.00771892989025977,
0.00822053759859568,0.00872214530693159,0.00882163416029687,0.00911084512080088,
0.00926867571247231,0.00937298629531544,0.00981572542009721,0.009924338430334,
0.0102952256348079,0.0103637517719452,0.0104756905653526,0.0107825930307397,
0.0109128329030101,0.0110270427003711,0.0118184582616005,0.0120162612334194,
0.0121297469704082,0.012410398075847,0.0126810991054268,0.0130200359460735,
0.0131274071843423,0.0132324512404454,0.0136546231592765,0.0140734930528288,
0.0142469357400738,0.0143351555104825,0.0147312308823071,0.0151293577222552,
0.0153736058156945,0.0154378597805196,0.0158451722172866,0.0159393472249651,
0.0159892119155382,0.0164350035042047,0.0165066770945964,0.0165405640505567,
0.0176432683205938),.UNSPECIFIED.);
#1812=B_SPLINE_CURVE_WITH_KNOTS('',3,(#27991,#27992,#27993,#27994,#27995,
#27996,#27997,#27998,#27999,#28000,#28001,#28002,#28003,#28004,#28005,#28006,
#28007,#28008,#28009,#28010,#28011,#28012,#28013,#28014,#28015,#28016,#28017,
#28018,#28019,#28020,#28021,#28022,#28023,#28024,#28025,#28026,#28027,#28028,
#28029,#28030,#28031,#28032,#28033,#28034,#28035,#28036,#28037,#28038,#28039,
#28040,#28041,#28042,#28043,#28044,#28045,#28046,#28047,#28048,#28049,#28050,
#28051,#28052,#28053,#28054,#28055,#28056,#28057,#28058,#28059,#28060,#28061,
#28062,#28063,#28064,#28065,#28066,#28067,#28068,#28069,#28070,#28071,#28072,
#28073,#28074,#28075),.UNSPECIFIED.,.F.,.F.,(4,3,3,3,3,3,3,3,3,3,3,3,3,
3,3,3,3,3,3,3,3,3,3,3,3,3,3,3,4),(0.0242222459426628,0.0244180431366776,
0.0250670610002247,0.0252558702165362,0.0254257993687501,0.0258101580369982,
0.0261920397107803,0.0262894944911059,0.0264352581025446,0.0268818610381716,
0.0273231187656756,0.0274466088771079,0.0279527924666284,0.0283567430402452,
0.0284590391121063,0.0288583023070336,0.0292494335045575,0.0293903673148149,
0.0294708328719711,0.0298842927152321,0.0302930478895242,0.0304239915893846,
0.0304812062897893,0.0310833961140862,0.0314576158639543,0.0314886932089115,
0.0318206160521525,0.0321559280953382,0.032491240138524),.UNSPECIFIED.);
#1813=B_SPLINE_CURVE_WITH_KNOTS('',3,(#28089,#28090,#28091,#28092,#28093,
#28094,#28095,#28096,#28097,#28098,#28099,#28100,#28101,#28102,#28103,#28104,
#28105,#28106,#28107,#28108,#28109,#28110,#28111,#28112,#28113,#28114,#28115,
#28116,#28117,#28118,#28119,#28120,#28121,#28122,#28123,#28124,#28125,#28126,
#28127,#28128,#28129,#28130,#28131,#28132,#28133,#28134,#28135,#28136,#28137,
#28138,#28139,#28140,#28141,#28142,#28143,#28144,#28145,#28146,#28147,#28148,
#28149,#28150,#28151,#28152,#28153,#28154,#28155,#28156,#28157,#28158,#28159,
#28160,#28161,#28162,#28163,#28164),.UNSPECIFIED.,.F.,.F.,(4,3,3,3,3,3,
3,3,3,3,3,3,3,3,3,3,3,3,3,3,3,3,3,3,3,4),(0.00807103269296787,0.00826343092632988,
0.00876686013716756,0.00910471112411131,0.00927072398918449,0.0101383895554718,
0.0102800255304896,0.0106156018941836,0.010655228771152,0.0110644258204309,
0.0111720679868323,0.0112913127308201,0.0117973861554865,0.0122057464181927,
0.0123035593154063,0.0132394248495532,0.0133153163713804,0.0138374104952791,
0.0142731032809137,0.0143254514319448,0.0148760179492037,0.0153067817122742,
0.0153336346080776,0.0156869818471577,0.0160337318414785,0.0163404601436347),
 .UNSPECIFIED.);
#1814=B_SPLINE_CURVE_WITH_KNOTS('',3,(#28168,#28169,#28170,#28171,#28172,
#28173,#28174,#28175,#28176,#28177,#28178,#28179,#28180,#28181,#28182,#28183,
#28184,#28185,#28186,#28187,#28188,#28189,#28190,#28191,#28192,#28193,#28194,
#28195,#28196,#28197,#28198,#28199,#28200,#28201,#28202,#28203,#28204,#28205,
#28206,#28207,#28208,#28209,#28210,#28211,#28212,#28213,#28214,#28215,#28216,
#28217,#28218,#28219,#28220,#28221,#28222,#28223,#28224,#28225,#28226,#28227,
#28228,#28229,#28230,#28231,#28232,#28233,#28234,#28235,#28236,#28237,#28238,
#28239,#28240,#28241,#28242,#28243,#28244,#28245,#28246,#28247,#28248,#28249,
#28250,#28251,#28252,#28253,#28254,#28255,#28256,#28257,#28258,#28259,#28260,
#28261,#28262,#28263,#28264,#28265,#28266,#28267,#28268,#28269,#28270,#28271,
#28272,#28273,#28274,#28275,#28276,#28277,#28278,#28279,#28280,#28281,#28282,
#28283,#28284,#28285,#28286,#28287,#28288,#28289,#28290,#28291,#28292,#28293,
#28294,#28295,#28296,#28297,#28298,#28299,#28300,#28301,#28302,#28303,#28304,
#28305,#28306,#28307,#28308,#28309,#28310,#28311,#28312,#28313,#28314,#28315,
#28316,#28317,#28318,#28319,#28320,#28321),.UNSPECIFIED.,.F.,.F.,(4,3,3,
3,3,3,3,3,3,3,3,3,3,3,3,3,3,3,3,3,3,3,3,3,3,3,3,3,3,3,3,3,3,3,3,3,3,3,3,
3,3,3,3,3,3,3,3,3,3,3,3,4),(4.45846292526202E-5,0.00105045630092898,0.00105093952698816,
0.0014376794093111,0.00155285871031254,0.00191803247755761,0.00205655415239476,
0.0020572944247237,0.00279642434499595,0.00306364932245924,0.00306768917245999,
0.00383461365631528,0.00407000422019478,0.0040800681747585,0.00507635911793032,
0.00509211131047192,0.0055976346059631,0.00608271401566585,0.00610269177361662,
0.00658589146453362,0.00660721081063723,0.00699582755236498,0.00708906891340139,
0.00711120248307089,0.00772832521421459,0.00809542381113692,0.0081185518555815,
0.00854575157131149,0.00859860126000469,0.00862200314174437,0.00910177870887246,
0.00912580243443331,0.010108133606608,0.0101346994725071,0.0110502314226318,
0.0111144885043435,0.0111454360522996,0.0116514589397514,0.0121208434020791,
0.0121576802258181,0.0129515084587526,0.0131271982998146,0.0131700170813561,
0.013745821675725,0.0141335531975501,0.014181101651953,0.0147833538088824,
0.0151399080952856,0.0151901066138265,0.0155690496395463,0.0159361916298065,
0.0161462629930212),.UNSPECIFIED.);
#1815=B_SPLINE_CURVE_WITH_KNOTS('',3,(#28322,#28323,#28324,#28325,#28326,
#28327,#28328,#28329,#28330,#28331,#28332,#28333,#28334,#28335,#28336,#28337,
#28338,#28339,#28340,#28341,#28342,#28343),.UNSPECIFIED.,.F.,.F.,(4,2,2,
2,2,2,2,2,2,2,4),(0.000187655515302136,0.00117307766248322,0.00166578873607376,
0.00215849980966431,0.0031439219568454,0.00412934410402649,0.00511476625120758,
0.00610018839838867,0.00659289947197922,0.00708561054556976,0.00807103269275084),
 .UNSPECIFIED.);
#1816=B_SPLINE_CURVE_WITH_KNOTS('',3,(#28372,#28373,#28374,#28375,#28376,
#28377,#28378,#28379,#28380,#28381,#28382,#28383,#28384,#28385,#28386,#28387,
#28388,#28389,#28390,#28391,#28392,#28393,#28394,#28395,#28396,#28397,#28398,
#28399,#28400,#28401,#28402,#28403,#28404,#28405,#28406,#28407,#28408,#28409,
#28410,#28411,#28412,#28413,#28414,#28415,#28416,#28417,#28418,#28419,#28420,
#28421,#28422,#28423,#28424,#28425,#28426,#28427,#28428,#28429,#28430,#28431,
#28432,#28433,#28434,#28435,#28436,#28437,#28438,#28439,#28440,#28441,#28442,
#28443,#28444,#28445,#28446,#28447,#28448,#28449,#28450,#28451,#28452,#28453,
#28454,#28455,#28456,#28457,#28458,#28459),.UNSPECIFIED.,.F.,.F.,(4,3,3,
3,3,3,3,3,3,3,3,3,3,3,3,3,3,3,3,3,3,3,3,3,3,3,3,3,3,4),(0.0177612809683272,
0.0179912055960288,0.0182264943827035,0.018320985239376,0.0186309863592005,
0.0188517626649399,0.0188806895104249,0.0195327263331859,0.0199466791231638,
0.0200000980525225,0.0205240586547836,0.02100811078643,0.0210480192570447,
0.0211195065946202,0.0218330559323615,0.0221573969432929,0.0222389151367179,
0.0227150057367735,0.0232746671940726,0.0233583236788155,0.0240758493690848,
0.0243994308669159,0.0244777322209132,0.0254514724876917,0.025529773750765,
0.0255971407630109,0.0260964347561723,0.0261568450340597,0.0266638537201985,
0.0267165493051086),.UNSPECIFIED.);
#1817=B_SPLINE_CURVE_WITH_KNOTS('',3,(#28463,#28464,#28465,#28466,#28467,
#28468,#28469,#28470,#28471,#28472,#28473,#28474,#28475,#28476,#28477,#28478,
#28479,#28480,#28481,#28482,#28483,#28484,#28485,#28486,#28487,#28488,#28489,
#28490,#28491,#28492,#28493,#28494,#28495,#28496,#28497,#28498,#28499,#28500,
#28501,#28502,#28503,#28504,#28505,#28506,#28507,#28508,#28509,#28510,#28511,
#28512,#28513,#28514,#28515,#28516,#28517,#28518,#28519,#28520,#28521,#28522,
#28523,#28524,#28525,#28526,#28527,#28528,#28529,#28530,#28531,#28532,#28533,
#28534,#28535,#28536,#28537,#28538,#28539,#28540,#28541),.UNSPECIFIED.,
 .F.,.F.,(4,3,3,3,3,3,3,3,3,3,3,3,3,3,3,3,3,3,3,3,3,3,3,3,3,3,4),(0.0267165493051086,
0.0273773663586454,0.0277977530222155,0.0278236664643063,0.0283640328899012,
0.0283772250439051,0.0289289794857498,0.028930783623504,0.029492481704934,
0.0300379007827017,0.0300544056967581,0.0308713360248079,0.0311450179418994,
0.0311725469988184,0.0317293956286949,0.0322521351010971,0.0322826877003502,
0.0330325553019409,0.0333592522602948,0.033385001375028,0.0337665202189872,
0.0339128108398936,0.0339332548501144,0.0344663694194925,0.0344806499432494,
0.0353087686546496,0.0355734865786901),.UNSPECIFIED.);
#1818=B_SPLINE_CURVE_WITH_KNOTS('',3,(#28544,#28545,#28546,#28547,#28548,
#28549,#28550,#28551,#28552,#28553,#28554,#28555,#28556,#28557,#28558,#28559,
#28560,#28561,#28562,#28563,#28564,#28565,#28566,#28567,#28568,#28569,#28570,
#28571,#28572,#28573,#28574,#28575,#28576,#28577,#28578,#28579,#28580,#28581,
#28582,#28583,#28584,#28585,#28586,#28587,#28588,#28589,#28590,#28591,#28592,
#28593,#28594,#28595,#28596,#28597,#28598,#28599,#28600,#28601,#28602,#28603,
#28604,#28605,#28606,#28607,#28608,#28609,#28610,#28611,#28612,#28613,#28614,
#28615,#28616,#28617,#28618,#28619,#28620,#28621,#28622,#28623,#28624,#28625,
#28626,#28627,#28628,#28629,#28630,#28631,#28632,#28633,#28634,#28635,#28636,
#28637,#28638,#28639,#28640,#28641,#28642,#28643,#28644,#28645,#28646,#28647,
#28648,#28649,#28650,#28651,#28652,#28653,#28654,#28655,#28656,#28657,#28658,
#28659,#28660,#28661,#28662,#28663,#28664,#28665,#28666,#28667,#28668,#28669,
#28670,#28671,#28672,#28673,#28674,#28675,#28676,#28677,#28678,#28679,#28680,
#28681,#28682,#28683,#28684,#28685,#28686,#28687,#28688,#28689,#28690,#28691,
#28692,#28693,#28694,#28695,#28696,#28697,#28698,#28699,#28700,#28701,#28702,
#28703,#28704,#28705,#28706,#28707,#28708,#28709,#28710,#28711,#28712,#28713,
#28714,#28715,#28716,#28717,#28718,#28719,#28720,#28721,#28722,#28723,#28724),
 .UNSPECIFIED.,.F.,.F.,(4,3,3,3,3,3,3,3,3,3,3,3,3,3,3,3,3,3,3,3,3,3,3,3,
3,3,3,3,3,3,3,3,3,3,3,3,3,3,3,3,3,3,3,3,3,3,3,3,3,3,3,3,3,3,3,3,3,3,3,3,
4),(0.0178660642413966,0.0181417588937503,0.0186938767206654,0.0187811248524612,
0.0189688428508114,0.0194531680236473,0.0199158046998442,0.0200716214602261,
0.0205298348659482,0.0210163068304557,0.0210454834309858,0.0211744000696409,
0.0219594418566194,0.0221678060338532,0.0222771786790556,0.0227260534193597,
0.0232822856052293,0.0233799572884703,0.0238115218795811,0.0239313465931777,
0.0242624070083197,0.0243886629871502,0.0244827358978851,0.0252848636807742,
0.025488188664657,0.0255855145072998,0.0260359693196439,0.0261369038120072,
0.0264718602397466,0.0265826145543591,0.0266882931167146,0.0271831282339348,
0.0276765624138436,0.0277910717261293,0.0280872868681377,0.0282242998156046,
0.0283424610308367,0.0287313424802207,0.0287733642636607,0.028893850335544,
0.0292158645122804,0.0294452396402514,0.0297215320002951,0.0298768660914162,
0.0299966289449587,0.0305825033289074,0.0309879174841298,0.0310994075543735,
0.0316285242822441,0.0321072673250968,0.0322021861637882,0.0327550977994062,
0.03323391559953,0.0333049647732029,0.0336759265167946,0.0338000533258756,
0.0338563540779102,0.0343681678909991,0.0344077433826176,0.0353007819162081,
0.0355105219920323),.UNSPECIFIED.);
#1819=B_SPLINE_CURVE_WITH_KNOTS('',3,(#28729,#28730,#28731,#28732,#28733,
#28734,#28735,#28736,#28737,#28738),.UNSPECIFIED.,.F.,.F.,(4,2,2,2,4),(-0.811230782792507,
-0.589543564549274,-0.405568456785375,-0.225516486965526,0.),
 .UNSPECIFIED.);
#1820=B_SPLINE_CURVE_WITH_KNOTS('',3,(#28740,#28741,#28742,#28743,#28744,
#28745,#28746,#28747,#28748,#28749,#28750,#28751,#28752,#28753,#28754,#28755),
 .UNSPECIFIED.,.F.,.F.,(4,2,2,2,2,2,2,4),(-1.61608002816124,-1.45775061305033,
-1.29955710501412,-1.0636537651015,-0.825767803590715,-0.617872986250325,
-0.355668197463001,0.),.UNSPECIFIED.);
#1821=B_SPLINE_CURVE_WITH_KNOTS('',3,(#28756,#28757,#28758,#28759,#28760,
#28761,#28762,#28763,#28764,#28765,#28766,#28767,#28768,#28769,#28770,#28771),
 .UNSPECIFIED.,.F.,.F.,(4,2,2,2,2,2,2,4),(-2.43104855078003,-1.903494016152,
-1.45644570848914,-1.09062827200157,-0.723808102624913,-0.376722226195001,
-0.186648168518802,0.),.UNSPECIFIED.);
#1822=B_SPLINE_CURVE_WITH_KNOTS('',3,(#31667,#31668,#31669,#31670,#31671,
#31672,#31673,#31674,#31675,#31676,#31677,#31678,#31679,#31680,#31681,#31682),
 .UNSPECIFIED.,.F.,.F.,(4,2,2,2,2,2,2,4),(0.,0.211383895657764,0.374142667531924,
0.583513224887238,0.779876212205008,0.988270595967209,1.21322647326508,
1.38005248901974),.UNSPECIFIED.);
#1823=B_SPLINE_CURVE_WITH_KNOTS('',3,(#37466,#37467,#37468,#37469,#37470,
#37471,#37472,#37473,#37474,#37475),.UNSPECIFIED.,.F.,.F.,(4,2,2,2,4),(0.,
0.220020771446265,0.376089701153298,0.530276196623649,0.752535026745683),
 .UNSPECIFIED.);
#1824=B_SPLINE_CURVE_WITH_KNOTS('',3,(#39422,#39423,#39424,#39425,#39426,
#39427,#39428,#39429,#39430,#39431,#39432,#39433,#39434,#39435,#39436,#39437),
 .UNSPECIFIED.,.F.,.F.,(4,2,2,2,2,2,2,4),(0.,0.371355913148883,0.741064833958748,
1.0486227715232,1.30223077148216,1.57308405581568,1.73972138317415,1.89659917227108),
 .UNSPECIFIED.);
#1825=B_SPLINE_CURVE_WITH_KNOTS('',3,(#40537,#40538,#40539,#40540,#40541,
#40542,#40543,#40544,#40545,#40546,#40547,#40548,#40549,#40550),
 .UNSPECIFIED.,.F.,.F.,(4,2,2,2,2,2,4),(-0.158545503402535,-0.158223124815241,
-0.138074238874086,-0.118093212716543,-0.0984509148305753,-0.0791141254766957,
-0.0790886006090571),.UNSPECIFIED.);
#1826=B_SPLINE_CURVE_WITH_KNOTS('',3,(#40568,#40569,#40570,#40571,#40572,
#40573,#40574,#40575,#40576,#40577,#40578,#40579,#40580,#40581),
 .UNSPECIFIED.,.F.,.F.,(4,2,2,2,2,2,4),(-0.0791417248593108,-0.0791161976751982,
-0.059777648817268,-0.0401335636282681,-0.0201507193459134,-2.01783034725622E-14,
0.000322407921445618),.UNSPECIFIED.);
#1827=LINE('',#9088,#2145);
#1828=LINE('',#9138,#2146);
#1829=LINE('',#9179,#2147);
#1830=LINE('',#9257,#2148);
#1831=LINE('',#9333,#2149);
#1832=LINE('',#9411,#2150);
#1833=LINE('',#9487,#2151);
#1834=LINE('',#9563,#2152);
#1835=LINE('',#9639,#2153);
#1836=LINE('',#9717,#2154);
#1837=LINE('',#9793,#2155);
#1838=LINE('',#9871,#2156);
#1839=LINE('',#9947,#2157);
#1840=LINE('',#10023,#2158);
#1841=LINE('',#10099,#2159);
#1842=LINE('',#10177,#2160);
#1843=LINE('',#10253,#2161);
#1844=LINE('',#10331,#2162);
#1845=LINE('',#10407,#2163);
#1846=LINE('',#10483,#2164);
#1847=LINE('',#10559,#2165);
#1848=LINE('',#10637,#2166);
#1849=LINE('',#10713,#2167);
#1850=LINE('',#10777,#2168);
#1851=LINE('',#10836,#2169);
#1852=LINE('',#10839,#2170);
#1853=LINE('',#10841,#2171);
#1854=LINE('',#10847,#2172);
#1855=LINE('',#10850,#2173);
#1856=LINE('',#10912,#2174);
#1857=LINE('',#10914,#2175);
#1858=LINE('',#10917,#2176);
#1859=LINE('',#11393,#2177);
#1860=LINE('',#11399,#2178);
#1861=LINE('',#11405,#2179);
#1862=LINE('',#11408,#2180);
#1863=LINE('',#11410,#2181);
#1864=LINE('',#11413,#2182);
#1865=LINE('',#11416,#2183);
#1866=LINE('',#11418,#2184);
#1867=LINE('',#11421,#2185);
#1868=LINE('',#11423,#2186);
#1869=LINE('',#11425,#2187);
#1870=LINE('',#11443,#2188);
#1871=LINE('',#11445,#2189);
#1872=LINE('',#11447,#2190);
#1873=LINE('',#11457,#2191);
#1874=LINE('',#11459,#2192);
#1875=LINE('',#11461,#2193);
#1876=LINE('',#11471,#2194);
#1877=LINE('',#11473,#2195);
#1878=LINE('',#11475,#2196);
#1879=LINE('',#11485,#2197);
#1880=LINE('',#11487,#2198);
#1881=LINE('',#11489,#2199);
#1882=LINE('',#11499,#2200);
#1883=LINE('',#11501,#2201);
#1884=LINE('',#11503,#2202);
#1885=LINE('',#11513,#2203);
#1886=LINE('',#11515,#2204);
#1887=LINE('',#11517,#2205);
#1888=LINE('',#11609,#2206);
#1889=LINE('',#11611,#2207);
#1890=LINE('',#11613,#2208);
#1891=LINE('',#11617,#2209);
#1892=LINE('',#11618,#2210);
#1893=LINE('',#11622,#2211);
#1894=LINE('',#11624,#2212);
#1895=LINE('',#11626,#2213);
#1896=LINE('',#11628,#2214);
#1897=LINE('',#11630,#2215);
#1898=LINE('',#11635,#2216);
#1899=LINE('',#11637,#2217);
#1900=LINE('',#11640,#2218);
#1901=LINE('',#11644,#2219);
#1902=LINE('',#11650,#2220);
#1903=LINE('',#11651,#2221);
#1904=LINE('',#11652,#2222);
#1905=LINE('',#11656,#2223);
#1906=LINE('',#11661,#2224);
#1907=LINE('',#11663,#2225);
#1908=LINE('',#11664,#2226);
#1909=LINE('',#11669,#2227);
#1910=LINE('',#11673,#2228);
#1911=LINE('',#11677,#2229);
#1912=LINE('',#11682,#2230);
#1913=LINE('',#11684,#2231);
#1914=LINE('',#11686,#2232);
#1915=LINE('',#11690,#2233);
#1916=LINE('',#11691,#2234);
#1917=LINE('',#11695,#2235);
#1918=LINE('',#11697,#2236);
#1919=LINE('',#11700,#2237);
#1920=LINE('',#11704,#2238);
#1921=LINE('',#11708,#2239);
#1922=LINE('',#11709,#2240);
#1923=LINE('',#11713,#2241);
#1924=LINE('',#11717,#2242);
#1925=LINE('',#11718,#2243);
#1926=LINE('',#11723,#2244);
#1927=LINE('',#11726,#2245);
#1928=LINE('',#11728,#2246);
#1929=LINE('',#11733,#2247);
#1930=LINE('',#11734,#2248);
#1931=LINE('',#11736,#2249);
#1932=LINE('',#11740,#2250);
#1933=LINE('',#11742,#2251);
#1934=LINE('',#11745,#2252);
#1935=LINE('',#11749,#2253);
#1936=LINE('',#11750,#2254);
#1937=LINE('',#11751,#2255);
#1938=LINE('',#11755,#2256);
#1939=LINE('',#11759,#2257);
#1940=LINE('',#11760,#2258);
#1941=LINE('',#11764,#2259);
#1942=LINE('',#11768,#2260);
#1943=LINE('',#11769,#2261);
#1944=LINE('',#11777,#2262);
#1945=LINE('',#11781,#2263);
#1946=LINE('',#11785,#2264);
#1947=LINE('',#11790,#2265);
#1948=LINE('',#11792,#2266);
#1949=LINE('',#11794,#2267);
#1950=LINE('',#11796,#2268);
#1951=LINE('',#11798,#2269);
#1952=LINE('',#25553,#2270);
#1953=LINE('',#25557,#2271);
#1954=LINE('',#25561,#2272);
#1955=LINE('',#25565,#2273);
#1956=LINE('',#25569,#2274);
#1957=LINE('',#25573,#2275);
#1958=LINE('',#28166,#2276);
#1959=LINE('',#28350,#2277);
#1960=LINE('',#28354,#2278);
#1961=LINE('',#28361,#2279);
#1962=LINE('',#28367,#2280);
#1963=LINE('',#28370,#2281);
#1964=LINE('',#28461,#2282);
#1965=LINE('',#39442,#2283);
#1966=LINE('',#39444,#2284);
#1967=LINE('',#39446,#2285);
#1968=LINE('',#39452,#2286);
#1969=LINE('',#39458,#2287);
#1970=LINE('',#39460,#2288);
#1971=LINE('',#39466,#2289);
#1972=LINE('',#39472,#2290);
#1973=LINE('',#39474,#2291);
#1974=LINE('',#39480,#2292);
#1975=LINE('',#39486,#2293);
#1976=LINE('',#39488,#2294);
#1977=LINE('',#39494,#2295);
#1978=LINE('',#39500,#2296);
#1979=LINE('',#39501,#2297);
#1980=LINE('',#39503,#2298);
#1981=LINE('',#39508,#2299);
#1982=LINE('',#39513,#2300);
#1983=LINE('',#39800,#2301);
#1984=LINE('',#39806,#2302);
#1985=LINE('',#39815,#2303);
#1986=LINE('',#39820,#2304);
#1987=LINE('',#39829,#2305);
#1988=LINE('',#39834,#2306);
#1989=LINE('',#39843,#2307);
#1990=LINE('',#39848,#2308);
#1991=LINE('',#39856,#2309);
#1992=LINE('',#39862,#2310);
#1993=LINE('',#39870,#2311);
#1994=LINE('',#39874,#2312);
#1995=LINE('',#39877,#2313);
#1996=LINE('',#39879,#2314);
#1997=LINE('',#39881,#2315);
#1998=LINE('',#39883,#2316);
#1999=LINE('',#39887,#2317);
#2000=LINE('',#39897,#2318);
#2001=LINE('',#39915,#2319);
#2002=LINE('',#39930,#2320);
#2003=LINE('',#39951,#2321);
#2004=LINE('',#39969,#2322);
#2005=LINE('',#40023,#2323);
#2006=LINE('',#40037,#2324);
#2007=LINE('',#40045,#2325);
#2008=LINE('',#40050,#2326);
#2009=LINE('',#40056,#2327);
#2010=LINE('',#40063,#2328);
#2011=LINE('',#40068,#2329);
#2012=LINE('',#40074,#2330);
#2013=LINE('',#40081,#2331);
#2014=LINE('',#40086,#2332);
#2015=LINE('',#40092,#2333);
#2016=LINE('',#40099,#2334);
#2017=LINE('',#40104,#2335);
#2018=LINE('',#40110,#2336);
#2019=LINE('',#40117,#2337);
#2020=LINE('',#40122,#2338);
#2021=LINE('',#40128,#2339);
#2022=LINE('',#40135,#2340);
#2023=LINE('',#40140,#2341);
#2024=LINE('',#40146,#2342);
#2025=LINE('',#40153,#2343);
#2026=LINE('',#40158,#2344);
#2027=LINE('',#40164,#2345);
#2028=LINE('',#40171,#2346);
#2029=LINE('',#40176,#2347);
#2030=LINE('',#40182,#2348);
#2031=LINE('',#40189,#2349);
#2032=LINE('',#40194,#2350);
#2033=LINE('',#40200,#2351);
#2034=LINE('',#40207,#2352);
#2035=LINE('',#40212,#2353);
#2036=LINE('',#40218,#2354);
#2037=LINE('',#40225,#2355);
#2038=LINE('',#40230,#2356);
#2039=LINE('',#40236,#2357);
#2040=LINE('',#40243,#2358);
#2041=LINE('',#40248,#2359);
#2042=LINE('',#40254,#2360);
#2043=LINE('',#40261,#2361);
#2044=LINE('',#40266,#2362);
#2045=LINE('',#40272,#2363);
#2046=LINE('',#40279,#2364);
#2047=LINE('',#40284,#2365);
#2048=LINE('',#40290,#2366);
#2049=LINE('',#40297,#2367);
#2050=LINE('',#40302,#2368);
#2051=LINE('',#40320,#2369);
#2052=LINE('',#40328,#2370);
#2053=LINE('',#40332,#2371);
#2054=LINE('',#40333,#2372);
#2055=LINE('',#40336,#2373);
#2056=LINE('',#40337,#2374);
#2057=LINE('',#40340,#2375);
#2058=LINE('',#40341,#2376);
#2059=LINE('',#40344,#2377);
#2060=LINE('',#40345,#2378);
#2061=LINE('',#40348,#2379);
#2062=LINE('',#40349,#2380);
#2063=LINE('',#40352,#2381);
#2064=LINE('',#40353,#2382);
#2065=LINE('',#40416,#2383);
#2066=LINE('',#40417,#2384);
#2067=LINE('',#40419,#2385);
#2068=LINE('',#40421,#2386);
#2069=LINE('',#40423,#2387);
#2070=LINE('',#40425,#2388);
#2071=LINE('',#40433,#2389);
#2072=LINE('',#40440,#2390);
#2073=LINE('',#40443,#2391);
#2074=LINE('',#40448,#2392);
#2075=LINE('',#40453,#2393);
#2076=LINE('',#40455,#2394);
#2077=LINE('',#40457,#2395);
#2078=LINE('',#40458,#2396);
#2079=LINE('',#40462,#2397);
#2080=LINE('',#40463,#2398);
#2081=LINE('',#40464,#2399);
#2082=LINE('',#40467,#2400);
#2083=LINE('',#40469,#2401);
#2084=LINE('',#40470,#2402);
#2085=LINE('',#40472,#2403);
#2086=LINE('',#40473,#2404);
#2087=LINE('',#40479,#2405);
#2088=LINE('',#40482,#2406);
#2089=LINE('',#40486,#2407);
#2090=LINE('',#40487,#2408);
#2091=LINE('',#40488,#2409);
#2092=LINE('',#40491,#2410);
#2093=LINE('',#40492,#2411);
#2094=LINE('',#40495,#2412);
#2095=LINE('',#40496,#2413);
#2096=LINE('',#40498,#2414);
#2097=LINE('',#40510,#2415);
#2098=LINE('',#40517,#2416);
#2099=LINE('',#40520,#2417);
#2100=LINE('',#40522,#2418);
#2101=LINE('',#40524,#2419);
#2102=LINE('',#40525,#2420);
#2103=LINE('',#40527,#2421);
#2104=LINE('',#40529,#2422);
#2105=LINE('',#40600,#2423);
#2106=LINE('',#40606,#2424);
#2107=LINE('',#40614,#2425);
#2108=LINE('',#40620,#2426);
#2109=LINE('',#40628,#2427);
#2110=LINE('',#40634,#2428);
#2111=LINE('',#40642,#2429);
#2112=LINE('',#40648,#2430);
#2113=LINE('',#40656,#2431);
#2114=LINE('',#40662,#2432);
#2115=LINE('',#40665,#2433);
#2116=LINE('',#40667,#2434);
#2117=LINE('',#40669,#2435);
#2118=LINE('',#40671,#2436);
#2119=LINE('',#40673,#2437);
#2120=LINE('',#40679,#2438);
#2121=LINE('',#40682,#2439);
#2122=LINE('',#40688,#2440);
#2123=LINE('',#40691,#2441);
#2124=LINE('',#40694,#2442);
#2125=LINE('',#40696,#2443);
#2126=LINE('',#40699,#2444);
#2127=LINE('',#40703,#2445);
#2128=LINE('',#40707,#2446);
#2129=LINE('',#40709,#2447);
#2130=LINE('',#40713,#2448);
#2131=LINE('',#40716,#2449);
#2132=LINE('',#40719,#2450);
#2133=LINE('',#40720,#2451);
#2134=LINE('',#40721,#2452);
#2135=LINE('',#40723,#2453);
#2136=LINE('',#40728,#2454);
#2137=LINE('',#40731,#2455);
#2138=LINE('',#40732,#2456);
#2139=LINE('',#40734,#2457);
#2140=LINE('',#40735,#2458);
#2141=LINE('',#40736,#2459);
#2142=LINE('',#40738,#2460);
#2143=LINE('',#40740,#2461);
#2144=LINE('',#40741,#2462);
#2145=VECTOR('',#7191,8.326);
#2146=VECTOR('',#7194,8.326);
#2147=VECTOR('',#7199,8.326);
#2148=VECTOR('',#7202,8.326);
#2149=VECTOR('',#7205,8.326);
#2150=VECTOR('',#7208,8.326);
#2151=VECTOR('',#7211,8.326);
#2152=VECTOR('',#7214,8.326);
#2153=VECTOR('',#7217,8.326);
#2154=VECTOR('',#7220,8.326);
#2155=VECTOR('',#7223,8.326);
#2156=VECTOR('',#7226,8.326);
#2157=VECTOR('',#7229,8.326);
#2158=VECTOR('',#7232,8.326);
#2159=VECTOR('',#7235,8.326);
#2160=VECTOR('',#7238,8.326);
#2161=VECTOR('',#7241,8.326);
#2162=VECTOR('',#7244,8.326);
#2163=VECTOR('',#7247,8.326);
#2164=VECTOR('',#7250,8.326);
#2165=VECTOR('',#7253,8.326);
#2166=VECTOR('',#7256,8.326);
#2167=VECTOR('',#7259,8.326);
#2168=VECTOR('',#7296,1000.);
#2169=VECTOR('',#7299,1000.);
#2170=VECTOR('',#7302,1000.);
#2171=VECTOR('',#7305,1000.);
#2172=VECTOR('',#7310,1000.);
#2173=VECTOR('',#7313,1000.);
#2174=VECTOR('',#7318,1000.);
#2175=VECTOR('',#7321,1000.);
#2176=VECTOR('',#7324,8.326);
#2177=VECTOR('',#7353,3.2);
#2178=VECTOR('',#7360,3.2);
#2179=VECTOR('',#7367,3.2);
#2180=VECTOR('',#7372,19.05);
#2181=VECTOR('',#7373,1000.);
#2182=VECTOR('',#7376,19.05);
#2183=VECTOR('',#7379,1000.);
#2184=VECTOR('',#7380,1000.);
#2185=VECTOR('',#7383,1000.);
#2186=VECTOR('',#7384,1000.);
#2187=VECTOR('',#7385,1000.);
#2188=VECTOR('',#7404,1000.);
#2189=VECTOR('',#7405,1000.);
#2190=VECTOR('',#7406,1000.);
#2191=VECTOR('',#7409,1000.);
#2192=VECTOR('',#7410,1000.);
#2193=VECTOR('',#7411,1000.);
#2194=VECTOR('',#7414,1000.);
#2195=VECTOR('',#7415,1000.);
#2196=VECTOR('',#7416,1000.);
#2197=VECTOR('',#7419,1000.);
#2198=VECTOR('',#7420,1000.);
#2199=VECTOR('',#7421,1000.);
#2200=VECTOR('',#7424,1000.);
#2201=VECTOR('',#7425,1000.);
#2202=VECTOR('',#7426,1000.);
#2203=VECTOR('',#7429,1000.);
#2204=VECTOR('',#7430,1000.);
#2205=VECTOR('',#7431,1000.);
#2206=VECTOR('',#7440,1000.);
#2207=VECTOR('',#7441,1000.);
#2208=VECTOR('',#7442,1000.);
#2209=VECTOR('',#7445,1000.);
#2210=VECTOR('',#7446,1000.);
#2211=VECTOR('',#7449,1000.);
#2212=VECTOR('',#7450,1000.);
#2213=VECTOR('',#7451,1000.);
#2214=VECTOR('',#7452,1000.);
#2215=VECTOR('',#7453,1000.);
#2216=VECTOR('',#7458,1000.);
#2217=VECTOR('',#7459,1000.);
#2218=VECTOR('',#7462,1000.);
#2219=VECTOR('',#7465,1000.);
#2220=VECTOR('',#7472,1000.);
#2221=VECTOR('',#7473,1000.);
#2222=VECTOR('',#7474,1000.);
#2223=VECTOR('',#7477,1000.);
#2224=VECTOR('',#7484,1000.);
#2225=VECTOR('',#7485,1000.);
#2226=VECTOR('',#7486,1000.);
#2227=VECTOR('',#7491,1000.);
#2228=VECTOR('',#7494,1000.);
#2229=VECTOR('',#7497,1000.);
#2230=VECTOR('',#7502,1000.);
#2231=VECTOR('',#7503,1000.);
#2232=VECTOR('',#7504,1000.);
#2233=VECTOR('',#7507,1000.);
#2234=VECTOR('',#7508,1000.);
#2235=VECTOR('',#7511,1000.);
#2236=VECTOR('',#7512,1000.);
#2237=VECTOR('',#7515,1000.);
#2238=VECTOR('',#7520,1000.);
#2239=VECTOR('',#7525,1000.);
#2240=VECTOR('',#7526,1000.);
#2241=VECTOR('',#7531,1000.);
#2242=VECTOR('',#7536,1000.);
#2243=VECTOR('',#7537,1000.);
#2244=VECTOR('',#7542,1000.);
#2245=VECTOR('',#7545,1000.);
#2246=VECTOR('',#7546,1000.);
#2247=VECTOR('',#7551,1000.);
#2248=VECTOR('',#7552,1000.);
#2249=VECTOR('',#7553,1000.);
#2250=VECTOR('',#7558,1000.);
#2251=VECTOR('',#7559,1000.);
#2252=VECTOR('',#7562,1000.);
#2253=VECTOR('',#7565,1000.);
#2254=VECTOR('',#7566,1000.);
#2255=VECTOR('',#7567,1000.);
#2256=VECTOR('',#7572,1000.);
#2257=VECTOR('',#7577,1000.);
#2258=VECTOR('',#7578,1000.);
#2259=VECTOR('',#7583,1000.);
#2260=VECTOR('',#7588,1000.);
#2261=VECTOR('',#7589,1000.);
#2262=VECTOR('',#7596,1000.);
#2263=VECTOR('',#7599,1000.);
#2264=VECTOR('',#7602,1000.);
#2265=VECTOR('',#7607,1000.);
#2266=VECTOR('',#7608,1000.);
#2267=VECTOR('',#7609,1000.);
#2268=VECTOR('',#7610,1000.);
#2269=VECTOR('',#7611,1000.);
#2270=VECTOR('',#7648,1000.);
#2271=VECTOR('',#7651,1000.);
#2272=VECTOR('',#7654,1000.);
#2273=VECTOR('',#7657,1000.);
#2274=VECTOR('',#7660,1000.);
#2275=VECTOR('',#7663,1000.);
#2276=VECTOR('',#7940,5.);
#2277=VECTOR('',#7949,7.4375);
#2278=VECTOR('',#7954,7.4375);
#2279=VECTOR('',#7961,11.7);
#2280=VECTOR('',#7968,7.70000000000001);
#2281=VECTOR('',#7973,12.7);
#2282=VECTOR('',#7974,12.7);
#2283=VECTOR('',#7987,1000.);
#2284=VECTOR('',#7988,1000.);
#2285=VECTOR('',#7989,1000.);
#2286=VECTOR('',#7990,1000.);
#2287=VECTOR('',#7993,1000.);
#2288=VECTOR('',#7994,1000.);
#2289=VECTOR('',#7995,1000.);
#2290=VECTOR('',#7998,1000.);
#2291=VECTOR('',#7999,1000.);
#2292=VECTOR('',#8000,1000.);
#2293=VECTOR('',#8003,1000.);
#2294=VECTOR('',#8004,1000.);
#2295=VECTOR('',#8005,1000.);
#2296=VECTOR('',#8008,1000.);
#2297=VECTOR('',#8009,1000.);
#2298=VECTOR('',#8010,1000.);
#2299=VECTOR('',#8013,1000.);
#2300=VECTOR('',#8014,1000.);
#2301=VECTOR('',#8059,4.975);
#2302=VECTOR('',#8066,2.5527);
#2303=VECTOR('',#8077,3.175);
#2304=VECTOR('',#8082,2.5527);
#2305=VECTOR('',#8093,3.175);
#2306=VECTOR('',#8098,2.5527);
#2307=VECTOR('',#8109,3.175);
#2308=VECTOR('',#8114,2.5527);
#2309=VECTOR('',#8123,3.175);
#2310=VECTOR('',#8130,3.175);
#2311=VECTOR('',#8139,3.175);
#2312=VECTOR('',#8144,2.49047);
#2313=VECTOR('',#8149,2.5527);
#2314=VECTOR('',#8152,2.5527);
#2315=VECTOR('',#8155,2.5527);
#2316=VECTOR('',#8158,2.5527);
#2317=VECTOR('',#8161,1000.);
#2318=VECTOR('',#8162,1000.);
#2319=VECTOR('',#8165,1000.);
#2320=VECTOR('',#8168,1000.);
#2321=VECTOR('',#8171,1000.);
#2322=VECTOR('',#8174,1000.);
#2323=VECTOR('',#8235,3.302);
#2324=VECTOR('',#8254,2.41935);
#2325=VECTOR('',#8263,2.41935);
#2326=VECTOR('',#8270,3.175);
#2327=VECTOR('',#8277,3.175);
#2328=VECTOR('',#8284,2.41935);
#2329=VECTOR('',#8291,3.175);
#2330=VECTOR('',#8298,3.175);
#2331=VECTOR('',#8305,2.41935);
#2332=VECTOR('',#8312,3.175);
#2333=VECTOR('',#8319,3.175);
#2334=VECTOR('',#8326,2.41935);
#2335=VECTOR('',#8333,3.175);
#2336=VECTOR('',#8340,3.175);
#2337=VECTOR('',#8347,2.41935);
#2338=VECTOR('',#8354,3.175);
#2339=VECTOR('',#8361,3.175);
#2340=VECTOR('',#8368,2.41935);
#2341=VECTOR('',#8375,3.175);
#2342=VECTOR('',#8382,3.175);
#2343=VECTOR('',#8389,2.41935);
#2344=VECTOR('',#8396,3.175);
#2345=VECTOR('',#8403,3.175);
#2346=VECTOR('',#8410,2.41935);
#2347=VECTOR('',#8417,3.175);
#2348=VECTOR('',#8424,3.175);
#2349=VECTOR('',#8431,2.41935);
#2350=VECTOR('',#8438,3.175);
#2351=VECTOR('',#8445,3.175);
#2352=VECTOR('',#8452,2.41935);
#2353=VECTOR('',#8459,3.175);
#2354=VECTOR('',#8466,3.175);
#2355=VECTOR('',#8473,2.41935);
#2356=VECTOR('',#8480,3.175);
#2357=VECTOR('',#8487,3.175);
#2358=VECTOR('',#8494,2.41935);
#2359=VECTOR('',#8501,3.175);
#2360=VECTOR('',#8508,3.175);
#2361=VECTOR('',#8515,2.41935);
#2362=VECTOR('',#8522,3.175);
#2363=VECTOR('',#8529,3.175);
#2364=VECTOR('',#8536,2.41935);
#2365=VECTOR('',#8543,3.175);
#2366=VECTOR('',#8550,3.175);
#2367=VECTOR('',#8557,2.41935);
#2368=VECTOR('',#8564,3.175);
#2369=VECTOR('',#8583,5.5626);
#2370=VECTOR('',#8594,3.175);
#2371=VECTOR('',#8599,1000.);
#2372=VECTOR('',#8600,1000.);
#2373=VECTOR('',#8603,1000.);
#2374=VECTOR('',#8604,1000.);
#2375=VECTOR('',#8607,1000.);
#2376=VECTOR('',#8608,1000.);
#2377=VECTOR('',#8611,1000.);
#2378=VECTOR('',#8612,1000.);
#2379=VECTOR('',#8615,1000.);
#2380=VECTOR('',#8616,1000.);
#2381=VECTOR('',#8619,1000.);
#2382=VECTOR('',#8620,1000.);
#2383=VECTOR('',#8649,1000.);
#2384=VECTOR('',#8650,1000.);
#2385=VECTOR('',#8653,1000.);
#2386=VECTOR('',#8656,1000.);
#2387=VECTOR('',#8659,1000.);
#2388=VECTOR('',#8662,1000.);
#2389=VECTOR('',#8673,3.175);
#2390=VECTOR('',#8680,1000.);
#2391=VECTOR('',#8683,1000.);
#2392=VECTOR('',#8688,3.175);
#2393=VECTOR('',#8693,1000.);
#2394=VECTOR('',#8694,1000.);
#2395=VECTOR('',#8695,1000.);
#2396=VECTOR('',#8696,1000.);
#2397=VECTOR('',#8699,1000.);
#2398=VECTOR('',#8700,1000.);
#2399=VECTOR('',#8701,1000.);
#2400=VECTOR('',#8704,1000.);
#2401=VECTOR('',#8705,1000.);
#2402=VECTOR('',#8706,1000.);
#2403=VECTOR('',#8709,1000.);
#2404=VECTOR('',#8710,1000.);
#2405=VECTOR('',#8715,1000.);
#2406=VECTOR('',#8718,1000.);
#2407=VECTOR('',#8721,1000.);
#2408=VECTOR('',#8722,1000.);
#2409=VECTOR('',#8723,1000.);
#2410=VECTOR('',#8726,1000.);
#2411=VECTOR('',#8727,1000.);
#2412=VECTOR('',#8730,1000.);
#2413=VECTOR('',#8731,1000.);
#2414=VECTOR('',#8734,1000.);
#2415=VECTOR('',#8753,1000.);
#2416=VECTOR('',#8762,1000.);
#2417=VECTOR('',#8767,1000.);
#2418=VECTOR('',#8770,1000.);
#2419=VECTOR('',#8773,1000.);
#2420=VECTOR('',#8774,1000.);
#2421=VECTOR('',#8777,1000.);
#2422=VECTOR('',#8780,1000.);
#2423=VECTOR('',#8827,3.5);
#2424=VECTOR('',#8834,3.99999999999998);
#2425=VECTOR('',#8843,3.5);
#2426=VECTOR('',#8850,4.);
#2427=VECTOR('',#8859,3.5);
#2428=VECTOR('',#8866,4.);
#2429=VECTOR('',#8875,3.49999999999999);
#2430=VECTOR('',#8882,4.);
#2431=VECTOR('',#8891,3.49999999999999);
#2432=VECTOR('',#8898,3.99999999999998);
#2433=VECTOR('',#8903,3.49999999999999);
#2434=VECTOR('',#8906,3.49999999999999);
#2435=VECTOR('',#8909,3.5);
#2436=VECTOR('',#8912,3.5);
#2437=VECTOR('',#8915,3.5);
#2438=VECTOR('',#8920,1000.);
#2439=VECTOR('',#8923,1000.);
#2440=VECTOR('',#8928,1000.);
#2441=VECTOR('',#8931,1000.);
#2442=VECTOR('',#8934,1000.);
#2443=VECTOR('',#8935,1000.);
#2444=VECTOR('',#8938,1000.);
#2445=VECTOR('',#8941,1000.);
#2446=VECTOR('',#8946,1000.);
#2447=VECTOR('',#8947,1000.);
#2448=VECTOR('',#8950,1000.);
#2449=VECTOR('',#8953,1000.);
#2450=VECTOR('',#8958,1000.);
#2451=VECTOR('',#8959,1000.);
#2452=VECTOR('',#8960,1000.);
#2453=VECTOR('',#8963,1000.);
#2454=VECTOR('',#8968,1000.);
#2455=VECTOR('',#8973,1000.);
#2456=VECTOR('',#8974,1000.);
#2457=VECTOR('',#8977,1000.);
#2458=VECTOR('',#8978,1000.);
#2459=VECTOR('',#8979,1000.);
#2460=VECTOR('',#8982,1000.);
#2461=VECTOR('',#8985,1000.);
#2462=VECTOR('',#8986,1000.);
#2463=VERTEX_POINT('',#9086);
#2464=VERTEX_POINT('',#9087);
#2465=VERTEX_POINT('',#9089);
#2466=VERTEX_POINT('',#9126);
#2467=VERTEX_POINT('',#9128);
#2468=VERTEX_POINT('',#9137);
#2469=VERTEX_POINT('',#9177);
#2470=VERTEX_POINT('',#9178);
#2471=VERTEX_POINT('',#9255);
#2472=VERTEX_POINT('',#9256);
#2473=VERTEX_POINT('',#9331);
#2474=VERTEX_POINT('',#9332);
#2475=VERTEX_POINT('',#9409);
#2476=VERTEX_POINT('',#9410);
#2477=VERTEX_POINT('',#9485);
#2478=VERTEX_POINT('',#9486);
#2479=VERTEX_POINT('',#9561);
#2480=VERTEX_POINT('',#9562);
#2481=VERTEX_POINT('',#9637);
#2482=VERTEX_POINT('',#9638);
#2483=VERTEX_POINT('',#9715);
#2484=VERTEX_POINT('',#9716);
#2485=VERTEX_POINT('',#9791);
#2486=VERTEX_POINT('',#9792);
#2487=VERTEX_POINT('',#9869);
#2488=VERTEX_POINT('',#9870);
#2489=VERTEX_POINT('',#9945);
#2490=VERTEX_POINT('',#9946);
#2491=VERTEX_POINT('',#10021);
#2492=VERTEX_POINT('',#10022);
#2493=VERTEX_POINT('',#10097);
#2494=VERTEX_POINT('',#10098);
#2495=VERTEX_POINT('',#10175);
#2496=VERTEX_POINT('',#10176);
#2497=VERTEX_POINT('',#10251);
#2498=VERTEX_POINT('',#10252);
#2499=VERTEX_POINT('',#10329);
#2500=VERTEX_POINT('',#10330);
#2501=VERTEX_POINT('',#10405);
#2502=VERTEX_POINT('',#10406);
#2503=VERTEX_POINT('',#10481);
#2504=VERTEX_POINT('',#10482);
#2505=VERTEX_POINT('',#10557);
#2506=VERTEX_POINT('',#10558);
#2507=VERTEX_POINT('',#10635);
#2508=VERTEX_POINT('',#10636);
#2509=VERTEX_POINT('',#10711);
#2510=VERTEX_POINT('',#10712);
#2511=VERTEX_POINT('',#10714);
#2512=VERTEX_POINT('',#10727);
#2513=VERTEX_POINT('',#10748);
#2514=VERTEX_POINT('',#10749);
#2515=VERTEX_POINT('',#10752);
#2516=VERTEX_POINT('',#10756);
#2517=VERTEX_POINT('',#10758);
#2518=VERTEX_POINT('',#10760);
#2519=VERTEX_POINT('',#10764);
#2520=VERTEX_POINT('',#10765);
#2521=VERTEX_POINT('',#10767);
#2522=VERTEX_POINT('',#10769);
#2523=VERTEX_POINT('',#10773);
#2524=VERTEX_POINT('',#10774);
#2525=VERTEX_POINT('',#10776);
#2526=VERTEX_POINT('',#10778);
#2527=VERTEX_POINT('',#10780);
#2528=VERTEX_POINT('',#10838);
#2529=VERTEX_POINT('',#10843);
#2530=VERTEX_POINT('',#10844);
#2531=VERTEX_POINT('',#10846);
#2532=VERTEX_POINT('',#10848);
#2533=VERTEX_POINT('',#10852);
#2534=VERTEX_POINT('',#10853);
#2535=VERTEX_POINT('',#10909);
#2536=VERTEX_POINT('',#10911);
#2537=VERTEX_POINT('',#10916);
#2538=VERTEX_POINT('',#10920);
#2539=VERTEX_POINT('',#10921);
#2540=VERTEX_POINT('',#10968);
#2541=VERTEX_POINT('',#11021);
#2542=VERTEX_POINT('',#11023);
#2543=VERTEX_POINT('',#11115);
#2544=VERTEX_POINT('',#11123);
#2545=VERTEX_POINT('',#11133);
#2546=VERTEX_POINT('',#11134);
#2547=VERTEX_POINT('',#11136);
#2548=VERTEX_POINT('',#11177);
#2549=VERTEX_POINT('',#11179);
#2550=VERTEX_POINT('',#11225);
#2551=VERTEX_POINT('',#11226);
#2552=VERTEX_POINT('',#11228);
#2553=VERTEX_POINT('',#11269);
#2554=VERTEX_POINT('',#11390);
#2555=VERTEX_POINT('',#11392);
#2556=VERTEX_POINT('',#11396);
#2557=VERTEX_POINT('',#11398);
#2558=VERTEX_POINT('',#11402);
#2559=VERTEX_POINT('',#11404);
#2560=VERTEX_POINT('',#11409);
#2561=VERTEX_POINT('',#11411);
#2562=VERTEX_POINT('',#11414);
#2563=VERTEX_POINT('',#11417);
#2564=VERTEX_POINT('',#11419);
#2565=VERTEX_POINT('',#11422);
#2566=VERTEX_POINT('',#11424);
#2567=VERTEX_POINT('',#11428);
#2568=VERTEX_POINT('',#11429);
#2569=VERTEX_POINT('',#11431);
#2570=VERTEX_POINT('',#11433);
#2571=VERTEX_POINT('',#11435);
#2572=VERTEX_POINT('',#11437);
#2573=VERTEX_POINT('',#11441);
#2574=VERTEX_POINT('',#11442);
#2575=VERTEX_POINT('',#11444);
#2576=VERTEX_POINT('',#11446);
#2577=VERTEX_POINT('',#11455);
#2578=VERTEX_POINT('',#11456);
#2579=VERTEX_POINT('',#11458);
#2580=VERTEX_POINT('',#11460);
#2581=VERTEX_POINT('',#11469);
#2582=VERTEX_POINT('',#11470);
#2583=VERTEX_POINT('',#11472);
#2584=VERTEX_POINT('',#11474);
#2585=VERTEX_POINT('',#11483);
#2586=VERTEX_POINT('',#11484);
#2587=VERTEX_POINT('',#11486);
#2588=VERTEX_POINT('',#11488);
#2589=VERTEX_POINT('',#11497);
#2590=VERTEX_POINT('',#11498);
#2591=VERTEX_POINT('',#11500);
#2592=VERTEX_POINT('',#11502);
#2593=VERTEX_POINT('',#11511);
#2594=VERTEX_POINT('',#11512);
#2595=VERTEX_POINT('',#11514);
#2596=VERTEX_POINT('',#11516);
#2597=VERTEX_POINT('',#11525);
#2598=VERTEX_POINT('',#11526);
#2599=VERTEX_POINT('',#11541);
#2600=VERTEX_POINT('',#11558);
#2601=VERTEX_POINT('',#11583);
#2602=VERTEX_POINT('',#11607);
#2603=VERTEX_POINT('',#11608);
#2604=VERTEX_POINT('',#11610);
#2605=VERTEX_POINT('',#11612);
#2606=VERTEX_POINT('',#11614);
#2607=VERTEX_POINT('',#11616);
#2608=VERTEX_POINT('',#11620);
#2609=VERTEX_POINT('',#11621);
#2610=VERTEX_POINT('',#11623);
#2611=VERTEX_POINT('',#11625);
#2612=VERTEX_POINT('',#11627);
#2613=VERTEX_POINT('',#11629);
#2614=VERTEX_POINT('',#11633);
#2615=VERTEX_POINT('',#11634);
#2616=VERTEX_POINT('',#11636);
#2617=VERTEX_POINT('',#11638);
#2618=VERTEX_POINT('',#11642);
#2619=VERTEX_POINT('',#11643);
#2620=VERTEX_POINT('',#11648);
#2621=VERTEX_POINT('',#11649);
#2622=VERTEX_POINT('',#11654);
#2623=VERTEX_POINT('',#11655);
#2624=VERTEX_POINT('',#11660);
#2625=VERTEX_POINT('',#11662);
#2626=VERTEX_POINT('',#11666);
#2627=VERTEX_POINT('',#11668);
#2628=VERTEX_POINT('',#11670);
#2629=VERTEX_POINT('',#11672);
#2630=VERTEX_POINT('',#11674);
#2631=VERTEX_POINT('',#11676);
#2632=VERTEX_POINT('',#11680);
#2633=VERTEX_POINT('',#11681);
#2634=VERTEX_POINT('',#11683);
#2635=VERTEX_POINT('',#11685);
#2636=VERTEX_POINT('',#11687);
#2637=VERTEX_POINT('',#11689);
#2638=VERTEX_POINT('',#11693);
#2639=VERTEX_POINT('',#11694);
#2640=VERTEX_POINT('',#11696);
#2641=VERTEX_POINT('',#11698);
#2642=VERTEX_POINT('',#11703);
#2643=VERTEX_POINT('',#11707);
#2644=VERTEX_POINT('',#11712);
#2645=VERTEX_POINT('',#11716);
#2646=VERTEX_POINT('',#11720);
#2647=VERTEX_POINT('',#11722);
#2648=VERTEX_POINT('',#11724);
#2649=VERTEX_POINT('',#11727);
#2650=VERTEX_POINT('',#11731);
#2651=VERTEX_POINT('',#11732);
#2652=VERTEX_POINT('',#11735);
#2653=VERTEX_POINT('',#11739);
#2654=VERTEX_POINT('',#11741);
#2655=VERTEX_POINT('',#11743);
#2656=VERTEX_POINT('',#11747);
#2657=VERTEX_POINT('',#11748);
#2658=VERTEX_POINT('',#11753);
#2659=VERTEX_POINT('',#11758);
#2660=VERTEX_POINT('',#11762);
#2661=VERTEX_POINT('',#11767);
#2662=VERTEX_POINT('',#11771);
#2663=VERTEX_POINT('',#11772);
#2664=VERTEX_POINT('',#11774);
#2665=VERTEX_POINT('',#11776);
#2666=VERTEX_POINT('',#11778);
#2667=VERTEX_POINT('',#11780);
#2668=VERTEX_POINT('',#11782);
#2669=VERTEX_POINT('',#11784);
#2670=VERTEX_POINT('',#11788);
#2671=VERTEX_POINT('',#11789);
#2672=VERTEX_POINT('',#11791);
#2673=VERTEX_POINT('',#11793);
#2674=VERTEX_POINT('',#11795);
#2675=VERTEX_POINT('',#11797);
#2676=VERTEX_POINT('',#11801);
#2677=VERTEX_POINT('',#11923);
#2678=VERTEX_POINT('',#12042);
#2679=VERTEX_POINT('',#12164);
#2680=VERTEX_POINT('',#12283);
#2681=VERTEX_POINT('',#12405);
#2682=VERTEX_POINT('',#12608);
#2683=VERTEX_POINT('',#12707);
#2684=VERTEX_POINT('',#12807);
#2685=VERTEX_POINT('',#12906);
#2686=VERTEX_POINT('',#13006);
#2687=VERTEX_POINT('',#13013);
#2688=VERTEX_POINT('',#13030);
#2689=VERTEX_POINT('',#25551);
#2690=VERTEX_POINT('',#25552);
#2691=VERTEX_POINT('',#25554);
#2692=VERTEX_POINT('',#25556);
#2693=VERTEX_POINT('',#25558);
#2694=VERTEX_POINT('',#25560);
#2695=VERTEX_POINT('',#25562);
#2696=VERTEX_POINT('',#25564);
#2697=VERTEX_POINT('',#25566);
#2698=VERTEX_POINT('',#25568);
#2699=VERTEX_POINT('',#25570);
#2700=VERTEX_POINT('',#25572);
#2701=VERTEX_POINT('',#27292);
#2702=VERTEX_POINT('',#27293);
#2703=VERTEX_POINT('',#27466);
#2704=VERTEX_POINT('',#27468);
#2705=VERTEX_POINT('',#27551);
#2706=VERTEX_POINT('',#27572);
#2707=VERTEX_POINT('',#27704);
#2708=VERTEX_POINT('',#27705);
#2709=VERTEX_POINT('',#27791);
#2710=VERTEX_POINT('',#27793);
#2711=VERTEX_POINT('',#27987);
#2712=VERTEX_POINT('',#27989);
#2713=VERTEX_POINT('',#28077);
#2714=VERTEX_POINT('',#28078);
#2715=VERTEX_POINT('',#28080);
#2716=VERTEX_POINT('',#28088);
#2717=VERTEX_POINT('',#28165);
#2718=VERTEX_POINT('',#28345);
#2719=VERTEX_POINT('',#28346);
#2720=VERTEX_POINT('',#28349);
#2721=VERTEX_POINT('',#28353);
#2722=VERTEX_POINT('',#28356);
#2723=VERTEX_POINT('',#28357);
#2724=VERTEX_POINT('',#28360);
#2725=VERTEX_POINT('',#28364);
#2726=VERTEX_POINT('',#28366);
#2727=VERTEX_POINT('',#28371);
#2728=VERTEX_POINT('',#28460);
#2729=VERTEX_POINT('',#28542);
#2730=VERTEX_POINT('',#28727);
#2731=VERTEX_POINT('',#28728);
#2732=VERTEX_POINT('',#28739);
#2733=VERTEX_POINT('',#30718);
#2734=VERTEX_POINT('',#31666);
#2735=VERTEX_POINT('',#36520);
#2736=VERTEX_POINT('',#39440);
#2737=VERTEX_POINT('',#39441);
#2738=VERTEX_POINT('',#39443);
#2739=VERTEX_POINT('',#39445);
#2740=VERTEX_POINT('',#39447);
#2741=VERTEX_POINT('',#39451);
#2742=VERTEX_POINT('',#39457);
#2743=VERTEX_POINT('',#39459);
#2744=VERTEX_POINT('',#39461);
#2745=VERTEX_POINT('',#39465);
#2746=VERTEX_POINT('',#39471);
#2747=VERTEX_POINT('',#39473);
#2748=VERTEX_POINT('',#39475);
#2749=VERTEX_POINT('',#39479);
#2750=VERTEX_POINT('',#39485);
#2751=VERTEX_POINT('',#39487);
#2752=VERTEX_POINT('',#39489);
#2753=VERTEX_POINT('',#39493);
#2754=VERTEX_POINT('',#39499);
#2755=VERTEX_POINT('',#39502);
#2756=VERTEX_POINT('',#39509);
#2757=VERTEX_POINT('',#39786);
#2758=VERTEX_POINT('',#39787);
#2759=VERTEX_POINT('',#39789);
#2760=VERTEX_POINT('',#39793);
#2761=VERTEX_POINT('',#39794);
#2762=VERTEX_POINT('',#39796);
#2763=VERTEX_POINT('',#39803);
#2764=VERTEX_POINT('',#39805);
#2765=VERTEX_POINT('',#39807);
#2766=VERTEX_POINT('',#39811);
#2767=VERTEX_POINT('',#39812);
#2768=VERTEX_POINT('',#39817);
#2769=VERTEX_POINT('',#39819);
#2770=VERTEX_POINT('',#39821);
#2771=VERTEX_POINT('',#39825);
#2772=VERTEX_POINT('',#39826);
#2773=VERTEX_POINT('',#39831);
#2774=VERTEX_POINT('',#39833);
#2775=VERTEX_POINT('',#39835);
#2776=VERTEX_POINT('',#39839);
#2777=VERTEX_POINT('',#39840);
#2778=VERTEX_POINT('',#39845);
#2779=VERTEX_POINT('',#39847);
#2780=VERTEX_POINT('',#39849);
#2781=VERTEX_POINT('',#39853);
#2782=VERTEX_POINT('',#39854);
#2783=VERTEX_POINT('',#39859);
#2784=VERTEX_POINT('',#39861);
#2785=VERTEX_POINT('',#39863);
#2786=VERTEX_POINT('',#39867);
#2787=VERTEX_POINT('',#39868);
#2788=VERTEX_POINT('',#39873);
#2789=VERTEX_POINT('',#39885);
#2790=VERTEX_POINT('',#39886);
#2791=VERTEX_POINT('',#39888);
#2792=VERTEX_POINT('',#39892);
#2793=VERTEX_POINT('',#39896);
#2794=VERTEX_POINT('',#39898);
#2795=VERTEX_POINT('',#39906);
#2796=VERTEX_POINT('',#39910);
#2797=VERTEX_POINT('',#39914);
#2798=VERTEX_POINT('',#39916);
#2799=VERTEX_POINT('',#39924);
#2800=VERTEX_POINT('',#39925);
#2801=VERTEX_POINT('',#39929);
#2802=VERTEX_POINT('',#39931);
#2803=VERTEX_POINT('',#39942);
#2804=VERTEX_POINT('',#39946);
#2805=VERTEX_POINT('',#39950);
#2806=VERTEX_POINT('',#39952);
#2807=VERTEX_POINT('',#39960);
#2808=VERTEX_POINT('',#39964);
#2809=VERTEX_POINT('',#39968);
#2810=VERTEX_POINT('',#39970);
#2811=VERTEX_POINT('',#39978);
#2812=VERTEX_POINT('',#39985);
#2813=VERTEX_POINT('',#40020);
#2814=VERTEX_POINT('',#40022);
#2815=VERTEX_POINT('',#40026);
#2816=VERTEX_POINT('',#40032);
#2817=VERTEX_POINT('',#40033);
#2818=VERTEX_POINT('',#40036);
#2819=VERTEX_POINT('',#40040);
#2820=VERTEX_POINT('',#40041);
#2821=VERTEX_POINT('',#40044);
#2822=VERTEX_POINT('',#40046);
#2823=VERTEX_POINT('',#40052);
#2824=VERTEX_POINT('',#40053);
#2825=VERTEX_POINT('',#40058);
#2826=VERTEX_POINT('',#40059);
#2827=VERTEX_POINT('',#40062);
#2828=VERTEX_POINT('',#40064);
#2829=VERTEX_POINT('',#40070);
#2830=VERTEX_POINT('',#40071);
#2831=VERTEX_POINT('',#40076);
#2832=VERTEX_POINT('',#40077);
#2833=VERTEX_POINT('',#40080);
#2834=VERTEX_POINT('',#40082);
#2835=VERTEX_POINT('',#40088);
#2836=VERTEX_POINT('',#40089);
#2837=VERTEX_POINT('',#40094);
#2838=VERTEX_POINT('',#40095);
#2839=VERTEX_POINT('',#40098);
#2840=VERTEX_POINT('',#40100);
#2841=VERTEX_POINT('',#40106);
#2842=VERTEX_POINT('',#40107);
#2843=VERTEX_POINT('',#40112);
#2844=VERTEX_POINT('',#40113);
#2845=VERTEX_POINT('',#40116);
#2846=VERTEX_POINT('',#40118);
#2847=VERTEX_POINT('',#40124);
#2848=VERTEX_POINT('',#40125);
#2849=VERTEX_POINT('',#40130);
#2850=VERTEX_POINT('',#40131);
#2851=VERTEX_POINT('',#40134);
#2852=VERTEX_POINT('',#40136);
#2853=VERTEX_POINT('',#40142);
#2854=VERTEX_POINT('',#40143);
#2855=VERTEX_POINT('',#40148);
#2856=VERTEX_POINT('',#40149);
#2857=VERTEX_POINT('',#40152);
#2858=VERTEX_POINT('',#40154);
#2859=VERTEX_POINT('',#40160);
#2860=VERTEX_POINT('',#40161);
#2861=VERTEX_POINT('',#40166);
#2862=VERTEX_POINT('',#40167);
#2863=VERTEX_POINT('',#40170);
#2864=VERTEX_POINT('',#40172);
#2865=VERTEX_POINT('',#40178);
#2866=VERTEX_POINT('',#40179);
#2867=VERTEX_POINT('',#40184);
#2868=VERTEX_POINT('',#40185);
#2869=VERTEX_POINT('',#40188);
#2870=VERTEX_POINT('',#40190);
#2871=VERTEX_POINT('',#40196);
#2872=VERTEX_POINT('',#40197);
#2873=VERTEX_POINT('',#40202);
#2874=VERTEX_POINT('',#40203);
#2875=VERTEX_POINT('',#40206);
#2876=VERTEX_POINT('',#40208);
#2877=VERTEX_POINT('',#40214);
#2878=VERTEX_POINT('',#40215);
#2879=VERTEX_POINT('',#40220);
#2880=VERTEX_POINT('',#40221);
#2881=VERTEX_POINT('',#40224);
#2882=VERTEX_POINT('',#40226);
#2883=VERTEX_POINT('',#40232);
#2884=VERTEX_POINT('',#40233);
#2885=VERTEX_POINT('',#40238);
#2886=VERTEX_POINT('',#40239);
#2887=VERTEX_POINT('',#40242);
#2888=VERTEX_POINT('',#40244);
#2889=VERTEX_POINT('',#40250);
#2890=VERTEX_POINT('',#40251);
#2891=VERTEX_POINT('',#40256);
#2892=VERTEX_POINT('',#40257);
#2893=VERTEX_POINT('',#40260);
#2894=VERTEX_POINT('',#40262);
#2895=VERTEX_POINT('',#40268);
#2896=VERTEX_POINT('',#40269);
#2897=VERTEX_POINT('',#40274);
#2898=VERTEX_POINT('',#40275);
#2899=VERTEX_POINT('',#40278);
#2900=VERTEX_POINT('',#40280);
#2901=VERTEX_POINT('',#40286);
#2902=VERTEX_POINT('',#40287);
#2903=VERTEX_POINT('',#40292);
#2904=VERTEX_POINT('',#40293);
#2905=VERTEX_POINT('',#40296);
#2906=VERTEX_POINT('',#40298);
#2907=VERTEX_POINT('',#40304);
#2908=VERTEX_POINT('',#40305);
#2909=VERTEX_POINT('',#40308);
#2910=VERTEX_POINT('',#40312);
#2911=VERTEX_POINT('',#40313);
#2912=VERTEX_POINT('',#40315);
#2913=VERTEX_POINT('',#40317);
#2914=VERTEX_POINT('',#40319);
#2915=VERTEX_POINT('',#40322);
#2916=VERTEX_POINT('',#40324);
#2917=VERTEX_POINT('',#40331);
#2918=VERTEX_POINT('',#40335);
#2919=VERTEX_POINT('',#40339);
#2920=VERTEX_POINT('',#40343);
#2921=VERTEX_POINT('',#40347);
#2922=VERTEX_POINT('',#40351);
#2923=VERTEX_POINT('',#40355);
#2924=VERTEX_POINT('',#40356);
#2925=VERTEX_POINT('',#40358);
#2926=VERTEX_POINT('',#40360);
#2927=VERTEX_POINT('',#40362);
#2928=VERTEX_POINT('',#40364);
#2929=VERTEX_POINT('',#40368);
#2930=VERTEX_POINT('',#40376);
#2931=VERTEX_POINT('',#40384);
#2932=VERTEX_POINT('',#40392);
#2933=VERTEX_POINT('',#40400);
#2934=VERTEX_POINT('',#40408);
#2935=VERTEX_POINT('',#40430);
#2936=VERTEX_POINT('',#40432);
#2937=VERTEX_POINT('',#40436);
#2938=VERTEX_POINT('',#40437);
#2939=VERTEX_POINT('',#40439);
#2940=VERTEX_POINT('',#40441);
#2941=VERTEX_POINT('',#40445);
#2942=VERTEX_POINT('',#40447);
#2943=VERTEX_POINT('',#40451);
#2944=VERTEX_POINT('',#40452);
#2945=VERTEX_POINT('',#40454);
#2946=VERTEX_POINT('',#40456);
#2947=VERTEX_POINT('',#40460);
#2948=VERTEX_POINT('',#40461);
#2949=VERTEX_POINT('',#40466);
#2950=VERTEX_POINT('',#40468);
#2951=VERTEX_POINT('',#40475);
#2952=VERTEX_POINT('',#40476);
#2953=VERTEX_POINT('',#40478);
#2954=VERTEX_POINT('',#40480);
#2955=VERTEX_POINT('',#40484);
#2956=VERTEX_POINT('',#40485);
#2957=VERTEX_POINT('',#40490);
#2958=VERTEX_POINT('',#40494);
#2959=VERTEX_POINT('',#40508);
#2960=VERTEX_POINT('',#40509);
#2961=VERTEX_POINT('',#40514);
#2962=VERTEX_POINT('',#40516);
#2963=VERTEX_POINT('',#40533);
#2964=VERTEX_POINT('',#40534);
#2965=VERTEX_POINT('',#40536);
#2966=VERTEX_POINT('',#40551);
#2967=VERTEX_POINT('',#40555);
#2968=VERTEX_POINT('',#40556);
#2969=VERTEX_POINT('',#40558);
#2970=VERTEX_POINT('',#40560);
#2971=VERTEX_POINT('',#40564);
#2972=VERTEX_POINT('',#40565);
#2973=VERTEX_POINT('',#40567);
#2974=VERTEX_POINT('',#40582);
#2975=VERTEX_POINT('',#40586);
#2976=VERTEX_POINT('',#40587);
#2977=VERTEX_POINT('',#40589);
#2978=VERTEX_POINT('',#40591);
#2979=VERTEX_POINT('',#40595);
#2980=VERTEX_POINT('',#40596);
#2981=VERTEX_POINT('',#40599);
#2982=VERTEX_POINT('',#40603);
#2983=VERTEX_POINT('',#40605);
#2984=VERTEX_POINT('',#40609);
#2985=VERTEX_POINT('',#40610);
#2986=VERTEX_POINT('',#40613);
#2987=VERTEX_POINT('',#40617);
#2988=VERTEX_POINT('',#40619);
#2989=VERTEX_POINT('',#40623);
#2990=VERTEX_POINT('',#40624);
#2991=VERTEX_POINT('',#40627);
#2992=VERTEX_POINT('',#40631);
#2993=VERTEX_POINT('',#40633);
#2994=VERTEX_POINT('',#40637);
#2995=VERTEX_POINT('',#40638);
#2996=VERTEX_POINT('',#40641);
#2997=VERTEX_POINT('',#40645);
#2998=VERTEX_POINT('',#40647);
#2999=VERTEX_POINT('',#40651);
#3000=VERTEX_POINT('',#40652);
#3001=VERTEX_POINT('',#40655);
#3002=VERTEX_POINT('',#40659);
#3003=VERTEX_POINT('',#40661);
#3004=VERTEX_POINT('',#40675);
#3005=VERTEX_POINT('',#40676);
#3006=VERTEX_POINT('',#40678);
#3007=VERTEX_POINT('',#40680);
#3008=VERTEX_POINT('',#40684);
#3009=VERTEX_POINT('',#40685);
#3010=VERTEX_POINT('',#40687);
#3011=VERTEX_POINT('',#40689);
#3012=VERTEX_POINT('',#40693);
#3013=VERTEX_POINT('',#40695);
#3014=VERTEX_POINT('',#40697);
#3015=VERTEX_POINT('',#40700);
#3016=VERTEX_POINT('',#40702);
#3017=VERTEX_POINT('',#40706);
#3018=VERTEX_POINT('',#40708);
#3019=VERTEX_POINT('',#40710);
#3020=VERTEX_POINT('',#40712);
#3021=VERTEX_POINT('',#40715);
#3022=VERTEX_POINT('',#40725);
#3023=VERTEX_POINT('',#40727);
#3024=EDGE_CURVE('',#2463,#2464,#1827,.T.);
#3025=EDGE_CURVE('',#2464,#2465,#1700,.T.);
#3026=EDGE_CURVE('',#2466,#2465,#1300,.T.);
#3027=EDGE_CURVE('',#2466,#2467,#1701,.T.);
#3028=EDGE_CURVE('',#2467,#2468,#1828,.T.);
#3029=EDGE_CURVE('',#2468,#2468,#1301,.T.);
#3030=EDGE_CURVE('',#2467,#2463,#1702,.T.);
#3031=EDGE_CURVE('',#2469,#2470,#1829,.T.);
#3032=EDGE_CURVE('',#2470,#2464,#1703,.T.);
#3033=EDGE_CURVE('',#2463,#2469,#1704,.T.);
#3034=EDGE_CURVE('',#2471,#2472,#1830,.T.);
#3035=EDGE_CURVE('',#2472,#2470,#1705,.T.);
#3036=EDGE_CURVE('',#2469,#2471,#1706,.T.);
#3037=EDGE_CURVE('',#2473,#2474,#1831,.T.);
#3038=EDGE_CURVE('',#2474,#2472,#1707,.T.);
#3039=EDGE_CURVE('',#2471,#2473,#1708,.T.);
#3040=EDGE_CURVE('',#2475,#2476,#1832,.T.);
#3041=EDGE_CURVE('',#2476,#2474,#1709,.T.);
#3042=EDGE_CURVE('',#2473,#2475,#1710,.T.);
#3043=EDGE_CURVE('',#2477,#2478,#1833,.T.);
#3044=EDGE_CURVE('',#2478,#2476,#1711,.T.);
#3045=EDGE_CURVE('',#2475,#2477,#1712,.T.);
#3046=EDGE_CURVE('',#2479,#2480,#1834,.T.);
#3047=EDGE_CURVE('',#2480,#2478,#1713,.T.);
#3048=EDGE_CURVE('',#2477,#2479,#1714,.T.);
#3049=EDGE_CURVE('',#2481,#2482,#1835,.T.);
#3050=EDGE_CURVE('',#2482,#2480,#1715,.T.);
#3051=EDGE_CURVE('',#2479,#2481,#1716,.T.);
#3052=EDGE_CURVE('',#2483,#2484,#1836,.T.);
#3053=EDGE_CURVE('',#2484,#2482,#1717,.T.);
#3054=EDGE_CURVE('',#2481,#2483,#1718,.T.);
#3055=EDGE_CURVE('',#2485,#2486,#1837,.T.);
#3056=EDGE_CURVE('',#2486,#2484,#1719,.T.);
#3057=EDGE_CURVE('',#2483,#2485,#1720,.T.);
#3058=EDGE_CURVE('',#2487,#2488,#1838,.T.);
#3059=EDGE_CURVE('',#2488,#2486,#1721,.T.);
#3060=EDGE_CURVE('',#2485,#2487,#1722,.T.);
#3061=EDGE_CURVE('',#2489,#2490,#1839,.T.);
#3062=EDGE_CURVE('',#2490,#2488,#1723,.T.);
#3063=EDGE_CURVE('',#2487,#2489,#1724,.T.);
#3064=EDGE_CURVE('',#2491,#2492,#1840,.T.);
#3065=EDGE_CURVE('',#2492,#2490,#1725,.T.);
#3066=EDGE_CURVE('',#2489,#2491,#1726,.T.);
#3067=EDGE_CURVE('',#2493,#2494,#1841,.T.);
#3068=EDGE_CURVE('',#2494,#2492,#1727,.T.);
#3069=EDGE_CURVE('',#2491,#2493,#1728,.T.);
#3070=EDGE_CURVE('',#2495,#2496,#1842,.T.);
#3071=EDGE_CURVE('',#2496,#2494,#1729,.T.);
#3072=EDGE_CURVE('',#2493,#2495,#1730,.T.);
#3073=EDGE_CURVE('',#2497,#2498,#1843,.T.);
#3074=EDGE_CURVE('',#2498,#2496,#1731,.T.);
#3075=EDGE_CURVE('',#2495,#2497,#1732,.T.);
#3076=EDGE_CURVE('',#2499,#2500,#1844,.T.);
#3077=EDGE_CURVE('',#2500,#2498,#1733,.T.);
#3078=EDGE_CURVE('',#2497,#2499,#1734,.T.);
#3079=EDGE_CURVE('',#2501,#2502,#1845,.T.);
#3080=EDGE_CURVE('',#2502,#2500,#1735,.T.);
#3081=EDGE_CURVE('',#2499,#2501,#1736,.T.);
#3082=EDGE_CURVE('',#2503,#2504,#1846,.T.);
#3083=EDGE_CURVE('',#2504,#2502,#1737,.T.);
#3084=EDGE_CURVE('',#2501,#2503,#1738,.T.);
#3085=EDGE_CURVE('',#2505,#2506,#1847,.T.);
#3086=EDGE_CURVE('',#2506,#2504,#1739,.T.);
#3087=EDGE_CURVE('',#2503,#2505,#1740,.T.);
#3088=EDGE_CURVE('',#2507,#2508,#1848,.T.);
#3089=EDGE_CURVE('',#2508,#2506,#1741,.T.);
#3090=EDGE_CURVE('',#2505,#2507,#1742,.T.);
#3091=EDGE_CURVE('',#2509,#2510,#1849,.T.);
#3092=EDGE_CURVE('',#2509,#2511,#1743,.T.);
#3093=EDGE_CURVE('',#2511,#2512,#1302,.T.);
#3094=EDGE_CURVE('',#2512,#2510,#1744,.T.);
#3095=EDGE_CURVE('',#2513,#2514,#1303,.T.);
#3096=EDGE_CURVE('',#2514,#2513,#1304,.T.);
#3097=EDGE_CURVE('',#2514,#2515,#1305,.T.);
#3098=EDGE_CURVE('',#2515,#2515,#1306,.T.);
#3099=EDGE_CURVE('',#2516,#2516,#1307,.T.);
#3100=EDGE_CURVE('',#2516,#2517,#1308,.T.);
#3101=EDGE_CURVE('',#2518,#2517,#1309,.T.);
#3102=EDGE_CURVE('',#2517,#2518,#1310,.T.);
#3103=EDGE_CURVE('',#2519,#2520,#1311,.T.);
#3104=EDGE_CURVE('',#2521,#2519,#1312,.T.);
#3105=EDGE_CURVE('',#2522,#2521,#1313,.T.);
#3106=EDGE_CURVE('',#2522,#2520,#1314,.T.);
#3107=EDGE_CURVE('',#2523,#2524,#1315,.T.);
#3108=EDGE_CURVE('',#2525,#2524,#1850,.T.);
#3109=EDGE_CURVE('',#2526,#2525,#454,.T.);
#3110=EDGE_CURVE('',#2527,#2526,#1745,.T.);
#3111=EDGE_CURVE('',#2523,#2527,#1851,.T.);
#3112=EDGE_CURVE('',#2528,#2521,#1852,.T.);
#3113=EDGE_CURVE('',#2523,#2528,#1316,.T.);
#3114=EDGE_CURVE('',#2522,#2523,#1853,.T.);
#3115=EDGE_CURVE('',#2529,#2530,#1317,.T.);
#3116=EDGE_CURVE('',#2531,#2530,#1854,.T.);
#3117=EDGE_CURVE('',#2531,#2532,#1318,.T.);
#3118=EDGE_CURVE('',#2529,#2532,#1855,.T.);
#3119=EDGE_CURVE('',#2533,#2534,#1746,.T.);
#3120=EDGE_CURVE('',#2534,#2535,#455,.T.);
#3121=EDGE_CURVE('',#2536,#2535,#1856,.T.);
#3122=EDGE_CURVE('',#2529,#2536,#1319,.T.);
#3123=EDGE_CURVE('',#2533,#2529,#1857,.T.);
#3124=EDGE_CURVE('',#2468,#2537,#1858,.T.);
#3125=EDGE_CURVE('',#2537,#2537,#1320,.T.);
#3126=EDGE_CURVE('',#2538,#2539,#1747,.T.);
#3127=EDGE_CURVE('',#2539,#2540,#1748,.T.);
#3128=EDGE_CURVE('',#2541,#2540,#1321,.T.);
#3129=EDGE_CURVE('',#2541,#2542,#1749,.T.);
#3130=EDGE_CURVE('',#2542,#2543,#1750,.T.);
#3131=EDGE_CURVE('',#2544,#2543,#1322,.T.);
#3132=EDGE_CURVE('',#2544,#2538,#1751,.T.);
#3133=EDGE_CURVE('',#2545,#2546,#1323,.T.);
#3134=EDGE_CURVE('',#2545,#2547,#1752,.T.);
#3135=EDGE_CURVE('',#2548,#2547,#1324,.T.);
#3136=EDGE_CURVE('',#2549,#2548,#1325,.T.);
#3137=EDGE_CURVE('',#2549,#2546,#1753,.T.);
#3138=EDGE_CURVE('',#2550,#2551,#1326,.T.);
#3139=EDGE_CURVE('',#2550,#2552,#1754,.T.);
#3140=EDGE_CURVE('',#2553,#2552,#1327,.T.);
#3141=EDGE_CURVE('',#2553,#2551,#1755,.T.);
#3142=EDGE_CURVE('',#2510,#2508,#1756,.T.);
#3143=EDGE_CURVE('',#2507,#2509,#1757,.T.);
#3144=EDGE_CURVE('',#2554,#2554,#1328,.T.);
#3145=EDGE_CURVE('',#2554,#2555,#1859,.T.);
#3146=EDGE_CURVE('',#2555,#2555,#1329,.T.);
#3147=EDGE_CURVE('',#2556,#2556,#1330,.T.);
#3148=EDGE_CURVE('',#2556,#2557,#1860,.T.);
#3149=EDGE_CURVE('',#2557,#2557,#1331,.T.);
#3150=EDGE_CURVE('',#2558,#2558,#1332,.T.);
#3151=EDGE_CURVE('',#2558,#2559,#1861,.T.);
#3152=EDGE_CURVE('',#2559,#2559,#1333,.T.);
#3153=EDGE_CURVE('',#2513,#2548,#1862,.T.);
#3154=EDGE_CURVE('',#2547,#2560,#1863,.T.);
#3155=EDGE_CURVE('',#2560,#2561,#1334,.T.);
#3156=EDGE_CURVE('',#2561,#2518,#1864,.T.);
#3157=EDGE_CURVE('',#2561,#2562,#1335,.T.);
#3158=EDGE_CURVE('',#2562,#2549,#1865,.T.);
#3159=EDGE_CURVE('',#2540,#2563,#1866,.T.);
#3160=EDGE_CURVE('',#2563,#2564,#1336,.T.);
#3161=EDGE_CURVE('',#2564,#2541,#1867,.T.);
#3162=EDGE_CURVE('',#2565,#2553,#1868,.T.);
#3163=EDGE_CURVE('',#2552,#2566,#1869,.T.);
#3164=EDGE_CURVE('',#2566,#2565,#1337,.T.);
#3165=EDGE_CURVE('',#2567,#2568,#1338,.T.);
#3166=EDGE_CURVE('',#2568,#2569,#1339,.T.);
#3167=EDGE_CURVE('',#2569,#2570,#1340,.T.);
#3168=EDGE_CURVE('',#2570,#2571,#1341,.T.);
#3169=EDGE_CURVE('',#2571,#2572,#1342,.T.);
#3170=EDGE_CURVE('',#2572,#2567,#1343,.T.);
#3171=EDGE_CURVE('',#2573,#2574,#1870,.T.);
#3172=EDGE_CURVE('',#2574,#2575,#1871,.T.);
#3173=EDGE_CURVE('',#2575,#2576,#1872,.T.);
#3174=EDGE_CURVE('',#2576,#2568,#183,.T.);
#3175=EDGE_CURVE('',#2568,#2573,#184,.T.);
#3176=EDGE_CURVE('',#2577,#2578,#1873,.T.);
#3177=EDGE_CURVE('',#2578,#2579,#1874,.T.);
#3178=EDGE_CURVE('',#2579,#2580,#1875,.T.);
#3179=EDGE_CURVE('',#2580,#2567,#185,.T.);
#3180=EDGE_CURVE('',#2567,#2577,#186,.T.);
#3181=EDGE_CURVE('',#2581,#2582,#1876,.T.);
#3182=EDGE_CURVE('',#2582,#2583,#1877,.T.);
#3183=EDGE_CURVE('',#2583,#2584,#1878,.T.);
#3184=EDGE_CURVE('',#2584,#2572,#187,.T.);
#3185=EDGE_CURVE('',#2572,#2581,#188,.T.);
#3186=EDGE_CURVE('',#2585,#2586,#1879,.T.);
#3187=EDGE_CURVE('',#2586,#2587,#1880,.T.);
#3188=EDGE_CURVE('',#2587,#2588,#1881,.T.);
#3189=EDGE_CURVE('',#2588,#2571,#189,.T.);
#3190=EDGE_CURVE('',#2571,#2585,#190,.T.);
#3191=EDGE_CURVE('',#2589,#2590,#1882,.T.);
#3192=EDGE_CURVE('',#2590,#2591,#1883,.T.);
#3193=EDGE_CURVE('',#2591,#2592,#1884,.T.);
#3194=EDGE_CURVE('',#2592,#2570,#191,.T.);
#3195=EDGE_CURVE('',#2570,#2589,#192,.T.);
#3196=EDGE_CURVE('',#2593,#2594,#1885,.T.);
#3197=EDGE_CURVE('',#2594,#2595,#1886,.T.);
#3198=EDGE_CURVE('',#2595,#2596,#1887,.T.);
#3199=EDGE_CURVE('',#2596,#2569,#193,.T.);
#3200=EDGE_CURVE('',#2569,#2593,#194,.T.);
#3201=EDGE_CURVE('',#2597,#2598,#1758,.T.);
#3202=EDGE_CURVE('',#2599,#2597,#1759,.T.);
#3203=EDGE_CURVE('',#2599,#2598,#1344,.T.);
#3204=EDGE_CURVE('',#2511,#2600,#1760,.T.);
#3205=EDGE_CURVE('',#2600,#2598,#1761,.T.);
#3206=EDGE_CURVE('',#2599,#2601,#1762,.T.);
#3207=EDGE_CURVE('',#2601,#2512,#1763,.T.);
#3208=EDGE_CURVE('',#2602,#2603,#1888,.T.);
#3209=EDGE_CURVE('',#2603,#2604,#1889,.T.);
#3210=EDGE_CURVE('',#2604,#2605,#1890,.T.);
#3211=EDGE_CURVE('',#2605,#2606,#456,.T.);
#3212=EDGE_CURVE('',#2606,#2607,#1891,.T.);
#3213=EDGE_CURVE('',#2607,#2602,#1892,.T.);
#3214=EDGE_CURVE('',#2608,#2609,#1893,.T.);
#3215=EDGE_CURVE('',#2609,#2610,#1894,.T.);
#3216=EDGE_CURVE('',#2610,#2611,#1895,.T.);
#3217=EDGE_CURVE('',#2611,#2612,#1896,.T.);
#3218=EDGE_CURVE('',#2612,#2613,#1897,.T.);
#3219=EDGE_CURVE('',#2613,#2608,#457,.T.);
#3220=EDGE_CURVE('',#2614,#2615,#1898,.T.);
#3221=EDGE_CURVE('',#2614,#2616,#1899,.T.);
#3222=EDGE_CURVE('',#2616,#2617,#1345,.T.);
#3223=EDGE_CURVE('',#2617,#2615,#1900,.T.);
#3224=EDGE_CURVE('',#2618,#2619,#1901,.T.);
#3225=EDGE_CURVE('',#2618,#2614,#1346,.T.);
#3226=EDGE_CURVE('',#2615,#2619,#1347,.T.);
#3227=EDGE_CURVE('',#2620,#2621,#1902,.T.);
#3228=EDGE_CURVE('',#2620,#2618,#1903,.T.);
#3229=EDGE_CURVE('',#2619,#2621,#1904,.T.);
#3230=EDGE_CURVE('',#2622,#2623,#1905,.T.);
#3231=EDGE_CURVE('',#2622,#2620,#1348,.T.);
#3232=EDGE_CURVE('',#2621,#2623,#1349,.T.);
#3233=EDGE_CURVE('',#2623,#2624,#1906,.T.);
#3234=EDGE_CURVE('',#2624,#2625,#1907,.T.);
#3235=EDGE_CURVE('',#2625,#2622,#1908,.T.);
#3236=EDGE_CURVE('',#2551,#2626,#1350,.T.);
#3237=EDGE_CURVE('',#2626,#2627,#1909,.T.);
#3238=EDGE_CURVE('',#2627,#2628,#1351,.T.);
#3239=EDGE_CURVE('',#2628,#2629,#1910,.T.);
#3240=EDGE_CURVE('',#2629,#2630,#1352,.T.);
#3241=EDGE_CURVE('',#2630,#2631,#1911,.T.);
#3242=EDGE_CURVE('',#2631,#2550,#1353,.T.);
#3243=EDGE_CURVE('',#2632,#2633,#1912,.T.);
#3244=EDGE_CURVE('',#2633,#2634,#1913,.T.);
#3245=EDGE_CURVE('',#2634,#2635,#1914,.T.);
#3246=EDGE_CURVE('',#2635,#2636,#458,.T.);
#3247=EDGE_CURVE('',#2636,#2637,#1915,.T.);
#3248=EDGE_CURVE('',#2637,#2632,#1916,.T.);
#3249=EDGE_CURVE('',#2638,#2639,#1917,.T.);
#3250=EDGE_CURVE('',#2638,#2640,#1918,.T.);
#3251=EDGE_CURVE('',#2640,#2641,#1354,.T.);
#3252=EDGE_CURVE('',#2641,#2639,#1919,.T.);
#3253=EDGE_CURVE('',#2639,#2525,#1355,.T.);
#3254=EDGE_CURVE('',#2642,#2525,#1920,.T.);
#3255=EDGE_CURVE('',#2642,#2638,#1356,.T.);
#3256=EDGE_CURVE('',#2643,#2524,#1921,.T.);
#3257=EDGE_CURVE('',#2643,#2642,#1922,.T.);
#3258=EDGE_CURVE('',#2524,#2528,#1357,.T.);
#3259=EDGE_CURVE('',#2644,#2528,#1923,.T.);
#3260=EDGE_CURVE('',#2644,#2643,#1358,.T.);
#3261=EDGE_CURVE('',#2521,#2645,#1924,.T.);
#3262=EDGE_CURVE('',#2645,#2644,#1925,.T.);
#3263=EDGE_CURVE('',#2546,#2646,#1359,.T.);
#3264=EDGE_CURVE('',#2646,#2647,#1926,.T.);
#3265=EDGE_CURVE('',#2647,#2648,#1360,.T.);
#3266=EDGE_CURVE('',#2648,#2519,#1927,.T.);
#3267=EDGE_CURVE('',#2520,#2649,#1928,.T.);
#3268=EDGE_CURVE('',#2649,#2545,#1361,.T.);
#3269=EDGE_CURVE('',#2650,#2651,#1929,.T.);
#3270=EDGE_CURVE('',#2651,#2522,#1930,.T.);
#3271=EDGE_CURVE('',#2527,#2652,#1931,.T.);
#3272=EDGE_CURVE('',#2652,#2650,#459,.T.);
#3273=EDGE_CURVE('',#2532,#2653,#1932,.T.);
#3274=EDGE_CURVE('',#2653,#2654,#1933,.T.);
#3275=EDGE_CURVE('',#2654,#2655,#460,.T.);
#3276=EDGE_CURVE('',#2655,#2533,#1934,.T.);
#3277=EDGE_CURVE('',#2656,#2657,#1935,.T.);
#3278=EDGE_CURVE('',#2656,#2544,#1936,.T.);
#3279=EDGE_CURVE('',#2543,#2657,#1937,.T.);
#3280=EDGE_CURVE('',#2657,#2658,#1362,.T.);
#3281=EDGE_CURVE('',#2535,#2658,#1938,.T.);
#3282=EDGE_CURVE('',#2535,#2656,#1363,.T.);
#3283=EDGE_CURVE('',#2658,#2659,#1939,.T.);
#3284=EDGE_CURVE('',#2536,#2659,#1940,.T.);
#3285=EDGE_CURVE('',#2659,#2660,#1364,.T.);
#3286=EDGE_CURVE('',#2530,#2660,#1941,.T.);
#3287=EDGE_CURVE('',#2530,#2536,#1365,.T.);
#3288=EDGE_CURVE('',#2660,#2661,#1942,.T.);
#3289=EDGE_CURVE('',#2661,#2531,#1943,.T.);
#3290=EDGE_CURVE('',#2662,#2663,#1366,.T.);
#3291=EDGE_CURVE('',#2663,#2664,#1367,.T.);
#3292=EDGE_CURVE('',#2664,#2665,#1944,.T.);
#3293=EDGE_CURVE('',#2665,#2666,#1368,.T.);
#3294=EDGE_CURVE('',#2666,#2667,#1945,.T.);
#3295=EDGE_CURVE('',#2667,#2668,#1369,.T.);
#3296=EDGE_CURVE('',#2668,#2669,#1946,.T.);
#3297=EDGE_CURVE('',#2669,#2662,#1370,.T.);
#3298=EDGE_CURVE('',#2670,#2671,#1947,.T.);
#3299=EDGE_CURVE('',#2671,#2672,#1948,.T.);
#3300=EDGE_CURVE('',#2672,#2673,#1949,.T.);
#3301=EDGE_CURVE('',#2673,#2674,#1950,.T.);
#3302=EDGE_CURVE('',#2674,#2675,#1951,.T.);
#3303=EDGE_CURVE('',#2675,#2670,#461,.T.);
#3304=EDGE_CURVE('',#2552,#2676,#1764,.T.);
#3305=EDGE_CURVE('',#2676,#2609,#1371,.T.);
#3306=EDGE_CURVE('',#2608,#2566,#1765,.T.);
#3307=EDGE_CURVE('',#2653,#2677,#1372,.T.);
#3308=EDGE_CURVE('',#2677,#2563,#1766,.T.);
#3309=EDGE_CURVE('',#2540,#2654,#1767,.T.);
#3310=EDGE_CURVE('',#2564,#2678,#1768,.T.);
#3311=EDGE_CURVE('',#2678,#2671,#1373,.T.);
#3312=EDGE_CURVE('',#2670,#2541,#1769,.T.);
#3313=EDGE_CURVE('',#2634,#2679,#1374,.T.);
#3314=EDGE_CURVE('',#2679,#2549,#1770,.T.);
#3315=EDGE_CURVE('',#2562,#2635,#1771,.T.);
#3316=EDGE_CURVE('',#2547,#2680,#1772,.T.);
#3317=EDGE_CURVE('',#2680,#2651,#1375,.T.);
#3318=EDGE_CURVE('',#2650,#2560,#1773,.T.);
#3319=EDGE_CURVE('',#2604,#2681,#1376,.T.);
#3320=EDGE_CURVE('',#2681,#2553,#1774,.T.);
#3321=EDGE_CURVE('',#2565,#2605,#1775,.T.);
#3322=EDGE_CURVE('',#2563,#2663,#1776,.T.);
#3323=EDGE_CURVE('',#2662,#2564,#1777,.T.);
#3324=EDGE_CURVE('',#2560,#2682,#1778,.T.);
#3325=EDGE_CURVE('',#2682,#2641,#1779,.T.);
#3326=EDGE_CURVE('',#2640,#2683,#1780,.T.);
#3327=EDGE_CURVE('',#2683,#2562,#1781,.T.);
#3328=EDGE_CURVE('',#2616,#2684,#1782,.T.);
#3329=EDGE_CURVE('',#2684,#2565,#1783,.T.);
#3330=EDGE_CURVE('',#2566,#2685,#1784,.T.);
#3331=EDGE_CURVE('',#2685,#2617,#1785,.T.);
#3332=EDGE_CURVE('',#2686,#2465,#1786,.T.);
#3333=EDGE_CURVE('',#2687,#2686,#1787,.T.);
#3334=EDGE_CURVE('',#2688,#2687,#1788,.T.);
#3335=EDGE_CURVE('',#2466,#2688,#1789,.T.);
#3336=EDGE_CURVE('',#2600,#2688,#195,.T.);
#3337=EDGE_CURVE('',#2597,#2687,#196,.T.);
#3338=EDGE_CURVE('',#2601,#2686,#197,.T.);
#3339=EDGE_CURVE('',#2689,#2690,#1952,.T.);
#3340=EDGE_CURVE('',#2690,#2691,#1377,.T.);
#3341=EDGE_CURVE('',#2691,#2692,#1953,.T.);
#3342=EDGE_CURVE('',#2692,#2693,#1378,.T.);
#3343=EDGE_CURVE('',#2693,#2694,#1954,.T.);
#3344=EDGE_CURVE('',#2694,#2695,#1379,.T.);
#3345=EDGE_CURVE('',#2695,#2696,#1955,.T.);
#3346=EDGE_CURVE('',#2696,#2697,#1380,.T.);
#3347=EDGE_CURVE('',#2697,#2698,#1956,.T.);
#3348=EDGE_CURVE('',#2698,#2699,#1381,.T.);
#3349=EDGE_CURVE('',#2699,#2700,#1957,.T.);
#3350=EDGE_CURVE('',#2700,#2689,#1382,.T.);
#3351=EDGE_CURVE('',#2576,#2593,#1790,.T.);
#3352=EDGE_CURVE('',#2596,#2589,#1791,.T.);
#3353=EDGE_CURVE('',#2592,#2585,#1792,.T.);
#3354=EDGE_CURVE('',#2588,#2581,#1793,.T.);
#3355=EDGE_CURVE('',#2584,#2577,#1794,.T.);
#3356=EDGE_CURVE('',#2580,#2573,#1795,.T.);
#3357=EDGE_CURVE('',#2583,#2578,#1383,.T.);
#3358=EDGE_CURVE('',#2587,#2582,#1384,.T.);
#3359=EDGE_CURVE('',#2591,#2586,#1385,.T.);
#3360=EDGE_CURVE('',#2595,#2590,#1386,.T.);
#3361=EDGE_CURVE('',#2575,#2594,#1387,.T.);
#3362=EDGE_CURVE('',#2579,#2574,#1388,.T.);
#3363=EDGE_CURVE('',#2594,#2696,#1389,.T.);
#3364=EDGE_CURVE('',#2697,#2575,#1390,.T.);
#3365=EDGE_CURVE('',#2698,#2574,#1391,.T.);
#3366=EDGE_CURVE('',#2595,#2695,#1392,.T.);
#3367=EDGE_CURVE('',#2699,#2579,#1393,.T.);
#3368=EDGE_CURVE('',#2590,#2694,#1394,.T.);
#3369=EDGE_CURVE('',#2700,#2578,#1395,.T.);
#3370=EDGE_CURVE('',#2591,#2693,#1396,.T.);
#3371=EDGE_CURVE('',#2689,#2583,#1397,.T.);
#3372=EDGE_CURVE('',#2586,#2692,#1398,.T.);
#3373=EDGE_CURVE('',#2690,#2582,#1399,.T.);
#3374=EDGE_CURVE('',#2587,#2691,#1400,.T.);
#3375=EDGE_CURVE('',#2625,#2603,#1401,.T.);
#3376=EDGE_CURVE('',#2622,#2602,#1402,.T.);
#3377=EDGE_CURVE('',#2620,#2602,#1403,.T.);
#3378=EDGE_CURVE('',#2618,#2607,#1796,.T.);
#3379=EDGE_CURVE('',#2614,#2607,#1797,.T.);
#3380=EDGE_CURVE('',#2616,#2606,#1404,.T.);
#3381=EDGE_CURVE('',#2684,#2605,#1405,.T.);
#3382=EDGE_CURVE('',#2610,#2624,#1406,.T.);
#3383=EDGE_CURVE('',#2611,#2623,#1407,.T.);
#3384=EDGE_CURVE('',#2611,#2621,#1408,.T.);
#3385=EDGE_CURVE('',#2612,#2619,#1798,.T.);
#3386=EDGE_CURVE('',#2612,#2615,#1799,.T.);
#3387=EDGE_CURVE('',#2613,#2617,#1409,.T.);
#3388=EDGE_CURVE('',#2608,#2685,#1410,.T.);
#3389=EDGE_CURVE('',#2672,#2661,#1411,.T.);
#3390=EDGE_CURVE('',#2673,#2660,#1412,.T.);
#3391=EDGE_CURVE('',#2673,#2659,#1413,.T.);
#3392=EDGE_CURVE('',#2674,#2658,#1800,.T.);
#3393=EDGE_CURVE('',#2674,#2657,#1801,.T.);
#3394=EDGE_CURVE('',#2675,#2543,#1414,.T.);
#3395=EDGE_CURVE('',#2670,#2542,#1415,.T.);
#3396=EDGE_CURVE('',#2654,#2538,#1416,.T.);
#3397=EDGE_CURVE('',#2655,#2544,#1417,.T.);
#3398=EDGE_CURVE('',#2533,#2656,#1802,.T.);
#3399=EDGE_CURVE('',#2527,#2639,#1803,.T.);
#3400=EDGE_CURVE('',#2652,#2641,#1418,.T.);
#3401=EDGE_CURVE('',#2650,#2682,#1419,.T.);
#3402=EDGE_CURVE('',#2635,#2683,#1420,.T.);
#3403=EDGE_CURVE('',#2636,#2640,#1421,.T.);
#3404=EDGE_CURVE('',#2637,#2638,#1804,.T.);
#3405=EDGE_CURVE('',#2637,#2642,#1805,.T.);
#3406=EDGE_CURVE('',#2632,#2643,#1422,.T.);
#3407=EDGE_CURVE('',#2632,#2644,#1423,.T.);
#3408=EDGE_CURVE('',#2645,#2633,#1424,.T.);
#3409=EDGE_CURVE('',#2551,#2681,#1425,.T.);
#3410=EDGE_CURVE('',#2626,#2604,#1426,.T.);
#3411=EDGE_CURVE('',#2627,#2603,#1427,.T.);
#3412=EDGE_CURVE('',#2628,#2625,#1428,.T.);
#3413=EDGE_CURVE('',#2629,#2624,#1429,.T.);
#3414=EDGE_CURVE('',#2630,#2610,#1430,.T.);
#3415=EDGE_CURVE('',#2631,#2609,#1431,.T.);
#3416=EDGE_CURVE('',#2550,#2676,#1432,.T.);
#3417=EDGE_CURVE('',#2678,#2662,#1433,.T.);
#3418=EDGE_CURVE('',#2671,#2669,#1434,.T.);
#3419=EDGE_CURVE('',#2672,#2668,#1435,.T.);
#3420=EDGE_CURVE('',#2661,#2667,#1436,.T.);
#3421=EDGE_CURVE('',#2531,#2666,#1437,.T.);
#3422=EDGE_CURVE('',#2532,#2665,#1438,.T.);
#3423=EDGE_CURVE('',#2653,#2664,#1439,.T.);
#3424=EDGE_CURVE('',#2677,#2663,#1440,.T.);
#3425=EDGE_CURVE('',#2680,#2545,#1441,.T.);
#3426=EDGE_CURVE('',#2651,#2649,#1442,.T.);
#3427=EDGE_CURVE('',#2645,#2648,#1443,.T.);
#3428=EDGE_CURVE('',#2633,#2647,#1444,.T.);
#3429=EDGE_CURVE('',#2634,#2646,#1445,.T.);
#3430=EDGE_CURVE('',#2679,#2546,#1446,.T.);
#3431=EDGE_CURVE('',#2701,#2702,#1806,.T.);
#3432=EDGE_CURVE('',#2701,#2703,#1447,.T.);
#3433=EDGE_CURVE('',#2704,#2703,#1807,.T.);
#3434=EDGE_CURVE('',#2705,#2704,#1808,.T.);
#3435=EDGE_CURVE('',#2706,#2705,#1448,.T.);
#3436=EDGE_CURVE('',#2702,#2706,#1809,.T.);
#3437=EDGE_CURVE('',#2707,#2708,#1810,.T.);
#3438=EDGE_CURVE('',#2707,#2709,#1449,.T.);
#3439=EDGE_CURVE('',#2710,#2709,#1811,.T.);
#3440=EDGE_CURVE('',#2711,#2710,#1450,.T.);
#3441=EDGE_CURVE('',#2712,#2711,#1451,.T.);
#3442=EDGE_CURVE('',#2708,#2712,#1812,.T.);
#3443=EDGE_CURVE('',#2713,#2714,#1452,.T.);
#3444=EDGE_CURVE('',#2713,#2715,#198,.T.);
#3445=EDGE_CURVE('',#2715,#2714,#199,.T.);
#3446=EDGE_CURVE('',#2716,#2707,#1813,.T.);
#3447=EDGE_CURVE('',#2708,#2717,#1958,.T.);
#3448=EDGE_CURVE('',#2717,#2701,#462,.T.);
#3449=EDGE_CURVE('',#2706,#2717,#1814,.T.);
#3450=EDGE_CURVE('',#2712,#2716,#1815,.T.);
#3451=EDGE_CURVE('',#2718,#2719,#1453,.T.);
#3452=EDGE_CURVE('',#2719,#2718,#1454,.T.);
#3453=EDGE_CURVE('',#2719,#2720,#1959,.T.);
#3454=EDGE_CURVE('',#2720,#2720,#1455,.T.);
#3455=EDGE_CURVE('',#2718,#2721,#1960,.T.);
#3456=EDGE_CURVE('',#2722,#2723,#1456,.T.);
#3457=EDGE_CURVE('',#2723,#2722,#1457,.T.);
#3458=EDGE_CURVE('',#2723,#2724,#1961,.T.);
#3459=EDGE_CURVE('',#2724,#2724,#1458,.T.);
#3460=EDGE_CURVE('',#2725,#2725,#1459,.T.);
#3461=EDGE_CURVE('',#2725,#2726,#1962,.T.);
#3462=EDGE_CURVE('',#2726,#2726,#1460,.T.);
#3463=EDGE_CURVE('',#2722,#2704,#1963,.T.);
#3464=EDGE_CURVE('',#2703,#2727,#1816,.T.);
#3465=EDGE_CURVE('',#2727,#2728,#1964,.T.);
#3466=EDGE_CURVE('',#2728,#2728,#1461,.T.);
#3467=EDGE_CURVE('',#2727,#2705,#1817,.T.);
#3468=EDGE_CURVE('',#2709,#2729,#1462,.T.);
#3469=EDGE_CURVE('',#2729,#2711,#1818,.T.);
#3470=EDGE_CURVE('',#2730,#2731,#1819,.T.);
#3471=EDGE_CURVE('',#2731,#2732,#1820,.T.);
#3472=EDGE_CURVE('',#2732,#2730,#1821,.T.);
#3473=EDGE_CURVE('',#2733,#2731,#200,.T.);
#3474=EDGE_CURVE('',#2733,#2734,#1822,.T.);
#3475=EDGE_CURVE('',#2734,#2732,#201,.T.);
#3476=EDGE_CURVE('',#2735,#2730,#202,.T.);
#3477=EDGE_CURVE('',#2735,#2733,#1823,.T.);
#3478=EDGE_CURVE('',#2734,#2735,#1824,.T.);
#3479=EDGE_CURVE('',#2736,#2737,#1965,.T.);
#3480=EDGE_CURVE('',#2736,#2738,#1966,.T.);
#3481=EDGE_CURVE('',#2738,#2739,#1967,.T.);
#3482=EDGE_CURVE('',#2740,#2739,#203,.T.);
#3483=EDGE_CURVE('',#2741,#2740,#1968,.T.);
#3484=EDGE_CURVE('',#2737,#2741,#204,.T.);
#3485=EDGE_CURVE('',#2738,#2742,#1969,.T.);
#3486=EDGE_CURVE('',#2742,#2743,#1970,.T.);
#3487=EDGE_CURVE('',#2744,#2743,#205,.T.);
#3488=EDGE_CURVE('',#2745,#2744,#1971,.T.);
#3489=EDGE_CURVE('',#2739,#2745,#206,.T.);
#3490=EDGE_CURVE('',#2742,#2746,#1972,.T.);
#3491=EDGE_CURVE('',#2746,#2747,#1973,.T.);
#3492=EDGE_CURVE('',#2748,#2747,#207,.T.);
#3493=EDGE_CURVE('',#2749,#2748,#1974,.T.);
#3494=EDGE_CURVE('',#2743,#2749,#208,.T.);
#3495=EDGE_CURVE('',#2746,#2750,#1975,.T.);
#3496=EDGE_CURVE('',#2750,#2751,#1976,.T.);
#3497=EDGE_CURVE('',#2752,#2751,#209,.T.);
#3498=EDGE_CURVE('',#2753,#2752,#1977,.T.);
#3499=EDGE_CURVE('',#2747,#2753,#210,.T.);
#3500=EDGE_CURVE('',#2750,#2754,#1978,.T.);
#3501=EDGE_CURVE('',#2754,#2715,#1979,.T.);
#3502=EDGE_CURVE('',#2755,#2713,#1980,.T.);
#3503=EDGE_CURVE('',#2751,#2755,#211,.T.);
#3504=EDGE_CURVE('',#2754,#2736,#1981,.T.);
#3505=EDGE_CURVE('',#2756,#2737,#212,.T.);
#3506=EDGE_CURVE('',#2714,#2756,#1982,.T.);
#3507=EDGE_CURVE('',#2756,#2741,#1463,.T.);
#3508=EDGE_CURVE('',#2752,#2755,#1464,.T.);
#3509=EDGE_CURVE('',#2748,#2753,#1465,.T.);
#3510=EDGE_CURVE('',#2744,#2749,#1466,.T.);
#3511=EDGE_CURVE('',#2740,#2745,#1467,.T.);
#3512=EDGE_CURVE('',#2757,#2758,#1468,.T.);
#3513=EDGE_CURVE('',#2757,#2759,#1469,.T.);
#3514=EDGE_CURVE('',#2758,#2757,#1470,.T.);
#3515=EDGE_CURVE('',#2760,#2761,#1471,.T.);
#3516=EDGE_CURVE('',#2762,#2761,#1472,.T.);
#3517=EDGE_CURVE('',#2761,#2760,#1473,.T.);
#3518=EDGE_CURVE('',#2758,#2760,#1983,.T.);
#3519=EDGE_CURVE('',#2763,#2763,#1474,.T.);
#3520=EDGE_CURVE('',#2763,#2764,#1984,.T.);
#3521=EDGE_CURVE('',#2765,#2764,#1475,.T.);
#3522=EDGE_CURVE('',#2764,#2765,#1476,.T.);
#3523=EDGE_CURVE('',#2766,#2767,#1477,.T.);
#3524=EDGE_CURVE('',#2767,#2766,#1478,.T.);
#3525=EDGE_CURVE('',#2767,#2765,#1985,.T.);
#3526=EDGE_CURVE('',#2768,#2768,#1479,.T.);
#3527=EDGE_CURVE('',#2768,#2769,#1986,.T.);
#3528=EDGE_CURVE('',#2770,#2769,#1480,.T.);
#3529=EDGE_CURVE('',#2769,#2770,#1481,.T.);
#3530=EDGE_CURVE('',#2771,#2772,#1482,.T.);
#3531=EDGE_CURVE('',#2772,#2771,#1483,.T.);
#3532=EDGE_CURVE('',#2772,#2770,#1987,.T.);
#3533=EDGE_CURVE('',#2773,#2773,#1484,.T.);
#3534=EDGE_CURVE('',#2773,#2774,#1988,.T.);
#3535=EDGE_CURVE('',#2775,#2774,#1485,.T.);
#3536=EDGE_CURVE('',#2774,#2775,#1486,.T.);
#3537=EDGE_CURVE('',#2776,#2777,#1487,.T.);
#3538=EDGE_CURVE('',#2777,#2776,#1488,.T.);
#3539=EDGE_CURVE('',#2777,#2775,#1989,.T.);
#3540=EDGE_CURVE('',#2778,#2778,#1489,.T.);
#3541=EDGE_CURVE('',#2778,#2779,#1990,.T.);
#3542=EDGE_CURVE('',#2780,#2779,#1490,.T.);
#3543=EDGE_CURVE('',#2779,#2780,#1491,.T.);
#3544=EDGE_CURVE('',#2781,#2782,#1492,.T.);
#3545=EDGE_CURVE('',#2782,#2780,#1991,.T.);
#3546=EDGE_CURVE('',#2782,#2781,#1493,.T.);
#3547=EDGE_CURVE('',#2783,#2783,#1494,.T.);
#3548=EDGE_CURVE('',#2783,#2784,#1992,.T.);
#3549=EDGE_CURVE('',#2784,#2785,#1495,.T.);
#3550=EDGE_CURVE('',#2785,#2784,#1496,.T.);
#3551=EDGE_CURVE('',#2786,#2787,#1497,.T.);
#3552=EDGE_CURVE('',#2787,#2785,#1993,.T.);
#3553=EDGE_CURVE('',#2787,#2786,#1498,.T.);
#3554=EDGE_CURVE('',#2781,#2788,#1994,.T.);
#3555=EDGE_CURVE('',#2788,#2788,#1499,.T.);
#3556=EDGE_CURVE('',#2776,#2778,#1995,.T.);
#3557=EDGE_CURVE('',#2771,#2773,#1996,.T.);
#3558=EDGE_CURVE('',#2766,#2768,#1997,.T.);
#3559=EDGE_CURVE('',#2786,#2763,#1998,.T.);
#3560=EDGE_CURVE('',#2789,#2790,#1999,.T.);
#3561=EDGE_CURVE('',#2790,#2791,#213,.T.);
#3562=EDGE_CURVE('',#2791,#2792,#214,.T.);
#3563=EDGE_CURVE('',#2793,#2792,#2000,.T.);
#3564=EDGE_CURVE('',#2794,#2793,#215,.T.);
#3565=EDGE_CURVE('',#2789,#2794,#216,.T.);
#3566=EDGE_CURVE('',#2792,#2795,#217,.T.);
#3567=EDGE_CURVE('',#2795,#2796,#218,.T.);
#3568=EDGE_CURVE('',#2797,#2796,#2001,.T.);
#3569=EDGE_CURVE('',#2798,#2797,#219,.T.);
#3570=EDGE_CURVE('',#2793,#2798,#220,.T.);
#3571=EDGE_CURVE('',#2799,#2800,#221,.T.);
#3572=EDGE_CURVE('',#2801,#2799,#2002,.T.);
#3573=EDGE_CURVE('',#2801,#2802,#222,.T.);
#3574=EDGE_CURVE('',#2802,#2797,#223,.T.);
#3575=EDGE_CURVE('',#2800,#2796,#224,.T.);
#3576=EDGE_CURVE('',#2799,#2803,#225,.T.);
#3577=EDGE_CURVE('',#2803,#2804,#226,.T.);
#3578=EDGE_CURVE('',#2805,#2804,#2003,.T.);
#3579=EDGE_CURVE('',#2806,#2805,#227,.T.);
#3580=EDGE_CURVE('',#2801,#2806,#228,.T.);
#3581=EDGE_CURVE('',#2804,#2807,#229,.T.);
#3582=EDGE_CURVE('',#2807,#2808,#230,.T.);
#3583=EDGE_CURVE('',#2809,#2808,#2004,.T.);
#3584=EDGE_CURVE('',#2810,#2809,#231,.T.);
#3585=EDGE_CURVE('',#2805,#2810,#232,.T.);
#3586=EDGE_CURVE('',#2808,#2811,#233,.T.);
#3587=EDGE_CURVE('',#2811,#2790,#234,.T.);
#3588=EDGE_CURVE('',#2812,#2789,#235,.T.);
#3589=EDGE_CURVE('',#2809,#2812,#236,.T.);
#3590=EDGE_CURVE('',#2803,#2800,#1500,.T.);
#3591=EDGE_CURVE('',#2800,#2795,#1501,.T.);
#3592=EDGE_CURVE('',#2795,#2791,#1502,.T.);
#3593=EDGE_CURVE('',#2791,#2811,#1503,.T.);
#3594=EDGE_CURVE('',#2811,#2807,#1504,.T.);
#3595=EDGE_CURVE('',#2807,#2803,#1505,.T.);
#3596=EDGE_CURVE('',#2802,#2798,#1506,.T.);
#3597=EDGE_CURVE('',#2802,#2806,#1507,.T.);
#3598=EDGE_CURVE('',#2806,#2810,#1508,.T.);
#3599=EDGE_CURVE('',#2810,#2812,#1509,.T.);
#3600=EDGE_CURVE('',#2812,#2794,#1510,.T.);
#3601=EDGE_CURVE('',#2794,#2798,#1511,.T.);
#3602=EDGE_CURVE('',#2813,#2813,#1512,.T.);
#3603=EDGE_CURVE('',#2813,#2814,#2005,.T.);
#3604=EDGE_CURVE('',#2814,#2814,#1513,.T.);
#3605=EDGE_CURVE('',#2815,#2815,#1514,.T.);
#3606=EDGE_CURVE('',#2816,#2817,#1515,.T.);
#3607=EDGE_CURVE('',#2817,#2816,#1516,.T.);
#3608=EDGE_CURVE('',#2816,#2818,#2006,.T.);
#3609=EDGE_CURVE('',#2818,#2818,#1517,.T.);
#3610=EDGE_CURVE('',#2819,#2820,#1518,.T.);
#3611=EDGE_CURVE('',#2820,#2819,#1519,.T.);
#3612=EDGE_CURVE('',#2820,#2821,#2007,.T.);
#3613=EDGE_CURVE('',#2821,#2822,#1520,.T.);
#3614=EDGE_CURVE('',#2822,#2821,#1521,.T.);
#3615=EDGE_CURVE('',#2817,#2822,#2008,.T.);
#3616=EDGE_CURVE('',#2823,#2824,#1522,.T.);
#3617=EDGE_CURVE('',#2824,#2823,#1523,.T.);
#3618=EDGE_CURVE('',#2824,#2819,#2009,.T.);
#3619=EDGE_CURVE('',#2825,#2826,#1524,.T.);
#3620=EDGE_CURVE('',#2826,#2825,#1525,.T.);
#3621=EDGE_CURVE('',#2826,#2827,#2010,.T.);
#3622=EDGE_CURVE('',#2827,#2828,#1526,.T.);
#3623=EDGE_CURVE('',#2828,#2827,#1527,.T.);
#3624=EDGE_CURVE('',#2823,#2828,#2011,.T.);
#3625=EDGE_CURVE('',#2829,#2830,#1528,.T.);
#3626=EDGE_CURVE('',#2830,#2829,#1529,.T.);
#3627=EDGE_CURVE('',#2830,#2825,#2012,.T.);
#3628=EDGE_CURVE('',#2831,#2832,#1530,.T.);
#3629=EDGE_CURVE('',#2832,#2831,#1531,.T.);
#3630=EDGE_CURVE('',#2832,#2833,#2013,.T.);
#3631=EDGE_CURVE('',#2833,#2834,#1532,.T.);
#3632=EDGE_CURVE('',#2834,#2833,#1533,.T.);
#3633=EDGE_CURVE('',#2829,#2834,#2014,.T.);
#3634=EDGE_CURVE('',#2835,#2836,#1534,.T.);
#3635=EDGE_CURVE('',#2836,#2835,#1535,.T.);
#3636=EDGE_CURVE('',#2836,#2831,#2015,.T.);
#3637=EDGE_CURVE('',#2837,#2838,#1536,.T.);
#3638=EDGE_CURVE('',#2838,#2837,#1537,.T.);
#3639=EDGE_CURVE('',#2838,#2839,#2016,.T.);
#3640=EDGE_CURVE('',#2839,#2840,#1538,.T.);
#3641=EDGE_CURVE('',#2840,#2839,#1539,.T.);
#3642=EDGE_CURVE('',#2835,#2840,#2017,.T.);
#3643=EDGE_CURVE('',#2841,#2842,#1540,.T.);
#3644=EDGE_CURVE('',#2842,#2841,#1541,.T.);
#3645=EDGE_CURVE('',#2842,#2837,#2018,.T.);
#3646=EDGE_CURVE('',#2843,#2844,#1542,.T.);
#3647=EDGE_CURVE('',#2844,#2843,#1543,.T.);
#3648=EDGE_CURVE('',#2844,#2845,#2019,.T.);
#3649=EDGE_CURVE('',#2845,#2846,#1544,.T.);
#3650=EDGE_CURVE('',#2846,#2845,#1545,.T.);
#3651=EDGE_CURVE('',#2841,#2846,#2020,.T.);
#3652=EDGE_CURVE('',#2847,#2848,#1546,.T.);
#3653=EDGE_CURVE('',#2848,#2847,#1547,.T.);
#3654=EDGE_CURVE('',#2848,#2843,#2021,.T.);
#3655=EDGE_CURVE('',#2849,#2850,#1548,.T.);
#3656=EDGE_CURVE('',#2850,#2849,#1549,.T.);
#3657=EDGE_CURVE('',#2850,#2851,#2022,.T.);
#3658=EDGE_CURVE('',#2851,#2852,#1550,.T.);
#3659=EDGE_CURVE('',#2852,#2851,#1551,.T.);
#3660=EDGE_CURVE('',#2847,#2852,#2023,.T.);
#3661=EDGE_CURVE('',#2853,#2854,#1552,.T.);
#3662=EDGE_CURVE('',#2854,#2853,#1553,.T.);
#3663=EDGE_CURVE('',#2854,#2849,#2024,.T.);
#3664=EDGE_CURVE('',#2855,#2856,#1554,.T.);
#3665=EDGE_CURVE('',#2856,#2855,#1555,.T.);
#3666=EDGE_CURVE('',#2856,#2857,#2025,.T.);
#3667=EDGE_CURVE('',#2857,#2858,#1556,.T.);
#3668=EDGE_CURVE('',#2858,#2857,#1557,.T.);
#3669=EDGE_CURVE('',#2853,#2858,#2026,.T.);
#3670=EDGE_CURVE('',#2859,#2860,#1558,.T.);
#3671=EDGE_CURVE('',#2860,#2859,#1559,.T.);
#3672=EDGE_CURVE('',#2860,#2855,#2027,.T.);
#3673=EDGE_CURVE('',#2861,#2862,#1560,.T.);
#3674=EDGE_CURVE('',#2862,#2861,#1561,.T.);
#3675=EDGE_CURVE('',#2862,#2863,#2028,.T.);
#3676=EDGE_CURVE('',#2863,#2864,#1562,.T.);
#3677=EDGE_CURVE('',#2864,#2863,#1563,.T.);
#3678=EDGE_CURVE('',#2859,#2864,#2029,.T.);
#3679=EDGE_CURVE('',#2865,#2866,#1564,.T.);
#3680=EDGE_CURVE('',#2866,#2865,#1565,.T.);
#3681=EDGE_CURVE('',#2866,#2861,#2030,.T.);
#3682=EDGE_CURVE('',#2867,#2868,#1566,.T.);
#3683=EDGE_CURVE('',#2868,#2867,#1567,.T.);
#3684=EDGE_CURVE('',#2868,#2869,#2031,.T.);
#3685=EDGE_CURVE('',#2869,#2870,#1568,.T.);
#3686=EDGE_CURVE('',#2870,#2869,#1569,.T.);
#3687=EDGE_CURVE('',#2865,#2870,#2032,.T.);
#3688=EDGE_CURVE('',#2871,#2872,#1570,.T.);
#3689=EDGE_CURVE('',#2872,#2871,#1571,.T.);
#3690=EDGE_CURVE('',#2872,#2867,#2033,.T.);
#3691=EDGE_CURVE('',#2873,#2874,#1572,.T.);
#3692=EDGE_CURVE('',#2874,#2873,#1573,.T.);
#3693=EDGE_CURVE('',#2874,#2875,#2034,.T.);
#3694=EDGE_CURVE('',#2875,#2876,#1574,.T.);
#3695=EDGE_CURVE('',#2876,#2875,#1575,.T.);
#3696=EDGE_CURVE('',#2871,#2876,#2035,.T.);
#3697=EDGE_CURVE('',#2877,#2878,#1576,.T.);
#3698=EDGE_CURVE('',#2878,#2877,#1577,.T.);
#3699=EDGE_CURVE('',#2878,#2873,#2036,.T.);
#3700=EDGE_CURVE('',#2879,#2880,#1578,.T.);
#3701=EDGE_CURVE('',#2880,#2879,#1579,.T.);
#3702=EDGE_CURVE('',#2880,#2881,#2037,.T.);
#3703=EDGE_CURVE('',#2881,#2882,#1580,.T.);
#3704=EDGE_CURVE('',#2882,#2881,#1581,.T.);
#3705=EDGE_CURVE('',#2877,#2882,#2038,.T.);
#3706=EDGE_CURVE('',#2883,#2884,#1582,.T.);
#3707=EDGE_CURVE('',#2884,#2883,#1583,.T.);
#3708=EDGE_CURVE('',#2884,#2879,#2039,.T.);
#3709=EDGE_CURVE('',#2885,#2886,#1584,.T.);
#3710=EDGE_CURVE('',#2886,#2885,#1585,.T.);
#3711=EDGE_CURVE('',#2886,#2887,#2040,.T.);
#3712=EDGE_CURVE('',#2887,#2888,#1586,.T.);
#3713=EDGE_CURVE('',#2888,#2887,#1587,.T.);
#3714=EDGE_CURVE('',#2883,#2888,#2041,.T.);
#3715=EDGE_CURVE('',#2889,#2890,#1588,.T.);
#3716=EDGE_CURVE('',#2890,#2889,#1589,.T.);
#3717=EDGE_CURVE('',#2890,#2885,#2042,.T.);
#3718=EDGE_CURVE('',#2891,#2892,#1590,.T.);
#3719=EDGE_CURVE('',#2892,#2891,#1591,.T.);
#3720=EDGE_CURVE('',#2892,#2893,#2043,.T.);
#3721=EDGE_CURVE('',#2893,#2894,#1592,.T.);
#3722=EDGE_CURVE('',#2894,#2893,#1593,.T.);
#3723=EDGE_CURVE('',#2889,#2894,#2044,.T.);
#3724=EDGE_CURVE('',#2895,#2896,#1594,.T.);
#3725=EDGE_CURVE('',#2896,#2895,#1595,.T.);
#3726=EDGE_CURVE('',#2896,#2891,#2045,.T.);
#3727=EDGE_CURVE('',#2897,#2898,#1596,.T.);
#3728=EDGE_CURVE('',#2898,#2897,#1597,.T.);
#3729=EDGE_CURVE('',#2898,#2899,#2046,.T.);
#3730=EDGE_CURVE('',#2899,#2900,#1598,.T.);
#3731=EDGE_CURVE('',#2900,#2899,#1599,.T.);
#3732=EDGE_CURVE('',#2895,#2900,#2047,.T.);
#3733=EDGE_CURVE('',#2901,#2902,#1600,.T.);
#3734=EDGE_CURVE('',#2902,#2901,#1601,.T.);
#3735=EDGE_CURVE('',#2902,#2897,#2048,.T.);
#3736=EDGE_CURVE('',#2903,#2904,#1602,.T.);
#3737=EDGE_CURVE('',#2904,#2903,#1603,.T.);
#3738=EDGE_CURVE('',#2904,#2905,#2049,.T.);
#3739=EDGE_CURVE('',#2905,#2906,#1604,.T.);
#3740=EDGE_CURVE('',#2906,#2905,#1605,.T.);
#3741=EDGE_CURVE('',#2901,#2906,#2050,.T.);
#3742=EDGE_CURVE('',#2907,#2908,#1606,.T.);
#3743=EDGE_CURVE('',#2908,#2907,#1607,.T.);
#3744=EDGE_CURVE('',#2908,#2909,#1608,.T.);
#3745=EDGE_CURVE('',#2909,#2909,#1609,.T.);
#3746=EDGE_CURVE('',#2910,#2911,#1610,.T.);
#3747=EDGE_CURVE('',#2912,#2910,#1611,.T.);
#3748=EDGE_CURVE('',#2913,#2912,#1612,.T.);
#3749=EDGE_CURVE('',#2913,#2914,#2051,.T.);
#3750=EDGE_CURVE('',#2914,#2914,#1613,.T.);
#3751=EDGE_CURVE('',#2915,#2913,#1614,.T.);
#3752=EDGE_CURVE('',#2916,#2915,#1615,.T.);
#3753=EDGE_CURVE('',#2911,#2916,#1616,.T.);
#3754=EDGE_CURVE('',#2907,#2903,#2052,.T.);
#3755=EDGE_CURVE('',#2917,#2915,#2053,.T.);
#3756=EDGE_CURVE('',#2913,#2917,#2054,.T.);
#3757=EDGE_CURVE('',#2915,#2918,#2055,.T.);
#3758=EDGE_CURVE('',#2918,#2916,#2056,.T.);
#3759=EDGE_CURVE('',#2916,#2919,#2057,.T.);
#3760=EDGE_CURVE('',#2919,#2911,#2058,.T.);
#3761=EDGE_CURVE('',#2911,#2920,#2059,.T.);
#3762=EDGE_CURVE('',#2920,#2910,#2060,.T.);
#3763=EDGE_CURVE('',#2910,#2921,#2061,.T.);
#3764=EDGE_CURVE('',#2921,#2912,#2062,.T.);
#3765=EDGE_CURVE('',#2912,#2922,#2063,.T.);
#3766=EDGE_CURVE('',#2922,#2913,#2064,.T.);
#3767=EDGE_CURVE('',#2923,#2924,#1617,.T.);
#3768=EDGE_CURVE('',#2925,#2923,#1618,.T.);
#3769=EDGE_CURVE('',#2926,#2925,#1619,.T.);
#3770=EDGE_CURVE('',#2927,#2926,#1620,.T.);
#3771=EDGE_CURVE('',#2927,#2928,#1621,.T.);
#3772=EDGE_CURVE('',#2924,#2928,#1622,.T.);
#3773=EDGE_CURVE('',#2928,#2929,#237,.T.);
#3774=EDGE_CURVE('',#2929,#2924,#238,.T.);
#3775=EDGE_CURVE('',#2927,#2930,#239,.T.);
#3776=EDGE_CURVE('',#2930,#2928,#240,.T.);
#3777=EDGE_CURVE('',#2931,#2927,#241,.T.);
#3778=EDGE_CURVE('',#2926,#2931,#242,.T.);
#3779=EDGE_CURVE('',#2932,#2926,#243,.T.);
#3780=EDGE_CURVE('',#2925,#2932,#244,.T.);
#3781=EDGE_CURVE('',#2924,#2933,#245,.T.);
#3782=EDGE_CURVE('',#2933,#2923,#246,.T.);
#3783=EDGE_CURVE('',#2934,#2925,#247,.T.);
#3784=EDGE_CURVE('',#2923,#2934,#248,.T.);
#3785=EDGE_CURVE('',#2922,#2934,#2065,.T.);
#3786=EDGE_CURVE('',#2917,#2933,#2066,.T.);
#3787=EDGE_CURVE('',#2921,#2932,#2067,.T.);
#3788=EDGE_CURVE('',#2920,#2931,#2068,.T.);
#3789=EDGE_CURVE('',#2919,#2930,#2069,.T.);
#3790=EDGE_CURVE('',#2918,#2929,#2070,.T.);
#3791=EDGE_CURVE('',#2935,#2935,#1623,.T.);
#3792=EDGE_CURVE('',#2935,#2936,#2071,.T.);
#3793=EDGE_CURVE('',#2936,#2936,#1624,.T.);
#3794=EDGE_CURVE('',#2937,#2938,#1625,.T.);
#3795=EDGE_CURVE('',#2938,#2939,#2072,.T.);
#3796=EDGE_CURVE('',#2940,#2939,#1626,.T.);
#3797=EDGE_CURVE('',#2937,#2940,#2073,.T.);
#3798=EDGE_CURVE('',#2941,#2941,#1627,.T.);
#3799=EDGE_CURVE('',#2941,#2942,#2074,.T.);
#3800=EDGE_CURVE('',#2942,#2942,#1628,.T.);
#3801=EDGE_CURVE('',#2943,#2944,#2075,.T.);
#3802=EDGE_CURVE('',#2944,#2945,#2076,.T.);
#3803=EDGE_CURVE('',#2945,#2946,#2077,.T.);
#3804=EDGE_CURVE('',#2943,#2946,#2078,.T.);
#3805=EDGE_CURVE('',#2947,#2948,#2079,.T.);
#3806=EDGE_CURVE('',#2948,#2944,#2080,.T.);
#3807=EDGE_CURVE('',#2947,#2943,#2081,.T.);
#3808=EDGE_CURVE('',#2945,#2949,#2082,.T.);
#3809=EDGE_CURVE('',#2949,#2950,#2083,.T.);
#3810=EDGE_CURVE('',#2946,#2950,#2084,.T.);
#3811=EDGE_CURVE('',#2948,#2949,#2085,.T.);
#3812=EDGE_CURVE('',#2947,#2950,#2086,.T.);
#3813=EDGE_CURVE('',#2951,#2952,#1629,.T.);
#3814=EDGE_CURVE('',#2953,#2951,#2087,.T.);
#3815=EDGE_CURVE('',#2953,#2954,#1630,.T.);
#3816=EDGE_CURVE('',#2954,#2952,#2088,.T.);
#3817=EDGE_CURVE('',#2955,#2956,#2089,.T.);
#3818=EDGE_CURVE('',#2954,#2955,#2090,.T.);
#3819=EDGE_CURVE('',#2956,#2953,#2091,.T.);
#3820=EDGE_CURVE('',#2955,#2957,#2092,.T.);
#3821=EDGE_CURVE('',#2952,#2957,#2093,.T.);
#3822=EDGE_CURVE('',#2957,#2958,#2094,.T.);
#3823=EDGE_CURVE('',#2958,#2951,#2095,.T.);
#3824=EDGE_CURVE('',#2958,#2956,#2096,.T.);
#3825=EDGE_CURVE('',#2943,#2957,#1631,.T.);
#3826=EDGE_CURVE('',#2947,#2955,#1632,.T.);
#3827=EDGE_CURVE('',#2958,#2946,#1633,.T.);
#3828=EDGE_CURVE('',#2956,#2950,#1634,.T.);
#3829=EDGE_CURVE('',#2959,#2960,#2097,.T.);
#3830=EDGE_CURVE('',#2960,#2944,#1635,.T.);
#3831=EDGE_CURVE('',#2959,#2948,#1636,.T.);
#3832=EDGE_CURVE('',#2945,#2961,#1637,.T.);
#3833=EDGE_CURVE('',#2961,#2962,#2098,.T.);
#3834=EDGE_CURVE('',#2949,#2962,#1638,.T.);
#3835=EDGE_CURVE('',#2959,#2962,#2099,.T.);
#3836=EDGE_CURVE('',#2960,#2961,#2100,.T.);
#3837=EDGE_CURVE('',#2959,#2937,#2101,.T.);
#3838=EDGE_CURVE('',#2938,#2962,#2102,.T.);
#3839=EDGE_CURVE('',#2939,#2961,#2103,.T.);
#3840=EDGE_CURVE('',#2960,#2940,#2104,.T.);
#3841=EDGE_CURVE('',#2963,#2964,#1639,.T.);
#3842=EDGE_CURVE('',#2963,#2965,#1825,.T.);
#3843=EDGE_CURVE('',#2966,#2965,#1640,.T.);
#3844=EDGE_CURVE('',#2966,#2964,#1641,.T.);
#3845=EDGE_CURVE('',#2967,#2968,#1642,.T.);
#3846=EDGE_CURVE('',#2967,#2969,#1643,.T.);
#3847=EDGE_CURVE('',#2970,#2969,#1644,.T.);
#3848=EDGE_CURVE('',#2968,#2970,#1645,.T.);
#3849=EDGE_CURVE('',#2971,#2972,#1646,.T.);
#3850=EDGE_CURVE('',#2971,#2973,#1826,.T.);
#3851=EDGE_CURVE('',#2974,#2973,#1647,.T.);
#3852=EDGE_CURVE('',#2974,#2972,#1648,.T.);
#3853=EDGE_CURVE('',#2975,#2976,#1649,.T.);
#3854=EDGE_CURVE('',#2975,#2977,#1650,.T.);
#3855=EDGE_CURVE('',#2978,#2977,#1651,.T.);
#3856=EDGE_CURVE('',#2976,#2978,#1652,.T.);
#3857=EDGE_CURVE('',#2979,#2980,#1653,.T.);
#3858=EDGE_CURVE('',#2980,#2979,#1654,.T.);
#3859=EDGE_CURVE('',#2980,#2981,#2105,.T.);
#3860=EDGE_CURVE('',#2981,#2981,#1655,.T.);
#3861=EDGE_CURVE('',#2982,#2982,#1656,.T.);
#3862=EDGE_CURVE('',#2982,#2983,#2106,.T.);
#3863=EDGE_CURVE('',#2983,#2983,#1657,.T.);
#3864=EDGE_CURVE('',#2984,#2985,#1658,.T.);
#3865=EDGE_CURVE('',#2985,#2984,#1659,.T.);
#3866=EDGE_CURVE('',#2985,#2986,#2107,.T.);
#3867=EDGE_CURVE('',#2986,#2986,#1660,.T.);
#3868=EDGE_CURVE('',#2987,#2987,#1661,.T.);
#3869=EDGE_CURVE('',#2987,#2988,#2108,.T.);
#3870=EDGE_CURVE('',#2988,#2988,#1662,.T.);
#3871=EDGE_CURVE('',#2989,#2990,#1663,.T.);
#3872=EDGE_CURVE('',#2990,#2989,#1664,.T.);
#3873=EDGE_CURVE('',#2990,#2991,#2109,.T.);
#3874=EDGE_CURVE('',#2991,#2991,#1665,.T.);
#3875=EDGE_CURVE('',#2992,#2992,#1666,.T.);
#3876=EDGE_CURVE('',#2992,#2993,#2110,.T.);
#3877=EDGE_CURVE('',#2993,#2993,#1667,.T.);
#3878=EDGE_CURVE('',#2994,#2995,#1668,.T.);
#3879=EDGE_CURVE('',#2995,#2994,#1669,.T.);
#3880=EDGE_CURVE('',#2995,#2996,#2111,.T.);
#3881=EDGE_CURVE('',#2996,#2996,#1670,.T.);
#3882=EDGE_CURVE('',#2997,#2997,#1671,.T.);
#3883=EDGE_CURVE('',#2997,#2998,#2112,.T.);
#3884=EDGE_CURVE('',#2998,#2998,#1672,.T.);
#3885=EDGE_CURVE('',#2999,#3000,#1673,.T.);
#3886=EDGE_CURVE('',#3000,#2999,#1674,.T.);
#3887=EDGE_CURVE('',#3000,#3001,#2113,.T.);
#3888=EDGE_CURVE('',#3001,#3001,#1675,.T.);
#3889=EDGE_CURVE('',#3002,#3002,#1676,.T.);
#3890=EDGE_CURVE('',#3002,#3003,#2114,.T.);
#3891=EDGE_CURVE('',#3003,#3003,#1677,.T.);
#3892=EDGE_CURVE('',#2999,#3002,#2115,.T.);
#3893=EDGE_CURVE('',#2994,#2997,#2116,.T.);
#3894=EDGE_CURVE('',#2989,#2992,#2117,.T.);
#3895=EDGE_CURVE('',#2984,#2987,#2118,.T.);
#3896=EDGE_CURVE('',#2979,#2982,#2119,.T.);
#3897=EDGE_CURVE('',#3004,#3005,#1678,.T.);
#3898=EDGE_CURVE('',#3005,#3006,#2120,.T.);
#3899=EDGE_CURVE('',#3006,#3007,#1679,.T.);
#3900=EDGE_CURVE('',#3004,#3007,#2121,.T.);
#3901=EDGE_CURVE('',#3008,#3009,#1680,.T.);
#3902=EDGE_CURVE('',#3009,#3010,#2122,.T.);
#3903=EDGE_CURVE('',#3010,#3011,#1681,.T.);
#3904=EDGE_CURVE('',#3008,#3011,#2123,.T.);
#3905=EDGE_CURVE('',#3012,#2963,#2124,.T.);
#3906=EDGE_CURVE('',#2964,#3013,#2125,.T.);
#3907=EDGE_CURVE('',#3013,#3014,#1682,.T.);
#3908=EDGE_CURVE('',#3014,#2970,#2126,.T.);
#3909=EDGE_CURVE('',#2969,#3015,#1683,.T.);
#3910=EDGE_CURVE('',#3015,#3016,#2127,.T.);
#3911=EDGE_CURVE('',#3016,#3012,#1684,.T.);
#3912=EDGE_CURVE('',#3017,#2974,#2128,.T.);
#3913=EDGE_CURVE('',#2973,#3018,#2129,.T.);
#3914=EDGE_CURVE('',#3018,#3019,#1685,.T.);
#3915=EDGE_CURVE('',#3019,#3020,#2130,.T.);
#3916=EDGE_CURVE('',#3020,#2975,#1686,.T.);
#3917=EDGE_CURVE('',#2976,#3021,#2131,.T.);
#3918=EDGE_CURVE('',#3021,#3017,#1687,.T.);
#3919=EDGE_CURVE('',#2968,#2978,#2132,.T.);
#3920=EDGE_CURVE('',#2968,#3008,#2133,.T.);
#3921=EDGE_CURVE('',#3011,#2978,#2134,.T.);
#3922=EDGE_CURVE('',#2967,#2977,#2135,.T.);
#3923=EDGE_CURVE('',#2977,#3022,#1688,.T.);
#3924=EDGE_CURVE('',#3023,#3022,#2136,.T.);
#3925=EDGE_CURVE('',#3023,#2967,#1689,.T.);
#3926=EDGE_CURVE('',#3022,#3006,#2137,.T.);
#3927=EDGE_CURVE('',#3005,#3023,#2138,.T.);
#3928=EDGE_CURVE('',#3007,#2971,#2139,.T.);
#3929=EDGE_CURVE('',#2965,#2971,#2140,.T.);
#3930=EDGE_CURVE('',#2965,#3004,#2141,.T.);
#3931=EDGE_CURVE('',#2966,#2972,#2142,.T.);
#3932=EDGE_CURVE('',#2972,#3010,#2143,.T.);
#3933=EDGE_CURVE('',#3009,#2966,#2144,.T.);
#3934=EDGE_CURVE('',#3022,#3020,#1690,.T.);
#3935=EDGE_CURVE('',#3006,#3019,#1691,.T.);
#3936=EDGE_CURVE('',#3021,#3011,#1692,.T.);
#3937=EDGE_CURVE('',#3007,#3018,#1693,.T.);
#3938=EDGE_CURVE('',#3017,#3010,#1694,.T.);
#3939=EDGE_CURVE('',#3015,#3023,#1695,.T.);
#3940=EDGE_CURVE('',#3016,#3005,#1696,.T.);
#3941=EDGE_CURVE('',#3008,#3014,#1697,.T.);
#3942=EDGE_CURVE('',#3012,#3004,#1698,.T.);
#3943=EDGE_CURVE('',#3009,#3013,#1699,.T.);
#3944=ORIENTED_EDGE('',*,*,#3024,.T.);
#3945=ORIENTED_EDGE('',*,*,#3025,.T.);
#3946=ORIENTED_EDGE('',*,*,#3026,.F.);
#3947=ORIENTED_EDGE('',*,*,#3027,.T.);
#3948=ORIENTED_EDGE('',*,*,#3028,.T.);
#3949=ORIENTED_EDGE('',*,*,#3029,.T.);
#3950=ORIENTED_EDGE('',*,*,#3028,.F.);
#3951=ORIENTED_EDGE('',*,*,#3030,.T.);
#3952=ORIENTED_EDGE('',*,*,#3031,.T.);
#3953=ORIENTED_EDGE('',*,*,#3032,.T.);
#3954=ORIENTED_EDGE('',*,*,#3024,.F.);
#3955=ORIENTED_EDGE('',*,*,#3033,.T.);
#3956=ORIENTED_EDGE('',*,*,#3034,.T.);
#3957=ORIENTED_EDGE('',*,*,#3035,.T.);
#3958=ORIENTED_EDGE('',*,*,#3031,.F.);
#3959=ORIENTED_EDGE('',*,*,#3036,.T.);
#3960=ORIENTED_EDGE('',*,*,#3037,.T.);
#3961=ORIENTED_EDGE('',*,*,#3038,.T.);
#3962=ORIENTED_EDGE('',*,*,#3034,.F.);
#3963=ORIENTED_EDGE('',*,*,#3039,.T.);
#3964=ORIENTED_EDGE('',*,*,#3040,.T.);
#3965=ORIENTED_EDGE('',*,*,#3041,.T.);
#3966=ORIENTED_EDGE('',*,*,#3037,.F.);
#3967=ORIENTED_EDGE('',*,*,#3042,.T.);
#3968=ORIENTED_EDGE('',*,*,#3043,.T.);
#3969=ORIENTED_EDGE('',*,*,#3044,.T.);
#3970=ORIENTED_EDGE('',*,*,#3040,.F.);
#3971=ORIENTED_EDGE('',*,*,#3045,.T.);
#3972=ORIENTED_EDGE('',*,*,#3046,.T.);
#3973=ORIENTED_EDGE('',*,*,#3047,.T.);
#3974=ORIENTED_EDGE('',*,*,#3043,.F.);
#3975=ORIENTED_EDGE('',*,*,#3048,.T.);
#3976=ORIENTED_EDGE('',*,*,#3049,.T.);
#3977=ORIENTED_EDGE('',*,*,#3050,.T.);
#3978=ORIENTED_EDGE('',*,*,#3046,.F.);
#3979=ORIENTED_EDGE('',*,*,#3051,.T.);
#3980=ORIENTED_EDGE('',*,*,#3052,.T.);
#3981=ORIENTED_EDGE('',*,*,#3053,.T.);
#3982=ORIENTED_EDGE('',*,*,#3049,.F.);
#3983=ORIENTED_EDGE('',*,*,#3054,.T.);
#3984=ORIENTED_EDGE('',*,*,#3055,.T.);
#3985=ORIENTED_EDGE('',*,*,#3056,.T.);
#3986=ORIENTED_EDGE('',*,*,#3052,.F.);
#3987=ORIENTED_EDGE('',*,*,#3057,.T.);
#3988=ORIENTED_EDGE('',*,*,#3058,.T.);
#3989=ORIENTED_EDGE('',*,*,#3059,.T.);
#3990=ORIENTED_EDGE('',*,*,#3055,.F.);
#3991=ORIENTED_EDGE('',*,*,#3060,.T.);
#3992=ORIENTED_EDGE('',*,*,#3061,.T.);
#3993=ORIENTED_EDGE('',*,*,#3062,.T.);
#3994=ORIENTED_EDGE('',*,*,#3058,.F.);
#3995=ORIENTED_EDGE('',*,*,#3063,.T.);
#3996=ORIENTED_EDGE('',*,*,#3064,.T.);
#3997=ORIENTED_EDGE('',*,*,#3065,.T.);
#3998=ORIENTED_EDGE('',*,*,#3061,.F.);
#3999=ORIENTED_EDGE('',*,*,#3066,.T.);
#4000=ORIENTED_EDGE('',*,*,#3067,.T.);
#4001=ORIENTED_EDGE('',*,*,#3068,.T.);
#4002=ORIENTED_EDGE('',*,*,#3064,.F.);
#4003=ORIENTED_EDGE('',*,*,#3069,.T.);
#4004=ORIENTED_EDGE('',*,*,#3070,.T.);
#4005=ORIENTED_EDGE('',*,*,#3071,.T.);
#4006=ORIENTED_EDGE('',*,*,#3067,.F.);
#4007=ORIENTED_EDGE('',*,*,#3072,.T.);
#4008=ORIENTED_EDGE('',*,*,#3073,.T.);
#4009=ORIENTED_EDGE('',*,*,#3074,.T.);
#4010=ORIENTED_EDGE('',*,*,#3070,.F.);
#4011=ORIENTED_EDGE('',*,*,#3075,.T.);
#4012=ORIENTED_EDGE('',*,*,#3076,.T.);
#4013=ORIENTED_EDGE('',*,*,#3077,.T.);
#4014=ORIENTED_EDGE('',*,*,#3073,.F.);
#4015=ORIENTED_EDGE('',*,*,#3078,.T.);
#4016=ORIENTED_EDGE('',*,*,#3079,.T.);
#4017=ORIENTED_EDGE('',*,*,#3080,.T.);
#4018=ORIENTED_EDGE('',*,*,#3076,.F.);
#4019=ORIENTED_EDGE('',*,*,#3081,.T.);
#4020=ORIENTED_EDGE('',*,*,#3082,.T.);
#4021=ORIENTED_EDGE('',*,*,#3083,.T.);
#4022=ORIENTED_EDGE('',*,*,#3079,.F.);
#4023=ORIENTED_EDGE('',*,*,#3084,.T.);
#4024=ORIENTED_EDGE('',*,*,#3085,.T.);
#4025=ORIENTED_EDGE('',*,*,#3086,.T.);
#4026=ORIENTED_EDGE('',*,*,#3082,.F.);
#4027=ORIENTED_EDGE('',*,*,#3087,.T.);
#4028=ORIENTED_EDGE('',*,*,#3088,.T.);
#4029=ORIENTED_EDGE('',*,*,#3089,.T.);
#4030=ORIENTED_EDGE('',*,*,#3085,.F.);
#4031=ORIENTED_EDGE('',*,*,#3090,.T.);
#4032=ORIENTED_EDGE('',*,*,#3091,.F.);
#4033=ORIENTED_EDGE('',*,*,#3092,.T.);
#4034=ORIENTED_EDGE('',*,*,#3093,.T.);
#4035=ORIENTED_EDGE('',*,*,#3094,.T.);
#4036=ORIENTED_EDGE('',*,*,#3095,.F.);
#4037=ORIENTED_EDGE('',*,*,#3096,.F.);
#4038=ORIENTED_EDGE('',*,*,#3097,.T.);
#4039=ORIENTED_EDGE('',*,*,#3098,.F.);
#4040=ORIENTED_EDGE('',*,*,#3097,.F.);
#4041=ORIENTED_EDGE('',*,*,#3099,.F.);
#4042=ORIENTED_EDGE('',*,*,#3100,.T.);
#4043=ORIENTED_EDGE('',*,*,#3101,.F.);
#4044=ORIENTED_EDGE('',*,*,#3102,.F.);
#4045=ORIENTED_EDGE('',*,*,#3100,.F.);
#4046=ORIENTED_EDGE('',*,*,#3103,.F.);
#4047=ORIENTED_EDGE('',*,*,#3104,.F.);
#4048=ORIENTED_EDGE('',*,*,#3105,.F.);
#4049=ORIENTED_EDGE('',*,*,#3106,.T.);
#4050=ORIENTED_EDGE('',*,*,#3107,.T.);
#4051=ORIENTED_EDGE('',*,*,#3108,.F.);
#4052=ORIENTED_EDGE('',*,*,#3109,.F.);
#4053=ORIENTED_EDGE('',*,*,#3110,.F.);
#4054=ORIENTED_EDGE('',*,*,#3111,.F.);
#4055=ORIENTED_EDGE('',*,*,#3105,.T.);
#4056=ORIENTED_EDGE('',*,*,#3112,.F.);
#4057=ORIENTED_EDGE('',*,*,#3113,.F.);
#4058=ORIENTED_EDGE('',*,*,#3114,.F.);
#4059=ORIENTED_EDGE('',*,*,#3115,.T.);
#4060=ORIENTED_EDGE('',*,*,#3116,.F.);
#4061=ORIENTED_EDGE('',*,*,#3117,.T.);
#4062=ORIENTED_EDGE('',*,*,#3118,.F.);
#4063=ORIENTED_EDGE('',*,*,#3119,.T.);
#4064=ORIENTED_EDGE('',*,*,#3120,.T.);
#4065=ORIENTED_EDGE('',*,*,#3121,.F.);
#4066=ORIENTED_EDGE('',*,*,#3122,.F.);
#4067=ORIENTED_EDGE('',*,*,#3123,.F.);
#4068=ORIENTED_EDGE('',*,*,#3029,.F.);
#4069=ORIENTED_EDGE('',*,*,#3124,.T.);
#4070=ORIENTED_EDGE('',*,*,#3125,.F.);
#4071=ORIENTED_EDGE('',*,*,#3124,.F.);
#4072=ORIENTED_EDGE('',*,*,#3126,.T.);
#4073=ORIENTED_EDGE('',*,*,#3127,.T.);
#4074=ORIENTED_EDGE('',*,*,#3128,.F.);
#4075=ORIENTED_EDGE('',*,*,#3129,.T.);
#4076=ORIENTED_EDGE('',*,*,#3130,.T.);
#4077=ORIENTED_EDGE('',*,*,#3131,.F.);
#4078=ORIENTED_EDGE('',*,*,#3132,.T.);
#4079=ORIENTED_EDGE('',*,*,#3133,.F.);
#4080=ORIENTED_EDGE('',*,*,#3134,.T.);
#4081=ORIENTED_EDGE('',*,*,#3135,.F.);
#4082=ORIENTED_EDGE('',*,*,#3136,.F.);
#4083=ORIENTED_EDGE('',*,*,#3137,.T.);
#4084=ORIENTED_EDGE('',*,*,#3138,.F.);
#4085=ORIENTED_EDGE('',*,*,#3139,.T.);
#4086=ORIENTED_EDGE('',*,*,#3140,.F.);
#4087=ORIENTED_EDGE('',*,*,#3141,.T.);
#4088=ORIENTED_EDGE('',*,*,#3091,.T.);
#4089=ORIENTED_EDGE('',*,*,#3142,.T.);
#4090=ORIENTED_EDGE('',*,*,#3088,.F.);
#4091=ORIENTED_EDGE('',*,*,#3143,.T.);
#4092=ORIENTED_EDGE('',*,*,#3144,.T.);
#4093=ORIENTED_EDGE('',*,*,#3145,.T.);
#4094=ORIENTED_EDGE('',*,*,#3146,.F.);
#4095=ORIENTED_EDGE('',*,*,#3145,.F.);
#4096=ORIENTED_EDGE('',*,*,#3147,.T.);
#4097=ORIENTED_EDGE('',*,*,#3148,.T.);
#4098=ORIENTED_EDGE('',*,*,#3149,.F.);
#4099=ORIENTED_EDGE('',*,*,#3148,.F.);
#4100=ORIENTED_EDGE('',*,*,#3150,.T.);
#4101=ORIENTED_EDGE('',*,*,#3151,.T.);
#4102=ORIENTED_EDGE('',*,*,#3152,.F.);
#4103=ORIENTED_EDGE('',*,*,#3151,.F.);
#4104=ORIENTED_EDGE('',*,*,#3095,.T.);
#4105=ORIENTED_EDGE('',*,*,#3096,.T.);
#4106=ORIENTED_EDGE('',*,*,#3153,.T.);
#4107=ORIENTED_EDGE('',*,*,#3135,.T.);
#4108=ORIENTED_EDGE('',*,*,#3154,.T.);
#4109=ORIENTED_EDGE('',*,*,#3155,.T.);
#4110=ORIENTED_EDGE('',*,*,#3156,.T.);
#4111=ORIENTED_EDGE('',*,*,#3101,.T.);
#4112=ORIENTED_EDGE('',*,*,#3102,.T.);
#4113=ORIENTED_EDGE('',*,*,#3156,.F.);
#4114=ORIENTED_EDGE('',*,*,#3157,.T.);
#4115=ORIENTED_EDGE('',*,*,#3158,.T.);
#4116=ORIENTED_EDGE('',*,*,#3136,.T.);
#4117=ORIENTED_EDGE('',*,*,#3153,.F.);
#4118=ORIENTED_EDGE('',*,*,#3128,.T.);
#4119=ORIENTED_EDGE('',*,*,#3159,.T.);
#4120=ORIENTED_EDGE('',*,*,#3160,.T.);
#4121=ORIENTED_EDGE('',*,*,#3161,.T.);
#4122=ORIENTED_EDGE('',*,*,#3162,.T.);
#4123=ORIENTED_EDGE('',*,*,#3140,.T.);
#4124=ORIENTED_EDGE('',*,*,#3163,.T.);
#4125=ORIENTED_EDGE('',*,*,#3164,.T.);
#4126=ORIENTED_EDGE('',*,*,#3165,.T.);
#4127=ORIENTED_EDGE('',*,*,#3166,.T.);
#4128=ORIENTED_EDGE('',*,*,#3167,.T.);
#4129=ORIENTED_EDGE('',*,*,#3168,.T.);
#4130=ORIENTED_EDGE('',*,*,#3169,.T.);
#4131=ORIENTED_EDGE('',*,*,#3170,.T.);
#4132=ORIENTED_EDGE('',*,*,#3125,.T.);
#4133=ORIENTED_EDGE('',*,*,#3171,.T.);
#4134=ORIENTED_EDGE('',*,*,#3172,.T.);
#4135=ORIENTED_EDGE('',*,*,#3173,.T.);
#4136=ORIENTED_EDGE('',*,*,#3174,.T.);
#4137=ORIENTED_EDGE('',*,*,#3175,.T.);
#4138=ORIENTED_EDGE('',*,*,#3176,.T.);
#4139=ORIENTED_EDGE('',*,*,#3177,.T.);
#4140=ORIENTED_EDGE('',*,*,#3178,.T.);
#4141=ORIENTED_EDGE('',*,*,#3179,.T.);
#4142=ORIENTED_EDGE('',*,*,#3180,.T.);
#4143=ORIENTED_EDGE('',*,*,#3181,.T.);
#4144=ORIENTED_EDGE('',*,*,#3182,.T.);
#4145=ORIENTED_EDGE('',*,*,#3183,.T.);
#4146=ORIENTED_EDGE('',*,*,#3184,.T.);
#4147=ORIENTED_EDGE('',*,*,#3185,.T.);
#4148=ORIENTED_EDGE('',*,*,#3186,.T.);
#4149=ORIENTED_EDGE('',*,*,#3187,.T.);
#4150=ORIENTED_EDGE('',*,*,#3188,.T.);
#4151=ORIENTED_EDGE('',*,*,#3189,.T.);
#4152=ORIENTED_EDGE('',*,*,#3190,.T.);
#4153=ORIENTED_EDGE('',*,*,#3191,.T.);
#4154=ORIENTED_EDGE('',*,*,#3192,.T.);
#4155=ORIENTED_EDGE('',*,*,#3193,.T.);
#4156=ORIENTED_EDGE('',*,*,#3194,.T.);
#4157=ORIENTED_EDGE('',*,*,#3195,.T.);
#4158=ORIENTED_EDGE('',*,*,#3196,.T.);
#4159=ORIENTED_EDGE('',*,*,#3197,.T.);
#4160=ORIENTED_EDGE('',*,*,#3198,.T.);
#4161=ORIENTED_EDGE('',*,*,#3199,.T.);
#4162=ORIENTED_EDGE('',*,*,#3200,.T.);
#4163=ORIENTED_EDGE('',*,*,#3098,.T.);
#4164=ORIENTED_EDGE('',*,*,#3201,.F.);
#4165=ORIENTED_EDGE('',*,*,#3202,.F.);
#4166=ORIENTED_EDGE('',*,*,#3203,.T.);
#4167=ORIENTED_EDGE('',*,*,#3204,.T.);
#4168=ORIENTED_EDGE('',*,*,#3205,.T.);
#4169=ORIENTED_EDGE('',*,*,#3203,.F.);
#4170=ORIENTED_EDGE('',*,*,#3206,.T.);
#4171=ORIENTED_EDGE('',*,*,#3207,.T.);
#4172=ORIENTED_EDGE('',*,*,#3093,.F.);
#4173=ORIENTED_EDGE('',*,*,#3208,.T.);
#4174=ORIENTED_EDGE('',*,*,#3209,.T.);
#4175=ORIENTED_EDGE('',*,*,#3210,.T.);
#4176=ORIENTED_EDGE('',*,*,#3211,.T.);
#4177=ORIENTED_EDGE('',*,*,#3212,.T.);
#4178=ORIENTED_EDGE('',*,*,#3213,.T.);
#4179=ORIENTED_EDGE('',*,*,#3150,.F.);
#4180=ORIENTED_EDGE('',*,*,#3214,.T.);
#4181=ORIENTED_EDGE('',*,*,#3215,.T.);
#4182=ORIENTED_EDGE('',*,*,#3216,.T.);
#4183=ORIENTED_EDGE('',*,*,#3217,.T.);
#4184=ORIENTED_EDGE('',*,*,#3218,.T.);
#4185=ORIENTED_EDGE('',*,*,#3219,.T.);
#4186=ORIENTED_EDGE('',*,*,#3152,.T.);
#4187=ORIENTED_EDGE('',*,*,#3220,.F.);
#4188=ORIENTED_EDGE('',*,*,#3221,.T.);
#4189=ORIENTED_EDGE('',*,*,#3222,.T.);
#4190=ORIENTED_EDGE('',*,*,#3223,.T.);
#4191=ORIENTED_EDGE('',*,*,#3224,.F.);
#4192=ORIENTED_EDGE('',*,*,#3225,.T.);
#4193=ORIENTED_EDGE('',*,*,#3220,.T.);
#4194=ORIENTED_EDGE('',*,*,#3226,.T.);
#4195=ORIENTED_EDGE('',*,*,#3227,.F.);
#4196=ORIENTED_EDGE('',*,*,#3228,.T.);
#4197=ORIENTED_EDGE('',*,*,#3224,.T.);
#4198=ORIENTED_EDGE('',*,*,#3229,.T.);
#4199=ORIENTED_EDGE('',*,*,#3230,.F.);
#4200=ORIENTED_EDGE('',*,*,#3231,.T.);
#4201=ORIENTED_EDGE('',*,*,#3227,.T.);
#4202=ORIENTED_EDGE('',*,*,#3232,.T.);
#4203=ORIENTED_EDGE('',*,*,#3233,.T.);
#4204=ORIENTED_EDGE('',*,*,#3234,.T.);
#4205=ORIENTED_EDGE('',*,*,#3235,.T.);
#4206=ORIENTED_EDGE('',*,*,#3230,.T.);
#4207=ORIENTED_EDGE('',*,*,#3138,.T.);
#4208=ORIENTED_EDGE('',*,*,#3236,.T.);
#4209=ORIENTED_EDGE('',*,*,#3237,.T.);
#4210=ORIENTED_EDGE('',*,*,#3238,.T.);
#4211=ORIENTED_EDGE('',*,*,#3239,.T.);
#4212=ORIENTED_EDGE('',*,*,#3240,.T.);
#4213=ORIENTED_EDGE('',*,*,#3241,.T.);
#4214=ORIENTED_EDGE('',*,*,#3242,.T.);
#4215=ORIENTED_EDGE('',*,*,#3243,.T.);
#4216=ORIENTED_EDGE('',*,*,#3244,.T.);
#4217=ORIENTED_EDGE('',*,*,#3245,.T.);
#4218=ORIENTED_EDGE('',*,*,#3246,.T.);
#4219=ORIENTED_EDGE('',*,*,#3247,.T.);
#4220=ORIENTED_EDGE('',*,*,#3248,.T.);
#4221=ORIENTED_EDGE('',*,*,#3147,.F.);
#4222=ORIENTED_EDGE('',*,*,#3249,.F.);
#4223=ORIENTED_EDGE('',*,*,#3250,.T.);
#4224=ORIENTED_EDGE('',*,*,#3251,.T.);
#4225=ORIENTED_EDGE('',*,*,#3252,.T.);
#4226=ORIENTED_EDGE('',*,*,#3249,.T.);
#4227=ORIENTED_EDGE('',*,*,#3253,.T.);
#4228=ORIENTED_EDGE('',*,*,#3254,.F.);
#4229=ORIENTED_EDGE('',*,*,#3255,.T.);
#4230=ORIENTED_EDGE('',*,*,#3254,.T.);
#4231=ORIENTED_EDGE('',*,*,#3108,.T.);
#4232=ORIENTED_EDGE('',*,*,#3256,.F.);
#4233=ORIENTED_EDGE('',*,*,#3257,.T.);
#4234=ORIENTED_EDGE('',*,*,#3256,.T.);
#4235=ORIENTED_EDGE('',*,*,#3258,.T.);
#4236=ORIENTED_EDGE('',*,*,#3259,.F.);
#4237=ORIENTED_EDGE('',*,*,#3260,.T.);
#4238=ORIENTED_EDGE('',*,*,#3112,.T.);
#4239=ORIENTED_EDGE('',*,*,#3261,.T.);
#4240=ORIENTED_EDGE('',*,*,#3262,.T.);
#4241=ORIENTED_EDGE('',*,*,#3259,.T.);
#4242=ORIENTED_EDGE('',*,*,#3133,.T.);
#4243=ORIENTED_EDGE('',*,*,#3263,.T.);
#4244=ORIENTED_EDGE('',*,*,#3264,.T.);
#4245=ORIENTED_EDGE('',*,*,#3265,.T.);
#4246=ORIENTED_EDGE('',*,*,#3266,.T.);
#4247=ORIENTED_EDGE('',*,*,#3103,.T.);
#4248=ORIENTED_EDGE('',*,*,#3267,.T.);
#4249=ORIENTED_EDGE('',*,*,#3268,.T.);
#4250=ORIENTED_EDGE('',*,*,#3269,.T.);
#4251=ORIENTED_EDGE('',*,*,#3270,.T.);
#4252=ORIENTED_EDGE('',*,*,#3114,.T.);
#4253=ORIENTED_EDGE('',*,*,#3111,.T.);
#4254=ORIENTED_EDGE('',*,*,#3271,.T.);
#4255=ORIENTED_EDGE('',*,*,#3272,.T.);
#4256=ORIENTED_EDGE('',*,*,#3149,.T.);
#4257=ORIENTED_EDGE('',*,*,#3118,.T.);
#4258=ORIENTED_EDGE('',*,*,#3273,.T.);
#4259=ORIENTED_EDGE('',*,*,#3274,.T.);
#4260=ORIENTED_EDGE('',*,*,#3275,.T.);
#4261=ORIENTED_EDGE('',*,*,#3276,.T.);
#4262=ORIENTED_EDGE('',*,*,#3123,.T.);
#4263=ORIENTED_EDGE('',*,*,#3144,.F.);
#4264=ORIENTED_EDGE('',*,*,#3277,.F.);
#4265=ORIENTED_EDGE('',*,*,#3278,.T.);
#4266=ORIENTED_EDGE('',*,*,#3131,.T.);
#4267=ORIENTED_EDGE('',*,*,#3279,.T.);
#4268=ORIENTED_EDGE('',*,*,#3277,.T.);
#4269=ORIENTED_EDGE('',*,*,#3280,.T.);
#4270=ORIENTED_EDGE('',*,*,#3281,.F.);
#4271=ORIENTED_EDGE('',*,*,#3282,.T.);
#4272=ORIENTED_EDGE('',*,*,#3281,.T.);
#4273=ORIENTED_EDGE('',*,*,#3283,.T.);
#4274=ORIENTED_EDGE('',*,*,#3284,.F.);
#4275=ORIENTED_EDGE('',*,*,#3121,.T.);
#4276=ORIENTED_EDGE('',*,*,#3284,.T.);
#4277=ORIENTED_EDGE('',*,*,#3285,.T.);
#4278=ORIENTED_EDGE('',*,*,#3286,.F.);
#4279=ORIENTED_EDGE('',*,*,#3287,.T.);
#4280=ORIENTED_EDGE('',*,*,#3288,.T.);
#4281=ORIENTED_EDGE('',*,*,#3289,.T.);
#4282=ORIENTED_EDGE('',*,*,#3116,.T.);
#4283=ORIENTED_EDGE('',*,*,#3286,.T.);
#4284=ORIENTED_EDGE('',*,*,#3290,.T.);
#4285=ORIENTED_EDGE('',*,*,#3291,.T.);
#4286=ORIENTED_EDGE('',*,*,#3292,.T.);
#4287=ORIENTED_EDGE('',*,*,#3293,.T.);
#4288=ORIENTED_EDGE('',*,*,#3294,.T.);
#4289=ORIENTED_EDGE('',*,*,#3295,.T.);
#4290=ORIENTED_EDGE('',*,*,#3296,.T.);
#4291=ORIENTED_EDGE('',*,*,#3297,.T.);
#4292=ORIENTED_EDGE('',*,*,#3298,.T.);
#4293=ORIENTED_EDGE('',*,*,#3299,.T.);
#4294=ORIENTED_EDGE('',*,*,#3300,.T.);
#4295=ORIENTED_EDGE('',*,*,#3301,.T.);
#4296=ORIENTED_EDGE('',*,*,#3302,.T.);
#4297=ORIENTED_EDGE('',*,*,#3303,.T.);
#4298=ORIENTED_EDGE('',*,*,#3146,.T.);
#4299=ORIENTED_EDGE('',*,*,#3163,.F.);
#4300=ORIENTED_EDGE('',*,*,#3304,.T.);
#4301=ORIENTED_EDGE('',*,*,#3305,.T.);
#4302=ORIENTED_EDGE('',*,*,#3214,.F.);
#4303=ORIENTED_EDGE('',*,*,#3306,.T.);
#4304=ORIENTED_EDGE('',*,*,#3307,.T.);
#4305=ORIENTED_EDGE('',*,*,#3308,.T.);
#4306=ORIENTED_EDGE('',*,*,#3159,.F.);
#4307=ORIENTED_EDGE('',*,*,#3309,.T.);
#4308=ORIENTED_EDGE('',*,*,#3274,.F.);
#4309=ORIENTED_EDGE('',*,*,#3161,.F.);
#4310=ORIENTED_EDGE('',*,*,#3310,.T.);
#4311=ORIENTED_EDGE('',*,*,#3311,.T.);
#4312=ORIENTED_EDGE('',*,*,#3298,.F.);
#4313=ORIENTED_EDGE('',*,*,#3312,.T.);
#4314=ORIENTED_EDGE('',*,*,#3313,.T.);
#4315=ORIENTED_EDGE('',*,*,#3314,.T.);
#4316=ORIENTED_EDGE('',*,*,#3158,.F.);
#4317=ORIENTED_EDGE('',*,*,#3315,.T.);
#4318=ORIENTED_EDGE('',*,*,#3245,.F.);
#4319=ORIENTED_EDGE('',*,*,#3154,.F.);
#4320=ORIENTED_EDGE('',*,*,#3316,.T.);
#4321=ORIENTED_EDGE('',*,*,#3317,.T.);
#4322=ORIENTED_EDGE('',*,*,#3269,.F.);
#4323=ORIENTED_EDGE('',*,*,#3318,.T.);
#4324=ORIENTED_EDGE('',*,*,#3319,.T.);
#4325=ORIENTED_EDGE('',*,*,#3320,.T.);
#4326=ORIENTED_EDGE('',*,*,#3162,.F.);
#4327=ORIENTED_EDGE('',*,*,#3321,.T.);
#4328=ORIENTED_EDGE('',*,*,#3210,.F.);
#4329=ORIENTED_EDGE('',*,*,#3160,.F.);
#4330=ORIENTED_EDGE('',*,*,#3322,.T.);
#4331=ORIENTED_EDGE('',*,*,#3290,.F.);
#4332=ORIENTED_EDGE('',*,*,#3323,.T.);
#4333=ORIENTED_EDGE('',*,*,#3155,.F.);
#4334=ORIENTED_EDGE('',*,*,#3324,.T.);
#4335=ORIENTED_EDGE('',*,*,#3325,.T.);
#4336=ORIENTED_EDGE('',*,*,#3251,.F.);
#4337=ORIENTED_EDGE('',*,*,#3326,.T.);
#4338=ORIENTED_EDGE('',*,*,#3327,.T.);
#4339=ORIENTED_EDGE('',*,*,#3157,.F.);
#4340=ORIENTED_EDGE('',*,*,#3328,.T.);
#4341=ORIENTED_EDGE('',*,*,#3329,.T.);
#4342=ORIENTED_EDGE('',*,*,#3164,.F.);
#4343=ORIENTED_EDGE('',*,*,#3330,.T.);
#4344=ORIENTED_EDGE('',*,*,#3331,.T.);
#4345=ORIENTED_EDGE('',*,*,#3222,.F.);
#4346=ORIENTED_EDGE('',*,*,#3026,.T.);
#4347=ORIENTED_EDGE('',*,*,#3332,.F.);
#4348=ORIENTED_EDGE('',*,*,#3333,.F.);
#4349=ORIENTED_EDGE('',*,*,#3334,.F.);
#4350=ORIENTED_EDGE('',*,*,#3335,.F.);
#4351=ORIENTED_EDGE('',*,*,#3201,.T.);
#4352=ORIENTED_EDGE('',*,*,#3205,.F.);
#4353=ORIENTED_EDGE('',*,*,#3336,.T.);
#4354=ORIENTED_EDGE('',*,*,#3334,.T.);
#4355=ORIENTED_EDGE('',*,*,#3337,.F.);
#4356=ORIENTED_EDGE('',*,*,#3335,.T.);
#4357=ORIENTED_EDGE('',*,*,#3336,.F.);
#4358=ORIENTED_EDGE('',*,*,#3204,.F.);
#4359=ORIENTED_EDGE('',*,*,#3092,.F.);
#4360=ORIENTED_EDGE('',*,*,#3143,.F.);
#4361=ORIENTED_EDGE('',*,*,#3090,.F.);
#4362=ORIENTED_EDGE('',*,*,#3087,.F.);
#4363=ORIENTED_EDGE('',*,*,#3084,.F.);
#4364=ORIENTED_EDGE('',*,*,#3081,.F.);
#4365=ORIENTED_EDGE('',*,*,#3078,.F.);
#4366=ORIENTED_EDGE('',*,*,#3075,.F.);
#4367=ORIENTED_EDGE('',*,*,#3072,.F.);
#4368=ORIENTED_EDGE('',*,*,#3069,.F.);
#4369=ORIENTED_EDGE('',*,*,#3066,.F.);
#4370=ORIENTED_EDGE('',*,*,#3063,.F.);
#4371=ORIENTED_EDGE('',*,*,#3060,.F.);
#4372=ORIENTED_EDGE('',*,*,#3057,.F.);
#4373=ORIENTED_EDGE('',*,*,#3054,.F.);
#4374=ORIENTED_EDGE('',*,*,#3051,.F.);
#4375=ORIENTED_EDGE('',*,*,#3048,.F.);
#4376=ORIENTED_EDGE('',*,*,#3045,.F.);
#4377=ORIENTED_EDGE('',*,*,#3042,.F.);
#4378=ORIENTED_EDGE('',*,*,#3039,.F.);
#4379=ORIENTED_EDGE('',*,*,#3036,.F.);
#4380=ORIENTED_EDGE('',*,*,#3033,.F.);
#4381=ORIENTED_EDGE('',*,*,#3030,.F.);
#4382=ORIENTED_EDGE('',*,*,#3027,.F.);
#4383=ORIENTED_EDGE('',*,*,#3202,.T.);
#4384=ORIENTED_EDGE('',*,*,#3337,.T.);
#4385=ORIENTED_EDGE('',*,*,#3333,.T.);
#4386=ORIENTED_EDGE('',*,*,#3338,.F.);
#4387=ORIENTED_EDGE('',*,*,#3206,.F.);
#4388=ORIENTED_EDGE('',*,*,#3207,.F.);
#4389=ORIENTED_EDGE('',*,*,#3338,.T.);
#4390=ORIENTED_EDGE('',*,*,#3332,.T.);
#4391=ORIENTED_EDGE('',*,*,#3025,.F.);
#4392=ORIENTED_EDGE('',*,*,#3032,.F.);
#4393=ORIENTED_EDGE('',*,*,#3035,.F.);
#4394=ORIENTED_EDGE('',*,*,#3038,.F.);
#4395=ORIENTED_EDGE('',*,*,#3041,.F.);
#4396=ORIENTED_EDGE('',*,*,#3044,.F.);
#4397=ORIENTED_EDGE('',*,*,#3047,.F.);
#4398=ORIENTED_EDGE('',*,*,#3050,.F.);
#4399=ORIENTED_EDGE('',*,*,#3053,.F.);
#4400=ORIENTED_EDGE('',*,*,#3056,.F.);
#4401=ORIENTED_EDGE('',*,*,#3059,.F.);
#4402=ORIENTED_EDGE('',*,*,#3062,.F.);
#4403=ORIENTED_EDGE('',*,*,#3065,.F.);
#4404=ORIENTED_EDGE('',*,*,#3068,.F.);
#4405=ORIENTED_EDGE('',*,*,#3071,.F.);
#4406=ORIENTED_EDGE('',*,*,#3074,.F.);
#4407=ORIENTED_EDGE('',*,*,#3077,.F.);
#4408=ORIENTED_EDGE('',*,*,#3080,.F.);
#4409=ORIENTED_EDGE('',*,*,#3083,.F.);
#4410=ORIENTED_EDGE('',*,*,#3086,.F.);
#4411=ORIENTED_EDGE('',*,*,#3089,.F.);
#4412=ORIENTED_EDGE('',*,*,#3142,.F.);
#4413=ORIENTED_EDGE('',*,*,#3094,.F.);
#4414=ORIENTED_EDGE('',*,*,#3099,.T.);
#4415=ORIENTED_EDGE('',*,*,#3339,.T.);
#4416=ORIENTED_EDGE('',*,*,#3340,.T.);
#4417=ORIENTED_EDGE('',*,*,#3341,.T.);
#4418=ORIENTED_EDGE('',*,*,#3342,.T.);
#4419=ORIENTED_EDGE('',*,*,#3343,.T.);
#4420=ORIENTED_EDGE('',*,*,#3344,.T.);
#4421=ORIENTED_EDGE('',*,*,#3345,.T.);
#4422=ORIENTED_EDGE('',*,*,#3346,.T.);
#4423=ORIENTED_EDGE('',*,*,#3347,.T.);
#4424=ORIENTED_EDGE('',*,*,#3348,.T.);
#4425=ORIENTED_EDGE('',*,*,#3349,.T.);
#4426=ORIENTED_EDGE('',*,*,#3350,.T.);
#4427=ORIENTED_EDGE('',*,*,#3174,.F.);
#4428=ORIENTED_EDGE('',*,*,#3351,.T.);
#4429=ORIENTED_EDGE('',*,*,#3200,.F.);
#4430=ORIENTED_EDGE('',*,*,#3166,.F.);
#4431=ORIENTED_EDGE('',*,*,#3199,.F.);
#4432=ORIENTED_EDGE('',*,*,#3352,.T.);
#4433=ORIENTED_EDGE('',*,*,#3195,.F.);
#4434=ORIENTED_EDGE('',*,*,#3167,.F.);
#4435=ORIENTED_EDGE('',*,*,#3194,.F.);
#4436=ORIENTED_EDGE('',*,*,#3353,.T.);
#4437=ORIENTED_EDGE('',*,*,#3190,.F.);
#4438=ORIENTED_EDGE('',*,*,#3168,.F.);
#4439=ORIENTED_EDGE('',*,*,#3189,.F.);
#4440=ORIENTED_EDGE('',*,*,#3354,.T.);
#4441=ORIENTED_EDGE('',*,*,#3185,.F.);
#4442=ORIENTED_EDGE('',*,*,#3169,.F.);
#4443=ORIENTED_EDGE('',*,*,#3184,.F.);
#4444=ORIENTED_EDGE('',*,*,#3355,.T.);
#4445=ORIENTED_EDGE('',*,*,#3180,.F.);
#4446=ORIENTED_EDGE('',*,*,#3170,.F.);
#4447=ORIENTED_EDGE('',*,*,#3179,.F.);
#4448=ORIENTED_EDGE('',*,*,#3356,.T.);
#4449=ORIENTED_EDGE('',*,*,#3175,.F.);
#4450=ORIENTED_EDGE('',*,*,#3165,.F.);
#4451=ORIENTED_EDGE('',*,*,#3183,.F.);
#4452=ORIENTED_EDGE('',*,*,#3357,.T.);
#4453=ORIENTED_EDGE('',*,*,#3176,.F.);
#4454=ORIENTED_EDGE('',*,*,#3355,.F.);
#4455=ORIENTED_EDGE('',*,*,#3188,.F.);
#4456=ORIENTED_EDGE('',*,*,#3358,.T.);
#4457=ORIENTED_EDGE('',*,*,#3181,.F.);
#4458=ORIENTED_EDGE('',*,*,#3354,.F.);
#4459=ORIENTED_EDGE('',*,*,#3193,.F.);
#4460=ORIENTED_EDGE('',*,*,#3359,.T.);
#4461=ORIENTED_EDGE('',*,*,#3186,.F.);
#4462=ORIENTED_EDGE('',*,*,#3353,.F.);
#4463=ORIENTED_EDGE('',*,*,#3198,.F.);
#4464=ORIENTED_EDGE('',*,*,#3360,.T.);
#4465=ORIENTED_EDGE('',*,*,#3191,.F.);
#4466=ORIENTED_EDGE('',*,*,#3352,.F.);
#4467=ORIENTED_EDGE('',*,*,#3173,.F.);
#4468=ORIENTED_EDGE('',*,*,#3361,.T.);
#4469=ORIENTED_EDGE('',*,*,#3196,.F.);
#4470=ORIENTED_EDGE('',*,*,#3351,.F.);
#4471=ORIENTED_EDGE('',*,*,#3178,.F.);
#4472=ORIENTED_EDGE('',*,*,#3362,.T.);
#4473=ORIENTED_EDGE('',*,*,#3171,.F.);
#4474=ORIENTED_EDGE('',*,*,#3356,.F.);
#4475=ORIENTED_EDGE('',*,*,#3363,.F.);
#4476=ORIENTED_EDGE('',*,*,#3361,.F.);
#4477=ORIENTED_EDGE('',*,*,#3364,.F.);
#4478=ORIENTED_EDGE('',*,*,#3346,.F.);
#4479=ORIENTED_EDGE('',*,*,#3364,.T.);
#4480=ORIENTED_EDGE('',*,*,#3172,.F.);
#4481=ORIENTED_EDGE('',*,*,#3365,.F.);
#4482=ORIENTED_EDGE('',*,*,#3347,.F.);
#4483=ORIENTED_EDGE('',*,*,#3363,.T.);
#4484=ORIENTED_EDGE('',*,*,#3345,.F.);
#4485=ORIENTED_EDGE('',*,*,#3366,.F.);
#4486=ORIENTED_EDGE('',*,*,#3197,.F.);
#4487=ORIENTED_EDGE('',*,*,#3365,.T.);
#4488=ORIENTED_EDGE('',*,*,#3362,.F.);
#4489=ORIENTED_EDGE('',*,*,#3367,.F.);
#4490=ORIENTED_EDGE('',*,*,#3348,.F.);
#4491=ORIENTED_EDGE('',*,*,#3366,.T.);
#4492=ORIENTED_EDGE('',*,*,#3344,.F.);
#4493=ORIENTED_EDGE('',*,*,#3368,.F.);
#4494=ORIENTED_EDGE('',*,*,#3360,.F.);
#4495=ORIENTED_EDGE('',*,*,#3367,.T.);
#4496=ORIENTED_EDGE('',*,*,#3177,.F.);
#4497=ORIENTED_EDGE('',*,*,#3369,.F.);
#4498=ORIENTED_EDGE('',*,*,#3349,.F.);
#4499=ORIENTED_EDGE('',*,*,#3368,.T.);
#4500=ORIENTED_EDGE('',*,*,#3343,.F.);
#4501=ORIENTED_EDGE('',*,*,#3370,.F.);
#4502=ORIENTED_EDGE('',*,*,#3192,.F.);
#4503=ORIENTED_EDGE('',*,*,#3369,.T.);
#4504=ORIENTED_EDGE('',*,*,#3357,.F.);
#4505=ORIENTED_EDGE('',*,*,#3371,.F.);
#4506=ORIENTED_EDGE('',*,*,#3350,.F.);
#4507=ORIENTED_EDGE('',*,*,#3370,.T.);
#4508=ORIENTED_EDGE('',*,*,#3342,.F.);
#4509=ORIENTED_EDGE('',*,*,#3372,.F.);
#4510=ORIENTED_EDGE('',*,*,#3359,.F.);
#4511=ORIENTED_EDGE('',*,*,#3371,.T.);
#4512=ORIENTED_EDGE('',*,*,#3182,.F.);
#4513=ORIENTED_EDGE('',*,*,#3373,.F.);
#4514=ORIENTED_EDGE('',*,*,#3339,.F.);
#4515=ORIENTED_EDGE('',*,*,#3372,.T.);
#4516=ORIENTED_EDGE('',*,*,#3341,.F.);
#4517=ORIENTED_EDGE('',*,*,#3374,.F.);
#4518=ORIENTED_EDGE('',*,*,#3187,.F.);
#4519=ORIENTED_EDGE('',*,*,#3373,.T.);
#4520=ORIENTED_EDGE('',*,*,#3358,.F.);
#4521=ORIENTED_EDGE('',*,*,#3374,.T.);
#4522=ORIENTED_EDGE('',*,*,#3340,.F.);
#4523=ORIENTED_EDGE('',*,*,#3235,.F.);
#4524=ORIENTED_EDGE('',*,*,#3375,.T.);
#4525=ORIENTED_EDGE('',*,*,#3208,.F.);
#4526=ORIENTED_EDGE('',*,*,#3376,.F.);
#4527=ORIENTED_EDGE('',*,*,#3231,.F.);
#4528=ORIENTED_EDGE('',*,*,#3376,.T.);
#4529=ORIENTED_EDGE('',*,*,#3377,.F.);
#4530=ORIENTED_EDGE('',*,*,#3377,.T.);
#4531=ORIENTED_EDGE('',*,*,#3213,.F.);
#4532=ORIENTED_EDGE('',*,*,#3378,.F.);
#4533=ORIENTED_EDGE('',*,*,#3228,.F.);
#4534=ORIENTED_EDGE('',*,*,#3225,.F.);
#4535=ORIENTED_EDGE('',*,*,#3378,.T.);
#4536=ORIENTED_EDGE('',*,*,#3379,.F.);
#4537=ORIENTED_EDGE('',*,*,#3379,.T.);
#4538=ORIENTED_EDGE('',*,*,#3212,.F.);
#4539=ORIENTED_EDGE('',*,*,#3380,.F.);
#4540=ORIENTED_EDGE('',*,*,#3221,.F.);
#4541=ORIENTED_EDGE('',*,*,#3380,.T.);
#4542=ORIENTED_EDGE('',*,*,#3211,.F.);
#4543=ORIENTED_EDGE('',*,*,#3381,.F.);
#4544=ORIENTED_EDGE('',*,*,#3328,.F.);
#4545=ORIENTED_EDGE('',*,*,#3321,.F.);
#4546=ORIENTED_EDGE('',*,*,#3329,.F.);
#4547=ORIENTED_EDGE('',*,*,#3381,.T.);
#4548=ORIENTED_EDGE('',*,*,#3216,.F.);
#4549=ORIENTED_EDGE('',*,*,#3382,.T.);
#4550=ORIENTED_EDGE('',*,*,#3233,.F.);
#4551=ORIENTED_EDGE('',*,*,#3383,.F.);
#4552=ORIENTED_EDGE('',*,*,#3383,.T.);
#4553=ORIENTED_EDGE('',*,*,#3232,.F.);
#4554=ORIENTED_EDGE('',*,*,#3384,.F.);
#4555=ORIENTED_EDGE('',*,*,#3384,.T.);
#4556=ORIENTED_EDGE('',*,*,#3229,.F.);
#4557=ORIENTED_EDGE('',*,*,#3385,.F.);
#4558=ORIENTED_EDGE('',*,*,#3217,.F.);
#4559=ORIENTED_EDGE('',*,*,#3385,.T.);
#4560=ORIENTED_EDGE('',*,*,#3226,.F.);
#4561=ORIENTED_EDGE('',*,*,#3386,.F.);
#4562=ORIENTED_EDGE('',*,*,#3386,.T.);
#4563=ORIENTED_EDGE('',*,*,#3223,.F.);
#4564=ORIENTED_EDGE('',*,*,#3387,.F.);
#4565=ORIENTED_EDGE('',*,*,#3218,.F.);
#4566=ORIENTED_EDGE('',*,*,#3387,.T.);
#4567=ORIENTED_EDGE('',*,*,#3331,.F.);
#4568=ORIENTED_EDGE('',*,*,#3388,.F.);
#4569=ORIENTED_EDGE('',*,*,#3219,.F.);
#4570=ORIENTED_EDGE('',*,*,#3388,.T.);
#4571=ORIENTED_EDGE('',*,*,#3330,.F.);
#4572=ORIENTED_EDGE('',*,*,#3306,.F.);
#4573=ORIENTED_EDGE('',*,*,#3300,.F.);
#4574=ORIENTED_EDGE('',*,*,#3389,.T.);
#4575=ORIENTED_EDGE('',*,*,#3288,.F.);
#4576=ORIENTED_EDGE('',*,*,#3390,.F.);
#4577=ORIENTED_EDGE('',*,*,#3390,.T.);
#4578=ORIENTED_EDGE('',*,*,#3285,.F.);
#4579=ORIENTED_EDGE('',*,*,#3391,.F.);
#4580=ORIENTED_EDGE('',*,*,#3391,.T.);
#4581=ORIENTED_EDGE('',*,*,#3283,.F.);
#4582=ORIENTED_EDGE('',*,*,#3392,.F.);
#4583=ORIENTED_EDGE('',*,*,#3301,.F.);
#4584=ORIENTED_EDGE('',*,*,#3392,.T.);
#4585=ORIENTED_EDGE('',*,*,#3280,.F.);
#4586=ORIENTED_EDGE('',*,*,#3393,.F.);
#4587=ORIENTED_EDGE('',*,*,#3393,.T.);
#4588=ORIENTED_EDGE('',*,*,#3279,.F.);
#4589=ORIENTED_EDGE('',*,*,#3394,.F.);
#4590=ORIENTED_EDGE('',*,*,#3302,.F.);
#4591=ORIENTED_EDGE('',*,*,#3394,.T.);
#4592=ORIENTED_EDGE('',*,*,#3130,.F.);
#4593=ORIENTED_EDGE('',*,*,#3395,.F.);
#4594=ORIENTED_EDGE('',*,*,#3303,.F.);
#4595=ORIENTED_EDGE('',*,*,#3395,.T.);
#4596=ORIENTED_EDGE('',*,*,#3129,.F.);
#4597=ORIENTED_EDGE('',*,*,#3312,.F.);
#4598=ORIENTED_EDGE('',*,*,#3309,.F.);
#4599=ORIENTED_EDGE('',*,*,#3127,.F.);
#4600=ORIENTED_EDGE('',*,*,#3126,.F.);
#4601=ORIENTED_EDGE('',*,*,#3396,.F.);
#4602=ORIENTED_EDGE('',*,*,#3396,.T.);
#4603=ORIENTED_EDGE('',*,*,#3132,.F.);
#4604=ORIENTED_EDGE('',*,*,#3397,.F.);
#4605=ORIENTED_EDGE('',*,*,#3275,.F.);
#4606=ORIENTED_EDGE('',*,*,#3397,.T.);
#4607=ORIENTED_EDGE('',*,*,#3278,.F.);
#4608=ORIENTED_EDGE('',*,*,#3398,.F.);
#4609=ORIENTED_EDGE('',*,*,#3276,.F.);
#4610=ORIENTED_EDGE('',*,*,#3398,.T.);
#4611=ORIENTED_EDGE('',*,*,#3282,.F.);
#4612=ORIENTED_EDGE('',*,*,#3120,.F.);
#4613=ORIENTED_EDGE('',*,*,#3119,.F.);
#4614=ORIENTED_EDGE('',*,*,#3122,.T.);
#4615=ORIENTED_EDGE('',*,*,#3287,.F.);
#4616=ORIENTED_EDGE('',*,*,#3115,.F.);
#4617=ORIENTED_EDGE('',*,*,#3113,.T.);
#4618=ORIENTED_EDGE('',*,*,#3258,.F.);
#4619=ORIENTED_EDGE('',*,*,#3107,.F.);
#4620=ORIENTED_EDGE('',*,*,#3110,.T.);
#4621=ORIENTED_EDGE('',*,*,#3109,.T.);
#4622=ORIENTED_EDGE('',*,*,#3253,.F.);
#4623=ORIENTED_EDGE('',*,*,#3399,.F.);
#4624=ORIENTED_EDGE('',*,*,#3399,.T.);
#4625=ORIENTED_EDGE('',*,*,#3252,.F.);
#4626=ORIENTED_EDGE('',*,*,#3400,.F.);
#4627=ORIENTED_EDGE('',*,*,#3271,.F.);
#4628=ORIENTED_EDGE('',*,*,#3400,.T.);
#4629=ORIENTED_EDGE('',*,*,#3325,.F.);
#4630=ORIENTED_EDGE('',*,*,#3401,.F.);
#4631=ORIENTED_EDGE('',*,*,#3272,.F.);
#4632=ORIENTED_EDGE('',*,*,#3401,.T.);
#4633=ORIENTED_EDGE('',*,*,#3324,.F.);
#4634=ORIENTED_EDGE('',*,*,#3318,.F.);
#4635=ORIENTED_EDGE('',*,*,#3315,.F.);
#4636=ORIENTED_EDGE('',*,*,#3327,.F.);
#4637=ORIENTED_EDGE('',*,*,#3402,.F.);
#4638=ORIENTED_EDGE('',*,*,#3402,.T.);
#4639=ORIENTED_EDGE('',*,*,#3326,.F.);
#4640=ORIENTED_EDGE('',*,*,#3403,.F.);
#4641=ORIENTED_EDGE('',*,*,#3246,.F.);
#4642=ORIENTED_EDGE('',*,*,#3403,.T.);
#4643=ORIENTED_EDGE('',*,*,#3250,.F.);
#4644=ORIENTED_EDGE('',*,*,#3404,.F.);
#4645=ORIENTED_EDGE('',*,*,#3247,.F.);
#4646=ORIENTED_EDGE('',*,*,#3404,.T.);
#4647=ORIENTED_EDGE('',*,*,#3255,.F.);
#4648=ORIENTED_EDGE('',*,*,#3405,.F.);
#4649=ORIENTED_EDGE('',*,*,#3405,.T.);
#4650=ORIENTED_EDGE('',*,*,#3257,.F.);
#4651=ORIENTED_EDGE('',*,*,#3406,.F.);
#4652=ORIENTED_EDGE('',*,*,#3248,.F.);
#4653=ORIENTED_EDGE('',*,*,#3406,.T.);
#4654=ORIENTED_EDGE('',*,*,#3260,.F.);
#4655=ORIENTED_EDGE('',*,*,#3407,.F.);
#4656=ORIENTED_EDGE('',*,*,#3262,.F.);
#4657=ORIENTED_EDGE('',*,*,#3408,.T.);
#4658=ORIENTED_EDGE('',*,*,#3243,.F.);
#4659=ORIENTED_EDGE('',*,*,#3407,.T.);
#4660=ORIENTED_EDGE('',*,*,#3141,.F.);
#4661=ORIENTED_EDGE('',*,*,#3320,.F.);
#4662=ORIENTED_EDGE('',*,*,#3409,.F.);
#4663=ORIENTED_EDGE('',*,*,#3409,.T.);
#4664=ORIENTED_EDGE('',*,*,#3319,.F.);
#4665=ORIENTED_EDGE('',*,*,#3410,.F.);
#4666=ORIENTED_EDGE('',*,*,#3236,.F.);
#4667=ORIENTED_EDGE('',*,*,#3410,.T.);
#4668=ORIENTED_EDGE('',*,*,#3209,.F.);
#4669=ORIENTED_EDGE('',*,*,#3411,.F.);
#4670=ORIENTED_EDGE('',*,*,#3237,.F.);
#4671=ORIENTED_EDGE('',*,*,#3411,.T.);
#4672=ORIENTED_EDGE('',*,*,#3375,.F.);
#4673=ORIENTED_EDGE('',*,*,#3412,.F.);
#4674=ORIENTED_EDGE('',*,*,#3238,.F.);
#4675=ORIENTED_EDGE('',*,*,#3412,.T.);
#4676=ORIENTED_EDGE('',*,*,#3234,.F.);
#4677=ORIENTED_EDGE('',*,*,#3413,.F.);
#4678=ORIENTED_EDGE('',*,*,#3239,.F.);
#4679=ORIENTED_EDGE('',*,*,#3413,.T.);
#4680=ORIENTED_EDGE('',*,*,#3382,.F.);
#4681=ORIENTED_EDGE('',*,*,#3414,.F.);
#4682=ORIENTED_EDGE('',*,*,#3240,.F.);
#4683=ORIENTED_EDGE('',*,*,#3414,.T.);
#4684=ORIENTED_EDGE('',*,*,#3215,.F.);
#4685=ORIENTED_EDGE('',*,*,#3415,.F.);
#4686=ORIENTED_EDGE('',*,*,#3241,.F.);
#4687=ORIENTED_EDGE('',*,*,#3415,.T.);
#4688=ORIENTED_EDGE('',*,*,#3305,.F.);
#4689=ORIENTED_EDGE('',*,*,#3416,.F.);
#4690=ORIENTED_EDGE('',*,*,#3242,.F.);
#4691=ORIENTED_EDGE('',*,*,#3304,.F.);
#4692=ORIENTED_EDGE('',*,*,#3139,.F.);
#4693=ORIENTED_EDGE('',*,*,#3416,.T.);
#4694=ORIENTED_EDGE('',*,*,#3310,.F.);
#4695=ORIENTED_EDGE('',*,*,#3323,.F.);
#4696=ORIENTED_EDGE('',*,*,#3417,.F.);
#4697=ORIENTED_EDGE('',*,*,#3417,.T.);
#4698=ORIENTED_EDGE('',*,*,#3297,.F.);
#4699=ORIENTED_EDGE('',*,*,#3418,.F.);
#4700=ORIENTED_EDGE('',*,*,#3311,.F.);
#4701=ORIENTED_EDGE('',*,*,#3418,.T.);
#4702=ORIENTED_EDGE('',*,*,#3296,.F.);
#4703=ORIENTED_EDGE('',*,*,#3419,.F.);
#4704=ORIENTED_EDGE('',*,*,#3299,.F.);
#4705=ORIENTED_EDGE('',*,*,#3419,.T.);
#4706=ORIENTED_EDGE('',*,*,#3295,.F.);
#4707=ORIENTED_EDGE('',*,*,#3420,.F.);
#4708=ORIENTED_EDGE('',*,*,#3389,.F.);
#4709=ORIENTED_EDGE('',*,*,#3420,.T.);
#4710=ORIENTED_EDGE('',*,*,#3294,.F.);
#4711=ORIENTED_EDGE('',*,*,#3421,.F.);
#4712=ORIENTED_EDGE('',*,*,#3289,.F.);
#4713=ORIENTED_EDGE('',*,*,#3421,.T.);
#4714=ORIENTED_EDGE('',*,*,#3293,.F.);
#4715=ORIENTED_EDGE('',*,*,#3422,.F.);
#4716=ORIENTED_EDGE('',*,*,#3117,.F.);
#4717=ORIENTED_EDGE('',*,*,#3422,.T.);
#4718=ORIENTED_EDGE('',*,*,#3292,.F.);
#4719=ORIENTED_EDGE('',*,*,#3423,.F.);
#4720=ORIENTED_EDGE('',*,*,#3273,.F.);
#4721=ORIENTED_EDGE('',*,*,#3423,.T.);
#4722=ORIENTED_EDGE('',*,*,#3291,.F.);
#4723=ORIENTED_EDGE('',*,*,#3424,.F.);
#4724=ORIENTED_EDGE('',*,*,#3307,.F.);
#4725=ORIENTED_EDGE('',*,*,#3424,.T.);
#4726=ORIENTED_EDGE('',*,*,#3322,.F.);
#4727=ORIENTED_EDGE('',*,*,#3308,.F.);
#4728=ORIENTED_EDGE('',*,*,#3316,.F.);
#4729=ORIENTED_EDGE('',*,*,#3134,.F.);
#4730=ORIENTED_EDGE('',*,*,#3425,.F.);
#4731=ORIENTED_EDGE('',*,*,#3425,.T.);
#4732=ORIENTED_EDGE('',*,*,#3268,.F.);
#4733=ORIENTED_EDGE('',*,*,#3426,.F.);
#4734=ORIENTED_EDGE('',*,*,#3317,.F.);
#4735=ORIENTED_EDGE('',*,*,#3426,.T.);
#4736=ORIENTED_EDGE('',*,*,#3267,.F.);
#4737=ORIENTED_EDGE('',*,*,#3106,.F.);
#4738=ORIENTED_EDGE('',*,*,#3270,.F.);
#4739=ORIENTED_EDGE('',*,*,#3104,.T.);
#4740=ORIENTED_EDGE('',*,*,#3266,.F.);
#4741=ORIENTED_EDGE('',*,*,#3427,.F.);
#4742=ORIENTED_EDGE('',*,*,#3261,.F.);
#4743=ORIENTED_EDGE('',*,*,#3427,.T.);
#4744=ORIENTED_EDGE('',*,*,#3265,.F.);
#4745=ORIENTED_EDGE('',*,*,#3428,.F.);
#4746=ORIENTED_EDGE('',*,*,#3408,.F.);
#4747=ORIENTED_EDGE('',*,*,#3428,.T.);
#4748=ORIENTED_EDGE('',*,*,#3264,.F.);
#4749=ORIENTED_EDGE('',*,*,#3429,.F.);
#4750=ORIENTED_EDGE('',*,*,#3244,.F.);
#4751=ORIENTED_EDGE('',*,*,#3429,.T.);
#4752=ORIENTED_EDGE('',*,*,#3263,.F.);
#4753=ORIENTED_EDGE('',*,*,#3430,.F.);
#4754=ORIENTED_EDGE('',*,*,#3313,.F.);
#4755=ORIENTED_EDGE('',*,*,#3430,.T.);
#4756=ORIENTED_EDGE('',*,*,#3137,.F.);
#4757=ORIENTED_EDGE('',*,*,#3314,.F.);
#4758=ORIENTED_EDGE('',*,*,#3431,.F.);
#4759=ORIENTED_EDGE('',*,*,#3432,.T.);
#4760=ORIENTED_EDGE('',*,*,#3433,.F.);
#4761=ORIENTED_EDGE('',*,*,#3434,.F.);
#4762=ORIENTED_EDGE('',*,*,#3435,.F.);
#4763=ORIENTED_EDGE('',*,*,#3436,.F.);
#4764=ORIENTED_EDGE('',*,*,#3437,.F.);
#4765=ORIENTED_EDGE('',*,*,#3438,.T.);
#4766=ORIENTED_EDGE('',*,*,#3439,.F.);
#4767=ORIENTED_EDGE('',*,*,#3440,.F.);
#4768=ORIENTED_EDGE('',*,*,#3441,.F.);
#4769=ORIENTED_EDGE('',*,*,#3442,.F.);
#4770=ORIENTED_EDGE('',*,*,#3443,.F.);
#4771=ORIENTED_EDGE('',*,*,#3444,.T.);
#4772=ORIENTED_EDGE('',*,*,#3445,.T.);
#4773=ORIENTED_EDGE('',*,*,#3446,.T.);
#4774=ORIENTED_EDGE('',*,*,#3437,.T.);
#4775=ORIENTED_EDGE('',*,*,#3447,.T.);
#4776=ORIENTED_EDGE('',*,*,#3448,.T.);
#4777=ORIENTED_EDGE('',*,*,#3431,.T.);
#4778=ORIENTED_EDGE('',*,*,#3436,.T.);
#4779=ORIENTED_EDGE('',*,*,#3449,.T.);
#4780=ORIENTED_EDGE('',*,*,#3447,.F.);
#4781=ORIENTED_EDGE('',*,*,#3442,.T.);
#4782=ORIENTED_EDGE('',*,*,#3450,.T.);
#4783=ORIENTED_EDGE('',*,*,#3451,.F.);
#4784=ORIENTED_EDGE('',*,*,#3452,.F.);
#4785=ORIENTED_EDGE('',*,*,#3453,.T.);
#4786=ORIENTED_EDGE('',*,*,#3454,.T.);
#4787=ORIENTED_EDGE('',*,*,#3453,.F.);
#4788=ORIENTED_EDGE('',*,*,#3451,.T.);
#4789=ORIENTED_EDGE('',*,*,#3452,.T.);
#4790=ORIENTED_EDGE('',*,*,#3455,.T.);
#4791=ORIENTED_EDGE('',*,*,#3455,.F.);
#4792=ORIENTED_EDGE('',*,*,#3456,.F.);
#4793=ORIENTED_EDGE('',*,*,#3457,.F.);
#4794=ORIENTED_EDGE('',*,*,#3458,.T.);
#4795=ORIENTED_EDGE('',*,*,#3459,.F.);
#4796=ORIENTED_EDGE('',*,*,#3458,.F.);
#4797=ORIENTED_EDGE('',*,*,#3460,.F.);
#4798=ORIENTED_EDGE('',*,*,#3461,.T.);
#4799=ORIENTED_EDGE('',*,*,#3462,.T.);
#4800=ORIENTED_EDGE('',*,*,#3461,.F.);
#4801=ORIENTED_EDGE('',*,*,#3456,.T.);
#4802=ORIENTED_EDGE('',*,*,#3457,.T.);
#4803=ORIENTED_EDGE('',*,*,#3463,.T.);
#4804=ORIENTED_EDGE('',*,*,#3433,.T.);
#4805=ORIENTED_EDGE('',*,*,#3464,.T.);
#4806=ORIENTED_EDGE('',*,*,#3465,.T.);
#4807=ORIENTED_EDGE('',*,*,#3466,.F.);
#4808=ORIENTED_EDGE('',*,*,#3465,.F.);
#4809=ORIENTED_EDGE('',*,*,#3467,.T.);
#4810=ORIENTED_EDGE('',*,*,#3434,.T.);
#4811=ORIENTED_EDGE('',*,*,#3463,.F.);
#4812=ORIENTED_EDGE('',*,*,#3439,.T.);
#4813=ORIENTED_EDGE('',*,*,#3468,.T.);
#4814=ORIENTED_EDGE('',*,*,#3469,.T.);
#4815=ORIENTED_EDGE('',*,*,#3440,.T.);
#4816=ORIENTED_EDGE('',*,*,#3459,.T.);
#4817=ORIENTED_EDGE('',*,*,#3462,.F.);
#4818=ORIENTED_EDGE('',*,*,#3470,.T.);
#4819=ORIENTED_EDGE('',*,*,#3471,.T.);
#4820=ORIENTED_EDGE('',*,*,#3472,.T.);
#4821=ORIENTED_EDGE('',*,*,#3460,.T.);
#4822=ORIENTED_EDGE('',*,*,#3473,.F.);
#4823=ORIENTED_EDGE('',*,*,#3474,.T.);
#4824=ORIENTED_EDGE('',*,*,#3475,.T.);
#4825=ORIENTED_EDGE('',*,*,#3471,.F.);
#4826=ORIENTED_EDGE('',*,*,#3476,.F.);
#4827=ORIENTED_EDGE('',*,*,#3477,.T.);
#4828=ORIENTED_EDGE('',*,*,#3473,.T.);
#4829=ORIENTED_EDGE('',*,*,#3470,.F.);
#4830=ORIENTED_EDGE('',*,*,#3475,.F.);
#4831=ORIENTED_EDGE('',*,*,#3478,.T.);
#4832=ORIENTED_EDGE('',*,*,#3476,.T.);
#4833=ORIENTED_EDGE('',*,*,#3472,.F.);
#4834=ORIENTED_EDGE('',*,*,#3478,.F.);
#4835=ORIENTED_EDGE('',*,*,#3474,.F.);
#4836=ORIENTED_EDGE('',*,*,#3477,.F.);
#4837=ORIENTED_EDGE('',*,*,#3454,.F.);
#4838=ORIENTED_EDGE('',*,*,#3479,.F.);
#4839=ORIENTED_EDGE('',*,*,#3480,.T.);
#4840=ORIENTED_EDGE('',*,*,#3481,.T.);
#4841=ORIENTED_EDGE('',*,*,#3482,.F.);
#4842=ORIENTED_EDGE('',*,*,#3483,.F.);
#4843=ORIENTED_EDGE('',*,*,#3484,.F.);
#4844=ORIENTED_EDGE('',*,*,#3481,.F.);
#4845=ORIENTED_EDGE('',*,*,#3485,.T.);
#4846=ORIENTED_EDGE('',*,*,#3486,.T.);
#4847=ORIENTED_EDGE('',*,*,#3487,.F.);
#4848=ORIENTED_EDGE('',*,*,#3488,.F.);
#4849=ORIENTED_EDGE('',*,*,#3489,.F.);
#4850=ORIENTED_EDGE('',*,*,#3486,.F.);
#4851=ORIENTED_EDGE('',*,*,#3490,.T.);
#4852=ORIENTED_EDGE('',*,*,#3491,.T.);
#4853=ORIENTED_EDGE('',*,*,#3492,.F.);
#4854=ORIENTED_EDGE('',*,*,#3493,.F.);
#4855=ORIENTED_EDGE('',*,*,#3494,.F.);
#4856=ORIENTED_EDGE('',*,*,#3491,.F.);
#4857=ORIENTED_EDGE('',*,*,#3495,.T.);
#4858=ORIENTED_EDGE('',*,*,#3496,.T.);
#4859=ORIENTED_EDGE('',*,*,#3497,.F.);
#4860=ORIENTED_EDGE('',*,*,#3498,.F.);
#4861=ORIENTED_EDGE('',*,*,#3499,.F.);
#4862=ORIENTED_EDGE('',*,*,#3496,.F.);
#4863=ORIENTED_EDGE('',*,*,#3500,.T.);
#4864=ORIENTED_EDGE('',*,*,#3501,.T.);
#4865=ORIENTED_EDGE('',*,*,#3444,.F.);
#4866=ORIENTED_EDGE('',*,*,#3502,.F.);
#4867=ORIENTED_EDGE('',*,*,#3503,.F.);
#4868=ORIENTED_EDGE('',*,*,#3501,.F.);
#4869=ORIENTED_EDGE('',*,*,#3504,.T.);
#4870=ORIENTED_EDGE('',*,*,#3479,.T.);
#4871=ORIENTED_EDGE('',*,*,#3505,.F.);
#4872=ORIENTED_EDGE('',*,*,#3506,.F.);
#4873=ORIENTED_EDGE('',*,*,#3445,.F.);
#4874=ORIENTED_EDGE('',*,*,#3466,.T.);
#4875=ORIENTED_EDGE('',*,*,#3480,.F.);
#4876=ORIENTED_EDGE('',*,*,#3504,.F.);
#4877=ORIENTED_EDGE('',*,*,#3500,.F.);
#4878=ORIENTED_EDGE('',*,*,#3495,.F.);
#4879=ORIENTED_EDGE('',*,*,#3490,.F.);
#4880=ORIENTED_EDGE('',*,*,#3485,.F.);
#4881=ORIENTED_EDGE('',*,*,#3505,.T.);
#4882=ORIENTED_EDGE('',*,*,#3484,.T.);
#4883=ORIENTED_EDGE('',*,*,#3507,.F.);
#4884=ORIENTED_EDGE('',*,*,#3508,.F.);
#4885=ORIENTED_EDGE('',*,*,#3497,.T.);
#4886=ORIENTED_EDGE('',*,*,#3503,.T.);
#4887=ORIENTED_EDGE('',*,*,#3509,.F.);
#4888=ORIENTED_EDGE('',*,*,#3492,.T.);
#4889=ORIENTED_EDGE('',*,*,#3499,.T.);
#4890=ORIENTED_EDGE('',*,*,#3510,.F.);
#4891=ORIENTED_EDGE('',*,*,#3487,.T.);
#4892=ORIENTED_EDGE('',*,*,#3494,.T.);
#4893=ORIENTED_EDGE('',*,*,#3511,.F.);
#4894=ORIENTED_EDGE('',*,*,#3482,.T.);
#4895=ORIENTED_EDGE('',*,*,#3489,.T.);
#4896=ORIENTED_EDGE('',*,*,#3483,.T.);
#4897=ORIENTED_EDGE('',*,*,#3511,.T.);
#4898=ORIENTED_EDGE('',*,*,#3488,.T.);
#4899=ORIENTED_EDGE('',*,*,#3510,.T.);
#4900=ORIENTED_EDGE('',*,*,#3493,.T.);
#4901=ORIENTED_EDGE('',*,*,#3509,.T.);
#4902=ORIENTED_EDGE('',*,*,#3498,.T.);
#4903=ORIENTED_EDGE('',*,*,#3508,.T.);
#4904=ORIENTED_EDGE('',*,*,#3502,.T.);
#4905=ORIENTED_EDGE('',*,*,#3443,.T.);
#4906=ORIENTED_EDGE('',*,*,#3506,.T.);
#4907=ORIENTED_EDGE('',*,*,#3507,.T.);
#4908=ORIENTED_EDGE('',*,*,#3438,.F.);
#4909=ORIENTED_EDGE('',*,*,#3446,.F.);
#4910=ORIENTED_EDGE('',*,*,#3450,.F.);
#4911=ORIENTED_EDGE('',*,*,#3441,.T.);
#4912=ORIENTED_EDGE('',*,*,#3469,.F.);
#4913=ORIENTED_EDGE('',*,*,#3468,.F.);
#4914=ORIENTED_EDGE('',*,*,#3432,.F.);
#4915=ORIENTED_EDGE('',*,*,#3448,.F.);
#4916=ORIENTED_EDGE('',*,*,#3449,.F.);
#4917=ORIENTED_EDGE('',*,*,#3435,.T.);
#4918=ORIENTED_EDGE('',*,*,#3467,.F.);
#4919=ORIENTED_EDGE('',*,*,#3464,.F.);
#4920=ORIENTED_EDGE('',*,*,#3512,.F.);
#4921=ORIENTED_EDGE('',*,*,#3513,.T.);
#4922=ORIENTED_EDGE('',*,*,#3513,.F.);
#4923=ORIENTED_EDGE('',*,*,#3514,.F.);
#4924=ORIENTED_EDGE('',*,*,#3515,.T.);
#4925=ORIENTED_EDGE('',*,*,#3516,.F.);
#4926=ORIENTED_EDGE('',*,*,#3516,.T.);
#4927=ORIENTED_EDGE('',*,*,#3517,.T.);
#4928=ORIENTED_EDGE('',*,*,#3512,.T.);
#4929=ORIENTED_EDGE('',*,*,#3518,.T.);
#4930=ORIENTED_EDGE('',*,*,#3517,.F.);
#4931=ORIENTED_EDGE('',*,*,#3515,.F.);
#4932=ORIENTED_EDGE('',*,*,#3518,.F.);
#4933=ORIENTED_EDGE('',*,*,#3514,.T.);
#4934=ORIENTED_EDGE('',*,*,#3519,.T.);
#4935=ORIENTED_EDGE('',*,*,#3520,.T.);
#4936=ORIENTED_EDGE('',*,*,#3521,.F.);
#4937=ORIENTED_EDGE('',*,*,#3522,.F.);
#4938=ORIENTED_EDGE('',*,*,#3520,.F.);
#4939=ORIENTED_EDGE('',*,*,#3523,.F.);
#4940=ORIENTED_EDGE('',*,*,#3524,.F.);
#4941=ORIENTED_EDGE('',*,*,#3525,.T.);
#4942=ORIENTED_EDGE('',*,*,#3521,.T.);
#4943=ORIENTED_EDGE('',*,*,#3522,.T.);
#4944=ORIENTED_EDGE('',*,*,#3525,.F.);
#4945=ORIENTED_EDGE('',*,*,#3526,.T.);
#4946=ORIENTED_EDGE('',*,*,#3527,.T.);
#4947=ORIENTED_EDGE('',*,*,#3528,.F.);
#4948=ORIENTED_EDGE('',*,*,#3529,.F.);
#4949=ORIENTED_EDGE('',*,*,#3527,.F.);
#4950=ORIENTED_EDGE('',*,*,#3530,.F.);
#4951=ORIENTED_EDGE('',*,*,#3531,.F.);
#4952=ORIENTED_EDGE('',*,*,#3532,.T.);
#4953=ORIENTED_EDGE('',*,*,#3528,.T.);
#4954=ORIENTED_EDGE('',*,*,#3529,.T.);
#4955=ORIENTED_EDGE('',*,*,#3532,.F.);
#4956=ORIENTED_EDGE('',*,*,#3533,.T.);
#4957=ORIENTED_EDGE('',*,*,#3534,.T.);
#4958=ORIENTED_EDGE('',*,*,#3535,.F.);
#4959=ORIENTED_EDGE('',*,*,#3536,.F.);
#4960=ORIENTED_EDGE('',*,*,#3534,.F.);
#4961=ORIENTED_EDGE('',*,*,#3537,.F.);
#4962=ORIENTED_EDGE('',*,*,#3538,.F.);
#4963=ORIENTED_EDGE('',*,*,#3539,.T.);
#4964=ORIENTED_EDGE('',*,*,#3535,.T.);
#4965=ORIENTED_EDGE('',*,*,#3536,.T.);
#4966=ORIENTED_EDGE('',*,*,#3539,.F.);
#4967=ORIENTED_EDGE('',*,*,#3540,.T.);
#4968=ORIENTED_EDGE('',*,*,#3541,.T.);
#4969=ORIENTED_EDGE('',*,*,#3542,.F.);
#4970=ORIENTED_EDGE('',*,*,#3543,.F.);
#4971=ORIENTED_EDGE('',*,*,#3541,.F.);
#4972=ORIENTED_EDGE('',*,*,#3544,.T.);
#4973=ORIENTED_EDGE('',*,*,#3545,.T.);
#4974=ORIENTED_EDGE('',*,*,#3542,.T.);
#4975=ORIENTED_EDGE('',*,*,#3543,.T.);
#4976=ORIENTED_EDGE('',*,*,#3545,.F.);
#4977=ORIENTED_EDGE('',*,*,#3546,.T.);
#4978=ORIENTED_EDGE('',*,*,#3547,.T.);
#4979=ORIENTED_EDGE('',*,*,#3548,.T.);
#4980=ORIENTED_EDGE('',*,*,#3549,.T.);
#4981=ORIENTED_EDGE('',*,*,#3550,.T.);
#4982=ORIENTED_EDGE('',*,*,#3548,.F.);
#4983=ORIENTED_EDGE('',*,*,#3551,.T.);
#4984=ORIENTED_EDGE('',*,*,#3552,.T.);
#4985=ORIENTED_EDGE('',*,*,#3549,.F.);
#4986=ORIENTED_EDGE('',*,*,#3550,.F.);
#4987=ORIENTED_EDGE('',*,*,#3552,.F.);
#4988=ORIENTED_EDGE('',*,*,#3553,.T.);
#4989=ORIENTED_EDGE('',*,*,#3544,.F.);
#4990=ORIENTED_EDGE('',*,*,#3554,.T.);
#4991=ORIENTED_EDGE('',*,*,#3555,.T.);
#4992=ORIENTED_EDGE('',*,*,#3554,.F.);
#4993=ORIENTED_EDGE('',*,*,#3546,.F.);
#4994=ORIENTED_EDGE('',*,*,#3537,.T.);
#4995=ORIENTED_EDGE('',*,*,#3538,.T.);
#4996=ORIENTED_EDGE('',*,*,#3556,.T.);
#4997=ORIENTED_EDGE('',*,*,#3540,.F.);
#4998=ORIENTED_EDGE('',*,*,#3556,.F.);
#4999=ORIENTED_EDGE('',*,*,#3530,.T.);
#5000=ORIENTED_EDGE('',*,*,#3531,.T.);
#5001=ORIENTED_EDGE('',*,*,#3557,.T.);
#5002=ORIENTED_EDGE('',*,*,#3533,.F.);
#5003=ORIENTED_EDGE('',*,*,#3557,.F.);
#5004=ORIENTED_EDGE('',*,*,#3523,.T.);
#5005=ORIENTED_EDGE('',*,*,#3524,.T.);
#5006=ORIENTED_EDGE('',*,*,#3558,.T.);
#5007=ORIENTED_EDGE('',*,*,#3526,.F.);
#5008=ORIENTED_EDGE('',*,*,#3558,.F.);
#5009=ORIENTED_EDGE('',*,*,#3551,.F.);
#5010=ORIENTED_EDGE('',*,*,#3559,.T.);
#5011=ORIENTED_EDGE('',*,*,#3519,.F.);
#5012=ORIENTED_EDGE('',*,*,#3559,.F.);
#5013=ORIENTED_EDGE('',*,*,#3553,.F.);
#5014=ORIENTED_EDGE('',*,*,#3560,.T.);
#5015=ORIENTED_EDGE('',*,*,#3561,.T.);
#5016=ORIENTED_EDGE('',*,*,#3562,.T.);
#5017=ORIENTED_EDGE('',*,*,#3563,.F.);
#5018=ORIENTED_EDGE('',*,*,#3564,.F.);
#5019=ORIENTED_EDGE('',*,*,#3565,.F.);
#5020=ORIENTED_EDGE('',*,*,#3563,.T.);
#5021=ORIENTED_EDGE('',*,*,#3566,.T.);
#5022=ORIENTED_EDGE('',*,*,#3567,.T.);
#5023=ORIENTED_EDGE('',*,*,#3568,.F.);
#5024=ORIENTED_EDGE('',*,*,#3569,.F.);
#5025=ORIENTED_EDGE('',*,*,#3570,.F.);
#5026=ORIENTED_EDGE('',*,*,#3571,.F.);
#5027=ORIENTED_EDGE('',*,*,#3572,.F.);
#5028=ORIENTED_EDGE('',*,*,#3573,.T.);
#5029=ORIENTED_EDGE('',*,*,#3574,.T.);
#5030=ORIENTED_EDGE('',*,*,#3568,.T.);
#5031=ORIENTED_EDGE('',*,*,#3575,.F.);
#5032=ORIENTED_EDGE('',*,*,#3572,.T.);
#5033=ORIENTED_EDGE('',*,*,#3576,.T.);
#5034=ORIENTED_EDGE('',*,*,#3577,.T.);
#5035=ORIENTED_EDGE('',*,*,#3578,.F.);
#5036=ORIENTED_EDGE('',*,*,#3579,.F.);
#5037=ORIENTED_EDGE('',*,*,#3580,.F.);
#5038=ORIENTED_EDGE('',*,*,#3578,.T.);
#5039=ORIENTED_EDGE('',*,*,#3581,.T.);
#5040=ORIENTED_EDGE('',*,*,#3582,.T.);
#5041=ORIENTED_EDGE('',*,*,#3583,.F.);
#5042=ORIENTED_EDGE('',*,*,#3584,.F.);
#5043=ORIENTED_EDGE('',*,*,#3585,.F.);
#5044=ORIENTED_EDGE('',*,*,#3583,.T.);
#5045=ORIENTED_EDGE('',*,*,#3586,.T.);
#5046=ORIENTED_EDGE('',*,*,#3587,.T.);
#5047=ORIENTED_EDGE('',*,*,#3560,.F.);
#5048=ORIENTED_EDGE('',*,*,#3588,.F.);
#5049=ORIENTED_EDGE('',*,*,#3589,.F.);
#5050=ORIENTED_EDGE('',*,*,#3590,.T.);
#5051=ORIENTED_EDGE('',*,*,#3591,.T.);
#5052=ORIENTED_EDGE('',*,*,#3592,.T.);
#5053=ORIENTED_EDGE('',*,*,#3593,.T.);
#5054=ORIENTED_EDGE('',*,*,#3594,.T.);
#5055=ORIENTED_EDGE('',*,*,#3595,.T.);
#5056=ORIENTED_EDGE('',*,*,#3555,.F.);
#5057=ORIENTED_EDGE('',*,*,#3596,.F.);
#5058=ORIENTED_EDGE('',*,*,#3597,.T.);
#5059=ORIENTED_EDGE('',*,*,#3598,.T.);
#5060=ORIENTED_EDGE('',*,*,#3599,.T.);
#5061=ORIENTED_EDGE('',*,*,#3600,.T.);
#5062=ORIENTED_EDGE('',*,*,#3601,.T.);
#5063=ORIENTED_EDGE('',*,*,#3547,.F.);
#5064=ORIENTED_EDGE('',*,*,#3569,.T.);
#5065=ORIENTED_EDGE('',*,*,#3574,.F.);
#5066=ORIENTED_EDGE('',*,*,#3596,.T.);
#5067=ORIENTED_EDGE('',*,*,#3564,.T.);
#5068=ORIENTED_EDGE('',*,*,#3570,.T.);
#5069=ORIENTED_EDGE('',*,*,#3601,.F.);
#5070=ORIENTED_EDGE('',*,*,#3565,.T.);
#5071=ORIENTED_EDGE('',*,*,#3600,.F.);
#5072=ORIENTED_EDGE('',*,*,#3588,.T.);
#5073=ORIENTED_EDGE('',*,*,#3584,.T.);
#5074=ORIENTED_EDGE('',*,*,#3589,.T.);
#5075=ORIENTED_EDGE('',*,*,#3599,.F.);
#5076=ORIENTED_EDGE('',*,*,#3579,.T.);
#5077=ORIENTED_EDGE('',*,*,#3585,.T.);
#5078=ORIENTED_EDGE('',*,*,#3598,.F.);
#5079=ORIENTED_EDGE('',*,*,#3580,.T.);
#5080=ORIENTED_EDGE('',*,*,#3597,.F.);
#5081=ORIENTED_EDGE('',*,*,#3573,.F.);
#5082=ORIENTED_EDGE('',*,*,#3571,.T.);
#5083=ORIENTED_EDGE('',*,*,#3590,.F.);
#5084=ORIENTED_EDGE('',*,*,#3576,.F.);
#5085=ORIENTED_EDGE('',*,*,#3595,.F.);
#5086=ORIENTED_EDGE('',*,*,#3581,.F.);
#5087=ORIENTED_EDGE('',*,*,#3577,.F.);
#5088=ORIENTED_EDGE('',*,*,#3594,.F.);
#5089=ORIENTED_EDGE('',*,*,#3586,.F.);
#5090=ORIENTED_EDGE('',*,*,#3582,.F.);
#5091=ORIENTED_EDGE('',*,*,#3587,.F.);
#5092=ORIENTED_EDGE('',*,*,#3593,.F.);
#5093=ORIENTED_EDGE('',*,*,#3561,.F.);
#5094=ORIENTED_EDGE('',*,*,#3592,.F.);
#5095=ORIENTED_EDGE('',*,*,#3566,.F.);
#5096=ORIENTED_EDGE('',*,*,#3562,.F.);
#5097=ORIENTED_EDGE('',*,*,#3591,.F.);
#5098=ORIENTED_EDGE('',*,*,#3575,.T.);
#5099=ORIENTED_EDGE('',*,*,#3567,.F.);
#5100=ORIENTED_EDGE('',*,*,#3602,.F.);
#5101=ORIENTED_EDGE('',*,*,#3603,.T.);
#5102=ORIENTED_EDGE('',*,*,#3604,.T.);
#5103=ORIENTED_EDGE('',*,*,#3603,.F.);
#5104=ORIENTED_EDGE('',*,*,#3605,.F.);
#5105=ORIENTED_EDGE('',*,*,#3602,.T.);
#5106=ORIENTED_EDGE('',*,*,#3605,.T.);
#5107=ORIENTED_EDGE('',*,*,#3604,.F.);
#5108=ORIENTED_EDGE('',*,*,#3606,.T.);
#5109=ORIENTED_EDGE('',*,*,#3607,.T.);
#5110=ORIENTED_EDGE('',*,*,#3608,.T.);
#5111=ORIENTED_EDGE('',*,*,#3609,.T.);
#5112=ORIENTED_EDGE('',*,*,#3608,.F.);
#5113=ORIENTED_EDGE('',*,*,#3610,.F.);
#5114=ORIENTED_EDGE('',*,*,#3611,.F.);
#5115=ORIENTED_EDGE('',*,*,#3612,.T.);
#5116=ORIENTED_EDGE('',*,*,#3613,.T.);
#5117=ORIENTED_EDGE('',*,*,#3614,.T.);
#5118=ORIENTED_EDGE('',*,*,#3612,.F.);
#5119=ORIENTED_EDGE('',*,*,#3606,.F.);
#5120=ORIENTED_EDGE('',*,*,#3607,.F.);
#5121=ORIENTED_EDGE('',*,*,#3615,.T.);
#5122=ORIENTED_EDGE('',*,*,#3613,.F.);
#5123=ORIENTED_EDGE('',*,*,#3614,.F.);
#5124=ORIENTED_EDGE('',*,*,#3615,.F.);
#5125=ORIENTED_EDGE('',*,*,#3616,.F.);
#5126=ORIENTED_EDGE('',*,*,#3617,.F.);
#5127=ORIENTED_EDGE('',*,*,#3618,.T.);
#5128=ORIENTED_EDGE('',*,*,#3610,.T.);
#5129=ORIENTED_EDGE('',*,*,#3611,.T.);
#5130=ORIENTED_EDGE('',*,*,#3618,.F.);
#5131=ORIENTED_EDGE('',*,*,#3619,.F.);
#5132=ORIENTED_EDGE('',*,*,#3620,.F.);
#5133=ORIENTED_EDGE('',*,*,#3621,.T.);
#5134=ORIENTED_EDGE('',*,*,#3622,.T.);
#5135=ORIENTED_EDGE('',*,*,#3623,.T.);
#5136=ORIENTED_EDGE('',*,*,#3621,.F.);
#5137=ORIENTED_EDGE('',*,*,#3616,.T.);
#5138=ORIENTED_EDGE('',*,*,#3617,.T.);
#5139=ORIENTED_EDGE('',*,*,#3624,.T.);
#5140=ORIENTED_EDGE('',*,*,#3622,.F.);
#5141=ORIENTED_EDGE('',*,*,#3623,.F.);
#5142=ORIENTED_EDGE('',*,*,#3624,.F.);
#5143=ORIENTED_EDGE('',*,*,#3625,.F.);
#5144=ORIENTED_EDGE('',*,*,#3626,.F.);
#5145=ORIENTED_EDGE('',*,*,#3627,.T.);
#5146=ORIENTED_EDGE('',*,*,#3619,.T.);
#5147=ORIENTED_EDGE('',*,*,#3620,.T.);
#5148=ORIENTED_EDGE('',*,*,#3627,.F.);
#5149=ORIENTED_EDGE('',*,*,#3628,.F.);
#5150=ORIENTED_EDGE('',*,*,#3629,.F.);
#5151=ORIENTED_EDGE('',*,*,#3630,.T.);
#5152=ORIENTED_EDGE('',*,*,#3631,.T.);
#5153=ORIENTED_EDGE('',*,*,#3632,.T.);
#5154=ORIENTED_EDGE('',*,*,#3630,.F.);
#5155=ORIENTED_EDGE('',*,*,#3625,.T.);
#5156=ORIENTED_EDGE('',*,*,#3626,.T.);
#5157=ORIENTED_EDGE('',*,*,#3633,.T.);
#5158=ORIENTED_EDGE('',*,*,#3631,.F.);
#5159=ORIENTED_EDGE('',*,*,#3632,.F.);
#5160=ORIENTED_EDGE('',*,*,#3633,.F.);
#5161=ORIENTED_EDGE('',*,*,#3634,.F.);
#5162=ORIENTED_EDGE('',*,*,#3635,.F.);
#5163=ORIENTED_EDGE('',*,*,#3636,.T.);
#5164=ORIENTED_EDGE('',*,*,#3628,.T.);
#5165=ORIENTED_EDGE('',*,*,#3629,.T.);
#5166=ORIENTED_EDGE('',*,*,#3636,.F.);
#5167=ORIENTED_EDGE('',*,*,#3637,.F.);
#5168=ORIENTED_EDGE('',*,*,#3638,.F.);
#5169=ORIENTED_EDGE('',*,*,#3639,.T.);
#5170=ORIENTED_EDGE('',*,*,#3640,.T.);
#5171=ORIENTED_EDGE('',*,*,#3641,.T.);
#5172=ORIENTED_EDGE('',*,*,#3639,.F.);
#5173=ORIENTED_EDGE('',*,*,#3634,.T.);
#5174=ORIENTED_EDGE('',*,*,#3635,.T.);
#5175=ORIENTED_EDGE('',*,*,#3642,.T.);
#5176=ORIENTED_EDGE('',*,*,#3640,.F.);
#5177=ORIENTED_EDGE('',*,*,#3641,.F.);
#5178=ORIENTED_EDGE('',*,*,#3642,.F.);
#5179=ORIENTED_EDGE('',*,*,#3643,.F.);
#5180=ORIENTED_EDGE('',*,*,#3644,.F.);
#5181=ORIENTED_EDGE('',*,*,#3645,.T.);
#5182=ORIENTED_EDGE('',*,*,#3637,.T.);
#5183=ORIENTED_EDGE('',*,*,#3638,.T.);
#5184=ORIENTED_EDGE('',*,*,#3645,.F.);
#5185=ORIENTED_EDGE('',*,*,#3646,.F.);
#5186=ORIENTED_EDGE('',*,*,#3647,.F.);
#5187=ORIENTED_EDGE('',*,*,#3648,.T.);
#5188=ORIENTED_EDGE('',*,*,#3649,.T.);
#5189=ORIENTED_EDGE('',*,*,#3650,.T.);
#5190=ORIENTED_EDGE('',*,*,#3648,.F.);
#5191=ORIENTED_EDGE('',*,*,#3643,.T.);
#5192=ORIENTED_EDGE('',*,*,#3644,.T.);
#5193=ORIENTED_EDGE('',*,*,#3651,.T.);
#5194=ORIENTED_EDGE('',*,*,#3649,.F.);
#5195=ORIENTED_EDGE('',*,*,#3650,.F.);
#5196=ORIENTED_EDGE('',*,*,#3651,.F.);
#5197=ORIENTED_EDGE('',*,*,#3652,.F.);
#5198=ORIENTED_EDGE('',*,*,#3653,.F.);
#5199=ORIENTED_EDGE('',*,*,#3654,.T.);
#5200=ORIENTED_EDGE('',*,*,#3646,.T.);
#5201=ORIENTED_EDGE('',*,*,#3647,.T.);
#5202=ORIENTED_EDGE('',*,*,#3654,.F.);
#5203=ORIENTED_EDGE('',*,*,#3655,.F.);
#5204=ORIENTED_EDGE('',*,*,#3656,.F.);
#5205=ORIENTED_EDGE('',*,*,#3657,.T.);
#5206=ORIENTED_EDGE('',*,*,#3658,.T.);
#5207=ORIENTED_EDGE('',*,*,#3659,.T.);
#5208=ORIENTED_EDGE('',*,*,#3657,.F.);
#5209=ORIENTED_EDGE('',*,*,#3652,.T.);
#5210=ORIENTED_EDGE('',*,*,#3653,.T.);
#5211=ORIENTED_EDGE('',*,*,#3660,.T.);
#5212=ORIENTED_EDGE('',*,*,#3658,.F.);
#5213=ORIENTED_EDGE('',*,*,#3659,.F.);
#5214=ORIENTED_EDGE('',*,*,#3660,.F.);
#5215=ORIENTED_EDGE('',*,*,#3661,.F.);
#5216=ORIENTED_EDGE('',*,*,#3662,.F.);
#5217=ORIENTED_EDGE('',*,*,#3663,.T.);
#5218=ORIENTED_EDGE('',*,*,#3655,.T.);
#5219=ORIENTED_EDGE('',*,*,#3656,.T.);
#5220=ORIENTED_EDGE('',*,*,#3663,.F.);
#5221=ORIENTED_EDGE('',*,*,#3664,.F.);
#5222=ORIENTED_EDGE('',*,*,#3665,.F.);
#5223=ORIENTED_EDGE('',*,*,#3666,.T.);
#5224=ORIENTED_EDGE('',*,*,#3667,.T.);
#5225=ORIENTED_EDGE('',*,*,#3668,.T.);
#5226=ORIENTED_EDGE('',*,*,#3666,.F.);
#5227=ORIENTED_EDGE('',*,*,#3661,.T.);
#5228=ORIENTED_EDGE('',*,*,#3662,.T.);
#5229=ORIENTED_EDGE('',*,*,#3669,.T.);
#5230=ORIENTED_EDGE('',*,*,#3667,.F.);
#5231=ORIENTED_EDGE('',*,*,#3668,.F.);
#5232=ORIENTED_EDGE('',*,*,#3669,.F.);
#5233=ORIENTED_EDGE('',*,*,#3670,.F.);
#5234=ORIENTED_EDGE('',*,*,#3671,.F.);
#5235=ORIENTED_EDGE('',*,*,#3672,.T.);
#5236=ORIENTED_EDGE('',*,*,#3664,.T.);
#5237=ORIENTED_EDGE('',*,*,#3665,.T.);
#5238=ORIENTED_EDGE('',*,*,#3672,.F.);
#5239=ORIENTED_EDGE('',*,*,#3673,.F.);
#5240=ORIENTED_EDGE('',*,*,#3674,.F.);
#5241=ORIENTED_EDGE('',*,*,#3675,.T.);
#5242=ORIENTED_EDGE('',*,*,#3676,.T.);
#5243=ORIENTED_EDGE('',*,*,#3677,.T.);
#5244=ORIENTED_EDGE('',*,*,#3675,.F.);
#5245=ORIENTED_EDGE('',*,*,#3670,.T.);
#5246=ORIENTED_EDGE('',*,*,#3671,.T.);
#5247=ORIENTED_EDGE('',*,*,#3678,.T.);
#5248=ORIENTED_EDGE('',*,*,#3676,.F.);
#5249=ORIENTED_EDGE('',*,*,#3677,.F.);
#5250=ORIENTED_EDGE('',*,*,#3678,.F.);
#5251=ORIENTED_EDGE('',*,*,#3679,.F.);
#5252=ORIENTED_EDGE('',*,*,#3680,.F.);
#5253=ORIENTED_EDGE('',*,*,#3681,.T.);
#5254=ORIENTED_EDGE('',*,*,#3673,.T.);
#5255=ORIENTED_EDGE('',*,*,#3674,.T.);
#5256=ORIENTED_EDGE('',*,*,#3681,.F.);
#5257=ORIENTED_EDGE('',*,*,#3682,.F.);
#5258=ORIENTED_EDGE('',*,*,#3683,.F.);
#5259=ORIENTED_EDGE('',*,*,#3684,.T.);
#5260=ORIENTED_EDGE('',*,*,#3685,.T.);
#5261=ORIENTED_EDGE('',*,*,#3686,.T.);
#5262=ORIENTED_EDGE('',*,*,#3684,.F.);
#5263=ORIENTED_EDGE('',*,*,#3679,.T.);
#5264=ORIENTED_EDGE('',*,*,#3680,.T.);
#5265=ORIENTED_EDGE('',*,*,#3687,.T.);
#5266=ORIENTED_EDGE('',*,*,#3685,.F.);
#5267=ORIENTED_EDGE('',*,*,#3686,.F.);
#5268=ORIENTED_EDGE('',*,*,#3687,.F.);
#5269=ORIENTED_EDGE('',*,*,#3688,.F.);
#5270=ORIENTED_EDGE('',*,*,#3689,.F.);
#5271=ORIENTED_EDGE('',*,*,#3690,.T.);
#5272=ORIENTED_EDGE('',*,*,#3682,.T.);
#5273=ORIENTED_EDGE('',*,*,#3683,.T.);
#5274=ORIENTED_EDGE('',*,*,#3690,.F.);
#5275=ORIENTED_EDGE('',*,*,#3691,.F.);
#5276=ORIENTED_EDGE('',*,*,#3692,.F.);
#5277=ORIENTED_EDGE('',*,*,#3693,.T.);
#5278=ORIENTED_EDGE('',*,*,#3694,.T.);
#5279=ORIENTED_EDGE('',*,*,#3695,.T.);
#5280=ORIENTED_EDGE('',*,*,#3693,.F.);
#5281=ORIENTED_EDGE('',*,*,#3688,.T.);
#5282=ORIENTED_EDGE('',*,*,#3689,.T.);
#5283=ORIENTED_EDGE('',*,*,#3696,.T.);
#5284=ORIENTED_EDGE('',*,*,#3694,.F.);
#5285=ORIENTED_EDGE('',*,*,#3695,.F.);
#5286=ORIENTED_EDGE('',*,*,#3696,.F.);
#5287=ORIENTED_EDGE('',*,*,#3697,.F.);
#5288=ORIENTED_EDGE('',*,*,#3698,.F.);
#5289=ORIENTED_EDGE('',*,*,#3699,.T.);
#5290=ORIENTED_EDGE('',*,*,#3691,.T.);
#5291=ORIENTED_EDGE('',*,*,#3692,.T.);
#5292=ORIENTED_EDGE('',*,*,#3699,.F.);
#5293=ORIENTED_EDGE('',*,*,#3700,.F.);
#5294=ORIENTED_EDGE('',*,*,#3701,.F.);
#5295=ORIENTED_EDGE('',*,*,#3702,.T.);
#5296=ORIENTED_EDGE('',*,*,#3703,.T.);
#5297=ORIENTED_EDGE('',*,*,#3704,.T.);
#5298=ORIENTED_EDGE('',*,*,#3702,.F.);
#5299=ORIENTED_EDGE('',*,*,#3697,.T.);
#5300=ORIENTED_EDGE('',*,*,#3698,.T.);
#5301=ORIENTED_EDGE('',*,*,#3705,.T.);
#5302=ORIENTED_EDGE('',*,*,#3703,.F.);
#5303=ORIENTED_EDGE('',*,*,#3704,.F.);
#5304=ORIENTED_EDGE('',*,*,#3705,.F.);
#5305=ORIENTED_EDGE('',*,*,#3706,.F.);
#5306=ORIENTED_EDGE('',*,*,#3707,.F.);
#5307=ORIENTED_EDGE('',*,*,#3708,.T.);
#5308=ORIENTED_EDGE('',*,*,#3700,.T.);
#5309=ORIENTED_EDGE('',*,*,#3701,.T.);
#5310=ORIENTED_EDGE('',*,*,#3708,.F.);
#5311=ORIENTED_EDGE('',*,*,#3709,.F.);
#5312=ORIENTED_EDGE('',*,*,#3710,.F.);
#5313=ORIENTED_EDGE('',*,*,#3711,.T.);
#5314=ORIENTED_EDGE('',*,*,#3712,.T.);
#5315=ORIENTED_EDGE('',*,*,#3713,.T.);
#5316=ORIENTED_EDGE('',*,*,#3711,.F.);
#5317=ORIENTED_EDGE('',*,*,#3706,.T.);
#5318=ORIENTED_EDGE('',*,*,#3707,.T.);
#5319=ORIENTED_EDGE('',*,*,#3714,.T.);
#5320=ORIENTED_EDGE('',*,*,#3712,.F.);
#5321=ORIENTED_EDGE('',*,*,#3713,.F.);
#5322=ORIENTED_EDGE('',*,*,#3714,.F.);
#5323=ORIENTED_EDGE('',*,*,#3715,.F.);
#5324=ORIENTED_EDGE('',*,*,#3716,.F.);
#5325=ORIENTED_EDGE('',*,*,#3717,.T.);
#5326=ORIENTED_EDGE('',*,*,#3709,.T.);
#5327=ORIENTED_EDGE('',*,*,#3710,.T.);
#5328=ORIENTED_EDGE('',*,*,#3717,.F.);
#5329=ORIENTED_EDGE('',*,*,#3718,.F.);
#5330=ORIENTED_EDGE('',*,*,#3719,.F.);
#5331=ORIENTED_EDGE('',*,*,#3720,.T.);
#5332=ORIENTED_EDGE('',*,*,#3721,.T.);
#5333=ORIENTED_EDGE('',*,*,#3722,.T.);
#5334=ORIENTED_EDGE('',*,*,#3720,.F.);
#5335=ORIENTED_EDGE('',*,*,#3715,.T.);
#5336=ORIENTED_EDGE('',*,*,#3716,.T.);
#5337=ORIENTED_EDGE('',*,*,#3723,.T.);
#5338=ORIENTED_EDGE('',*,*,#3721,.F.);
#5339=ORIENTED_EDGE('',*,*,#3722,.F.);
#5340=ORIENTED_EDGE('',*,*,#3723,.F.);
#5341=ORIENTED_EDGE('',*,*,#3724,.F.);
#5342=ORIENTED_EDGE('',*,*,#3725,.F.);
#5343=ORIENTED_EDGE('',*,*,#3726,.T.);
#5344=ORIENTED_EDGE('',*,*,#3718,.T.);
#5345=ORIENTED_EDGE('',*,*,#3719,.T.);
#5346=ORIENTED_EDGE('',*,*,#3726,.F.);
#5347=ORIENTED_EDGE('',*,*,#3727,.F.);
#5348=ORIENTED_EDGE('',*,*,#3728,.F.);
#5349=ORIENTED_EDGE('',*,*,#3729,.T.);
#5350=ORIENTED_EDGE('',*,*,#3730,.T.);
#5351=ORIENTED_EDGE('',*,*,#3731,.T.);
#5352=ORIENTED_EDGE('',*,*,#3729,.F.);
#5353=ORIENTED_EDGE('',*,*,#3724,.T.);
#5354=ORIENTED_EDGE('',*,*,#3725,.T.);
#5355=ORIENTED_EDGE('',*,*,#3732,.T.);
#5356=ORIENTED_EDGE('',*,*,#3730,.F.);
#5357=ORIENTED_EDGE('',*,*,#3731,.F.);
#5358=ORIENTED_EDGE('',*,*,#3732,.F.);
#5359=ORIENTED_EDGE('',*,*,#3733,.F.);
#5360=ORIENTED_EDGE('',*,*,#3734,.F.);
#5361=ORIENTED_EDGE('',*,*,#3735,.T.);
#5362=ORIENTED_EDGE('',*,*,#3727,.T.);
#5363=ORIENTED_EDGE('',*,*,#3728,.T.);
#5364=ORIENTED_EDGE('',*,*,#3735,.F.);
#5365=ORIENTED_EDGE('',*,*,#3736,.F.);
#5366=ORIENTED_EDGE('',*,*,#3737,.F.);
#5367=ORIENTED_EDGE('',*,*,#3738,.T.);
#5368=ORIENTED_EDGE('',*,*,#3739,.T.);
#5369=ORIENTED_EDGE('',*,*,#3740,.T.);
#5370=ORIENTED_EDGE('',*,*,#3738,.F.);
#5371=ORIENTED_EDGE('',*,*,#3733,.T.);
#5372=ORIENTED_EDGE('',*,*,#3734,.T.);
#5373=ORIENTED_EDGE('',*,*,#3741,.T.);
#5374=ORIENTED_EDGE('',*,*,#3739,.F.);
#5375=ORIENTED_EDGE('',*,*,#3740,.F.);
#5376=ORIENTED_EDGE('',*,*,#3741,.F.);
#5377=ORIENTED_EDGE('',*,*,#3742,.F.);
#5378=ORIENTED_EDGE('',*,*,#3743,.F.);
#5379=ORIENTED_EDGE('',*,*,#3744,.T.);
#5380=ORIENTED_EDGE('',*,*,#3745,.F.);
#5381=ORIENTED_EDGE('',*,*,#3744,.F.);
#5382=ORIENTED_EDGE('',*,*,#3746,.F.);
#5383=ORIENTED_EDGE('',*,*,#3747,.F.);
#5384=ORIENTED_EDGE('',*,*,#3748,.F.);
#5385=ORIENTED_EDGE('',*,*,#3749,.T.);
#5386=ORIENTED_EDGE('',*,*,#3750,.F.);
#5387=ORIENTED_EDGE('',*,*,#3749,.F.);
#5388=ORIENTED_EDGE('',*,*,#3751,.F.);
#5389=ORIENTED_EDGE('',*,*,#3752,.F.);
#5390=ORIENTED_EDGE('',*,*,#3753,.F.);
#5391=ORIENTED_EDGE('',*,*,#3742,.T.);
#5392=ORIENTED_EDGE('',*,*,#3743,.T.);
#5393=ORIENTED_EDGE('',*,*,#3754,.T.);
#5394=ORIENTED_EDGE('',*,*,#3736,.T.);
#5395=ORIENTED_EDGE('',*,*,#3737,.T.);
#5396=ORIENTED_EDGE('',*,*,#3754,.F.);
#5397=ORIENTED_EDGE('',*,*,#3750,.T.);
#5398=ORIENTED_EDGE('',*,*,#3745,.T.);
#5399=ORIENTED_EDGE('',*,*,#3755,.T.);
#5400=ORIENTED_EDGE('',*,*,#3751,.T.);
#5401=ORIENTED_EDGE('',*,*,#3756,.T.);
#5402=ORIENTED_EDGE('',*,*,#3757,.T.);
#5403=ORIENTED_EDGE('',*,*,#3758,.T.);
#5404=ORIENTED_EDGE('',*,*,#3752,.T.);
#5405=ORIENTED_EDGE('',*,*,#3759,.T.);
#5406=ORIENTED_EDGE('',*,*,#3760,.T.);
#5407=ORIENTED_EDGE('',*,*,#3753,.T.);
#5408=ORIENTED_EDGE('',*,*,#3761,.T.);
#5409=ORIENTED_EDGE('',*,*,#3762,.T.);
#5410=ORIENTED_EDGE('',*,*,#3746,.T.);
#5411=ORIENTED_EDGE('',*,*,#3763,.T.);
#5412=ORIENTED_EDGE('',*,*,#3764,.T.);
#5413=ORIENTED_EDGE('',*,*,#3747,.T.);
#5414=ORIENTED_EDGE('',*,*,#3765,.T.);
#5415=ORIENTED_EDGE('',*,*,#3766,.T.);
#5416=ORIENTED_EDGE('',*,*,#3748,.T.);
#5417=ORIENTED_EDGE('',*,*,#3767,.F.);
#5418=ORIENTED_EDGE('',*,*,#3768,.F.);
#5419=ORIENTED_EDGE('',*,*,#3769,.F.);
#5420=ORIENTED_EDGE('',*,*,#3770,.F.);
#5421=ORIENTED_EDGE('',*,*,#3771,.T.);
#5422=ORIENTED_EDGE('',*,*,#3772,.F.);
#5423=ORIENTED_EDGE('',*,*,#3773,.T.);
#5424=ORIENTED_EDGE('',*,*,#3774,.T.);
#5425=ORIENTED_EDGE('',*,*,#3772,.T.);
#5426=ORIENTED_EDGE('',*,*,#3775,.T.);
#5427=ORIENTED_EDGE('',*,*,#3776,.T.);
#5428=ORIENTED_EDGE('',*,*,#3771,.F.);
#5429=ORIENTED_EDGE('',*,*,#3777,.T.);
#5430=ORIENTED_EDGE('',*,*,#3770,.T.);
#5431=ORIENTED_EDGE('',*,*,#3778,.T.);
#5432=ORIENTED_EDGE('',*,*,#3779,.T.);
#5433=ORIENTED_EDGE('',*,*,#3769,.T.);
#5434=ORIENTED_EDGE('',*,*,#3780,.T.);
#5435=ORIENTED_EDGE('',*,*,#3781,.T.);
#5436=ORIENTED_EDGE('',*,*,#3782,.T.);
#5437=ORIENTED_EDGE('',*,*,#3767,.T.);
#5438=ORIENTED_EDGE('',*,*,#3783,.T.);
#5439=ORIENTED_EDGE('',*,*,#3768,.T.);
#5440=ORIENTED_EDGE('',*,*,#3784,.T.);
#5441=ORIENTED_EDGE('',*,*,#3766,.F.);
#5442=ORIENTED_EDGE('',*,*,#3785,.T.);
#5443=ORIENTED_EDGE('',*,*,#3784,.F.);
#5444=ORIENTED_EDGE('',*,*,#3782,.F.);
#5445=ORIENTED_EDGE('',*,*,#3786,.F.);
#5446=ORIENTED_EDGE('',*,*,#3756,.F.);
#5447=ORIENTED_EDGE('',*,*,#3764,.F.);
#5448=ORIENTED_EDGE('',*,*,#3787,.T.);
#5449=ORIENTED_EDGE('',*,*,#3780,.F.);
#5450=ORIENTED_EDGE('',*,*,#3783,.F.);
#5451=ORIENTED_EDGE('',*,*,#3785,.F.);
#5452=ORIENTED_EDGE('',*,*,#3765,.F.);
#5453=ORIENTED_EDGE('',*,*,#3762,.F.);
#5454=ORIENTED_EDGE('',*,*,#3788,.T.);
#5455=ORIENTED_EDGE('',*,*,#3778,.F.);
#5456=ORIENTED_EDGE('',*,*,#3779,.F.);
#5457=ORIENTED_EDGE('',*,*,#3787,.F.);
#5458=ORIENTED_EDGE('',*,*,#3763,.F.);
#5459=ORIENTED_EDGE('',*,*,#3760,.F.);
#5460=ORIENTED_EDGE('',*,*,#3789,.T.);
#5461=ORIENTED_EDGE('',*,*,#3775,.F.);
#5462=ORIENTED_EDGE('',*,*,#3777,.F.);
#5463=ORIENTED_EDGE('',*,*,#3788,.F.);
#5464=ORIENTED_EDGE('',*,*,#3761,.F.);
#5465=ORIENTED_EDGE('',*,*,#3758,.F.);
#5466=ORIENTED_EDGE('',*,*,#3790,.T.);
#5467=ORIENTED_EDGE('',*,*,#3773,.F.);
#5468=ORIENTED_EDGE('',*,*,#3776,.F.);
#5469=ORIENTED_EDGE('',*,*,#3789,.F.);
#5470=ORIENTED_EDGE('',*,*,#3759,.F.);
#5471=ORIENTED_EDGE('',*,*,#3755,.F.);
#5472=ORIENTED_EDGE('',*,*,#3786,.T.);
#5473=ORIENTED_EDGE('',*,*,#3781,.F.);
#5474=ORIENTED_EDGE('',*,*,#3774,.F.);
#5475=ORIENTED_EDGE('',*,*,#3790,.F.);
#5476=ORIENTED_EDGE('',*,*,#3757,.F.);
#5477=ORIENTED_EDGE('',*,*,#3609,.F.);
#5478=ORIENTED_EDGE('',*,*,#3791,.F.);
#5479=ORIENTED_EDGE('',*,*,#3792,.T.);
#5480=ORIENTED_EDGE('',*,*,#3793,.T.);
#5481=ORIENTED_EDGE('',*,*,#3792,.F.);
#5482=ORIENTED_EDGE('',*,*,#3794,.T.);
#5483=ORIENTED_EDGE('',*,*,#3795,.T.);
#5484=ORIENTED_EDGE('',*,*,#3796,.F.);
#5485=ORIENTED_EDGE('',*,*,#3797,.F.);
#5486=ORIENTED_EDGE('',*,*,#3798,.F.);
#5487=ORIENTED_EDGE('',*,*,#3799,.T.);
#5488=ORIENTED_EDGE('',*,*,#3800,.T.);
#5489=ORIENTED_EDGE('',*,*,#3799,.F.);
#5490=ORIENTED_EDGE('',*,*,#3801,.T.);
#5491=ORIENTED_EDGE('',*,*,#3802,.T.);
#5492=ORIENTED_EDGE('',*,*,#3803,.T.);
#5493=ORIENTED_EDGE('',*,*,#3804,.F.);
#5494=ORIENTED_EDGE('',*,*,#3805,.T.);
#5495=ORIENTED_EDGE('',*,*,#3806,.T.);
#5496=ORIENTED_EDGE('',*,*,#3801,.F.);
#5497=ORIENTED_EDGE('',*,*,#3807,.F.);
#5498=ORIENTED_EDGE('',*,*,#3803,.F.);
#5499=ORIENTED_EDGE('',*,*,#3808,.T.);
#5500=ORIENTED_EDGE('',*,*,#3809,.T.);
#5501=ORIENTED_EDGE('',*,*,#3810,.F.);
#5502=ORIENTED_EDGE('',*,*,#3811,.F.);
#5503=ORIENTED_EDGE('',*,*,#3805,.F.);
#5504=ORIENTED_EDGE('',*,*,#3812,.T.);
#5505=ORIENTED_EDGE('',*,*,#3809,.F.);
#5506=ORIENTED_EDGE('',*,*,#3813,.F.);
#5507=ORIENTED_EDGE('',*,*,#3814,.F.);
#5508=ORIENTED_EDGE('',*,*,#3815,.T.);
#5509=ORIENTED_EDGE('',*,*,#3816,.T.);
#5510=ORIENTED_EDGE('',*,*,#3817,.F.);
#5511=ORIENTED_EDGE('',*,*,#3818,.F.);
#5512=ORIENTED_EDGE('',*,*,#3815,.F.);
#5513=ORIENTED_EDGE('',*,*,#3819,.F.);
#5514=ORIENTED_EDGE('',*,*,#3798,.T.);
#5515=ORIENTED_EDGE('',*,*,#3818,.T.);
#5516=ORIENTED_EDGE('',*,*,#3820,.T.);
#5517=ORIENTED_EDGE('',*,*,#3821,.F.);
#5518=ORIENTED_EDGE('',*,*,#3816,.F.);
#5519=ORIENTED_EDGE('',*,*,#3821,.T.);
#5520=ORIENTED_EDGE('',*,*,#3822,.T.);
#5521=ORIENTED_EDGE('',*,*,#3823,.T.);
#5522=ORIENTED_EDGE('',*,*,#3813,.T.);
#5523=ORIENTED_EDGE('',*,*,#3800,.F.);
#5524=ORIENTED_EDGE('',*,*,#3823,.F.);
#5525=ORIENTED_EDGE('',*,*,#3824,.T.);
#5526=ORIENTED_EDGE('',*,*,#3819,.T.);
#5527=ORIENTED_EDGE('',*,*,#3814,.T.);
#5528=ORIENTED_EDGE('',*,*,#3807,.T.);
#5529=ORIENTED_EDGE('',*,*,#3825,.T.);
#5530=ORIENTED_EDGE('',*,*,#3820,.F.);
#5531=ORIENTED_EDGE('',*,*,#3826,.F.);
#5532=ORIENTED_EDGE('',*,*,#3824,.F.);
#5533=ORIENTED_EDGE('',*,*,#3827,.T.);
#5534=ORIENTED_EDGE('',*,*,#3810,.T.);
#5535=ORIENTED_EDGE('',*,*,#3828,.F.);
#5536=ORIENTED_EDGE('',*,*,#3828,.T.);
#5537=ORIENTED_EDGE('',*,*,#3812,.F.);
#5538=ORIENTED_EDGE('',*,*,#3826,.T.);
#5539=ORIENTED_EDGE('',*,*,#3817,.T.);
#5540=ORIENTED_EDGE('',*,*,#3827,.F.);
#5541=ORIENTED_EDGE('',*,*,#3822,.F.);
#5542=ORIENTED_EDGE('',*,*,#3825,.F.);
#5543=ORIENTED_EDGE('',*,*,#3804,.T.);
#5544=ORIENTED_EDGE('',*,*,#3829,.T.);
#5545=ORIENTED_EDGE('',*,*,#3830,.T.);
#5546=ORIENTED_EDGE('',*,*,#3806,.F.);
#5547=ORIENTED_EDGE('',*,*,#3831,.F.);
#5548=ORIENTED_EDGE('',*,*,#3808,.F.);
#5549=ORIENTED_EDGE('',*,*,#3832,.T.);
#5550=ORIENTED_EDGE('',*,*,#3833,.T.);
#5551=ORIENTED_EDGE('',*,*,#3834,.F.);
#5552=ORIENTED_EDGE('',*,*,#3834,.T.);
#5553=ORIENTED_EDGE('',*,*,#3835,.F.);
#5554=ORIENTED_EDGE('',*,*,#3831,.T.);
#5555=ORIENTED_EDGE('',*,*,#3811,.T.);
#5556=ORIENTED_EDGE('',*,*,#3832,.F.);
#5557=ORIENTED_EDGE('',*,*,#3802,.F.);
#5558=ORIENTED_EDGE('',*,*,#3830,.F.);
#5559=ORIENTED_EDGE('',*,*,#3836,.T.);
#5560=ORIENTED_EDGE('',*,*,#3837,.F.);
#5561=ORIENTED_EDGE('',*,*,#3835,.T.);
#5562=ORIENTED_EDGE('',*,*,#3838,.F.);
#5563=ORIENTED_EDGE('',*,*,#3794,.F.);
#5564=ORIENTED_EDGE('',*,*,#3791,.T.);
#5565=ORIENTED_EDGE('',*,*,#3833,.F.);
#5566=ORIENTED_EDGE('',*,*,#3839,.F.);
#5567=ORIENTED_EDGE('',*,*,#3795,.F.);
#5568=ORIENTED_EDGE('',*,*,#3838,.T.);
#5569=ORIENTED_EDGE('',*,*,#3836,.F.);
#5570=ORIENTED_EDGE('',*,*,#3840,.T.);
#5571=ORIENTED_EDGE('',*,*,#3796,.T.);
#5572=ORIENTED_EDGE('',*,*,#3839,.T.);
#5573=ORIENTED_EDGE('',*,*,#3793,.F.);
#5574=ORIENTED_EDGE('',*,*,#3829,.F.);
#5575=ORIENTED_EDGE('',*,*,#3837,.T.);
#5576=ORIENTED_EDGE('',*,*,#3797,.T.);
#5577=ORIENTED_EDGE('',*,*,#3840,.F.);
#5578=ORIENTED_EDGE('',*,*,#3841,.F.);
#5579=ORIENTED_EDGE('',*,*,#3842,.T.);
#5580=ORIENTED_EDGE('',*,*,#3843,.F.);
#5581=ORIENTED_EDGE('',*,*,#3844,.T.);
#5582=ORIENTED_EDGE('',*,*,#3845,.F.);
#5583=ORIENTED_EDGE('',*,*,#3846,.T.);
#5584=ORIENTED_EDGE('',*,*,#3847,.F.);
#5585=ORIENTED_EDGE('',*,*,#3848,.F.);
#5586=ORIENTED_EDGE('',*,*,#3849,.F.);
#5587=ORIENTED_EDGE('',*,*,#3850,.T.);
#5588=ORIENTED_EDGE('',*,*,#3851,.F.);
#5589=ORIENTED_EDGE('',*,*,#3852,.T.);
#5590=ORIENTED_EDGE('',*,*,#3853,.F.);
#5591=ORIENTED_EDGE('',*,*,#3854,.T.);
#5592=ORIENTED_EDGE('',*,*,#3855,.F.);
#5593=ORIENTED_EDGE('',*,*,#3856,.F.);
#5594=ORIENTED_EDGE('',*,*,#3857,.F.);
#5595=ORIENTED_EDGE('',*,*,#3858,.F.);
#5596=ORIENTED_EDGE('',*,*,#3859,.T.);
#5597=ORIENTED_EDGE('',*,*,#3860,.F.);
#5598=ORIENTED_EDGE('',*,*,#3859,.F.);
#5599=ORIENTED_EDGE('',*,*,#3861,.F.);
#5600=ORIENTED_EDGE('',*,*,#3862,.T.);
#5601=ORIENTED_EDGE('',*,*,#3863,.F.);
#5602=ORIENTED_EDGE('',*,*,#3862,.F.);
#5603=ORIENTED_EDGE('',*,*,#3864,.F.);
#5604=ORIENTED_EDGE('',*,*,#3865,.F.);
#5605=ORIENTED_EDGE('',*,*,#3866,.T.);
#5606=ORIENTED_EDGE('',*,*,#3867,.F.);
#5607=ORIENTED_EDGE('',*,*,#3866,.F.);
#5608=ORIENTED_EDGE('',*,*,#3868,.F.);
#5609=ORIENTED_EDGE('',*,*,#3869,.T.);
#5610=ORIENTED_EDGE('',*,*,#3870,.F.);
#5611=ORIENTED_EDGE('',*,*,#3869,.F.);
#5612=ORIENTED_EDGE('',*,*,#3871,.F.);
#5613=ORIENTED_EDGE('',*,*,#3872,.F.);
#5614=ORIENTED_EDGE('',*,*,#3873,.T.);
#5615=ORIENTED_EDGE('',*,*,#3874,.F.);
#5616=ORIENTED_EDGE('',*,*,#3873,.F.);
#5617=ORIENTED_EDGE('',*,*,#3875,.F.);
#5618=ORIENTED_EDGE('',*,*,#3876,.T.);
#5619=ORIENTED_EDGE('',*,*,#3877,.F.);
#5620=ORIENTED_EDGE('',*,*,#3876,.F.);
#5621=ORIENTED_EDGE('',*,*,#3878,.F.);
#5622=ORIENTED_EDGE('',*,*,#3879,.F.);
#5623=ORIENTED_EDGE('',*,*,#3880,.T.);
#5624=ORIENTED_EDGE('',*,*,#3881,.F.);
#5625=ORIENTED_EDGE('',*,*,#3880,.F.);
#5626=ORIENTED_EDGE('',*,*,#3882,.F.);
#5627=ORIENTED_EDGE('',*,*,#3883,.T.);
#5628=ORIENTED_EDGE('',*,*,#3884,.F.);
#5629=ORIENTED_EDGE('',*,*,#3883,.F.);
#5630=ORIENTED_EDGE('',*,*,#3885,.F.);
#5631=ORIENTED_EDGE('',*,*,#3886,.F.);
#5632=ORIENTED_EDGE('',*,*,#3887,.T.);
#5633=ORIENTED_EDGE('',*,*,#3888,.F.);
#5634=ORIENTED_EDGE('',*,*,#3887,.F.);
#5635=ORIENTED_EDGE('',*,*,#3889,.F.);
#5636=ORIENTED_EDGE('',*,*,#3890,.T.);
#5637=ORIENTED_EDGE('',*,*,#3891,.F.);
#5638=ORIENTED_EDGE('',*,*,#3890,.F.);
#5639=ORIENTED_EDGE('',*,*,#3885,.T.);
#5640=ORIENTED_EDGE('',*,*,#3886,.T.);
#5641=ORIENTED_EDGE('',*,*,#3892,.T.);
#5642=ORIENTED_EDGE('',*,*,#3889,.T.);
#5643=ORIENTED_EDGE('',*,*,#3892,.F.);
#5644=ORIENTED_EDGE('',*,*,#3878,.T.);
#5645=ORIENTED_EDGE('',*,*,#3879,.T.);
#5646=ORIENTED_EDGE('',*,*,#3893,.T.);
#5647=ORIENTED_EDGE('',*,*,#3882,.T.);
#5648=ORIENTED_EDGE('',*,*,#3893,.F.);
#5649=ORIENTED_EDGE('',*,*,#3871,.T.);
#5650=ORIENTED_EDGE('',*,*,#3872,.T.);
#5651=ORIENTED_EDGE('',*,*,#3894,.T.);
#5652=ORIENTED_EDGE('',*,*,#3875,.T.);
#5653=ORIENTED_EDGE('',*,*,#3894,.F.);
#5654=ORIENTED_EDGE('',*,*,#3864,.T.);
#5655=ORIENTED_EDGE('',*,*,#3865,.T.);
#5656=ORIENTED_EDGE('',*,*,#3895,.T.);
#5657=ORIENTED_EDGE('',*,*,#3868,.T.);
#5658=ORIENTED_EDGE('',*,*,#3895,.F.);
#5659=ORIENTED_EDGE('',*,*,#3857,.T.);
#5660=ORIENTED_EDGE('',*,*,#3858,.T.);
#5661=ORIENTED_EDGE('',*,*,#3896,.T.);
#5662=ORIENTED_EDGE('',*,*,#3861,.T.);
#5663=ORIENTED_EDGE('',*,*,#3896,.F.);
#5664=ORIENTED_EDGE('',*,*,#3897,.T.);
#5665=ORIENTED_EDGE('',*,*,#3898,.T.);
#5666=ORIENTED_EDGE('',*,*,#3899,.T.);
#5667=ORIENTED_EDGE('',*,*,#3900,.F.);
#5668=ORIENTED_EDGE('',*,*,#3901,.T.);
#5669=ORIENTED_EDGE('',*,*,#3902,.T.);
#5670=ORIENTED_EDGE('',*,*,#3903,.T.);
#5671=ORIENTED_EDGE('',*,*,#3904,.F.);
#5672=ORIENTED_EDGE('',*,*,#3905,.T.);
#5673=ORIENTED_EDGE('',*,*,#3841,.T.);
#5674=ORIENTED_EDGE('',*,*,#3906,.T.);
#5675=ORIENTED_EDGE('',*,*,#3907,.T.);
#5676=ORIENTED_EDGE('',*,*,#3908,.T.);
#5677=ORIENTED_EDGE('',*,*,#3847,.T.);
#5678=ORIENTED_EDGE('',*,*,#3909,.T.);
#5679=ORIENTED_EDGE('',*,*,#3910,.T.);
#5680=ORIENTED_EDGE('',*,*,#3911,.T.);
#5681=ORIENTED_EDGE('',*,*,#3888,.T.);
#5682=ORIENTED_EDGE('',*,*,#3881,.T.);
#5683=ORIENTED_EDGE('',*,*,#3874,.T.);
#5684=ORIENTED_EDGE('',*,*,#3867,.T.);
#5685=ORIENTED_EDGE('',*,*,#3860,.T.);
#5686=ORIENTED_EDGE('',*,*,#3912,.T.);
#5687=ORIENTED_EDGE('',*,*,#3851,.T.);
#5688=ORIENTED_EDGE('',*,*,#3913,.T.);
#5689=ORIENTED_EDGE('',*,*,#3914,.T.);
#5690=ORIENTED_EDGE('',*,*,#3915,.T.);
#5691=ORIENTED_EDGE('',*,*,#3916,.T.);
#5692=ORIENTED_EDGE('',*,*,#3853,.T.);
#5693=ORIENTED_EDGE('',*,*,#3917,.T.);
#5694=ORIENTED_EDGE('',*,*,#3918,.T.);
#5695=ORIENTED_EDGE('',*,*,#3891,.T.);
#5696=ORIENTED_EDGE('',*,*,#3884,.T.);
#5697=ORIENTED_EDGE('',*,*,#3877,.T.);
#5698=ORIENTED_EDGE('',*,*,#3870,.T.);
#5699=ORIENTED_EDGE('',*,*,#3863,.T.);
#5700=ORIENTED_EDGE('',*,*,#3919,.F.);
#5701=ORIENTED_EDGE('',*,*,#3920,.T.);
#5702=ORIENTED_EDGE('',*,*,#3904,.T.);
#5703=ORIENTED_EDGE('',*,*,#3921,.T.);
#5704=ORIENTED_EDGE('',*,*,#3919,.T.);
#5705=ORIENTED_EDGE('',*,*,#3855,.T.);
#5706=ORIENTED_EDGE('',*,*,#3922,.F.);
#5707=ORIENTED_EDGE('',*,*,#3845,.T.);
#5708=ORIENTED_EDGE('',*,*,#3922,.T.);
#5709=ORIENTED_EDGE('',*,*,#3923,.T.);
#5710=ORIENTED_EDGE('',*,*,#3924,.F.);
#5711=ORIENTED_EDGE('',*,*,#3925,.T.);
#5712=ORIENTED_EDGE('',*,*,#3924,.T.);
#5713=ORIENTED_EDGE('',*,*,#3926,.T.);
#5714=ORIENTED_EDGE('',*,*,#3898,.F.);
#5715=ORIENTED_EDGE('',*,*,#3927,.T.);
#5716=ORIENTED_EDGE('',*,*,#3900,.T.);
#5717=ORIENTED_EDGE('',*,*,#3928,.T.);
#5718=ORIENTED_EDGE('',*,*,#3929,.F.);
#5719=ORIENTED_EDGE('',*,*,#3930,.T.);
#5720=ORIENTED_EDGE('',*,*,#3929,.T.);
#5721=ORIENTED_EDGE('',*,*,#3849,.T.);
#5722=ORIENTED_EDGE('',*,*,#3931,.F.);
#5723=ORIENTED_EDGE('',*,*,#3843,.T.);
#5724=ORIENTED_EDGE('',*,*,#3931,.T.);
#5725=ORIENTED_EDGE('',*,*,#3932,.T.);
#5726=ORIENTED_EDGE('',*,*,#3902,.F.);
#5727=ORIENTED_EDGE('',*,*,#3933,.T.);
#5728=ORIENTED_EDGE('',*,*,#3934,.F.);
#5729=ORIENTED_EDGE('',*,*,#3923,.F.);
#5730=ORIENTED_EDGE('',*,*,#3854,.F.);
#5731=ORIENTED_EDGE('',*,*,#3916,.F.);
#5732=ORIENTED_EDGE('',*,*,#3934,.T.);
#5733=ORIENTED_EDGE('',*,*,#3915,.F.);
#5734=ORIENTED_EDGE('',*,*,#3935,.F.);
#5735=ORIENTED_EDGE('',*,*,#3926,.F.);
#5736=ORIENTED_EDGE('',*,*,#3856,.T.);
#5737=ORIENTED_EDGE('',*,*,#3921,.F.);
#5738=ORIENTED_EDGE('',*,*,#3936,.F.);
#5739=ORIENTED_EDGE('',*,*,#3917,.F.);
#5740=ORIENTED_EDGE('',*,*,#3935,.T.);
#5741=ORIENTED_EDGE('',*,*,#3914,.F.);
#5742=ORIENTED_EDGE('',*,*,#3937,.F.);
#5743=ORIENTED_EDGE('',*,*,#3899,.F.);
#5744=ORIENTED_EDGE('',*,*,#3936,.T.);
#5745=ORIENTED_EDGE('',*,*,#3903,.F.);
#5746=ORIENTED_EDGE('',*,*,#3938,.F.);
#5747=ORIENTED_EDGE('',*,*,#3918,.F.);
#5748=ORIENTED_EDGE('',*,*,#3937,.T.);
#5749=ORIENTED_EDGE('',*,*,#3913,.F.);
#5750=ORIENTED_EDGE('',*,*,#3850,.F.);
#5751=ORIENTED_EDGE('',*,*,#3928,.F.);
#5752=ORIENTED_EDGE('',*,*,#3938,.T.);
#5753=ORIENTED_EDGE('',*,*,#3932,.F.);
#5754=ORIENTED_EDGE('',*,*,#3852,.F.);
#5755=ORIENTED_EDGE('',*,*,#3912,.F.);
#5756=ORIENTED_EDGE('',*,*,#3939,.F.);
#5757=ORIENTED_EDGE('',*,*,#3909,.F.);
#5758=ORIENTED_EDGE('',*,*,#3846,.F.);
#5759=ORIENTED_EDGE('',*,*,#3925,.F.);
#5760=ORIENTED_EDGE('',*,*,#3939,.T.);
#5761=ORIENTED_EDGE('',*,*,#3927,.F.);
#5762=ORIENTED_EDGE('',*,*,#3940,.F.);
#5763=ORIENTED_EDGE('',*,*,#3910,.F.);
#5764=ORIENTED_EDGE('',*,*,#3848,.T.);
#5765=ORIENTED_EDGE('',*,*,#3908,.F.);
#5766=ORIENTED_EDGE('',*,*,#3941,.F.);
#5767=ORIENTED_EDGE('',*,*,#3920,.F.);
#5768=ORIENTED_EDGE('',*,*,#3940,.T.);
#5769=ORIENTED_EDGE('',*,*,#3897,.F.);
#5770=ORIENTED_EDGE('',*,*,#3942,.F.);
#5771=ORIENTED_EDGE('',*,*,#3911,.F.);
#5772=ORIENTED_EDGE('',*,*,#3941,.T.);
#5773=ORIENTED_EDGE('',*,*,#3907,.F.);
#5774=ORIENTED_EDGE('',*,*,#3943,.F.);
#5775=ORIENTED_EDGE('',*,*,#3901,.F.);
#5776=ORIENTED_EDGE('',*,*,#3942,.T.);
#5777=ORIENTED_EDGE('',*,*,#3930,.F.);
#5778=ORIENTED_EDGE('',*,*,#3842,.F.);
#5779=ORIENTED_EDGE('',*,*,#3905,.F.);
#5780=ORIENTED_EDGE('',*,*,#3943,.T.);
#5781=ORIENTED_EDGE('',*,*,#3906,.F.);
#5782=ORIENTED_EDGE('',*,*,#3844,.F.);
#5783=ORIENTED_EDGE('',*,*,#3933,.F.);
#5784=CYLINDRICAL_SURFACE('',#6397,8.326);
#5785=CYLINDRICAL_SURFACE('',#6400,8.326);
#5786=CYLINDRICAL_SURFACE('',#6401,8.326);
#5787=CYLINDRICAL_SURFACE('',#6402,8.326);
#5788=CYLINDRICAL_SURFACE('',#6403,8.326);
#5789=CYLINDRICAL_SURFACE('',#6404,8.326);
#5790=CYLINDRICAL_SURFACE('',#6405,8.326);
#5791=CYLINDRICAL_SURFACE('',#6406,8.326);
#5792=CYLINDRICAL_SURFACE('',#6407,8.326);
#5793=CYLINDRICAL_SURFACE('',#6408,8.326);
#5794=CYLINDRICAL_SURFACE('',#6409,8.326);
#5795=CYLINDRICAL_SURFACE('',#6410,8.326);
#5796=CYLINDRICAL_SURFACE('',#6411,8.326);
#5797=CYLINDRICAL_SURFACE('',#6412,8.326);
#5798=CYLINDRICAL_SURFACE('',#6413,8.326);
#5799=CYLINDRICAL_SURFACE('',#6414,8.326);
#5800=CYLINDRICAL_SURFACE('',#6415,8.326);
#5801=CYLINDRICAL_SURFACE('',#6416,8.326);
#5802=CYLINDRICAL_SURFACE('',#6417,8.326);
#5803=CYLINDRICAL_SURFACE('',#6418,8.326);
#5804=CYLINDRICAL_SURFACE('',#6419,8.326);
#5805=CYLINDRICAL_SURFACE('',#6420,8.326);
#5806=CYLINDRICAL_SURFACE('',#6437,5.);
#5807=CYLINDRICAL_SURFACE('',#6440,5.);
#5808=CYLINDRICAL_SURFACE('',#6442,5.);
#5809=CYLINDRICAL_SURFACE('',#6445,5.);
#5810=CYLINDRICAL_SURFACE('',#6460,8.326);
#5811=CYLINDRICAL_SURFACE('',#6461,3.2);
#5812=CYLINDRICAL_SURFACE('',#6464,3.2);
#5813=CYLINDRICAL_SURFACE('',#6467,3.2);
#5814=CYLINDRICAL_SURFACE('',#6470,19.05);
#5815=CYLINDRICAL_SURFACE('',#6497,3.);
#5816=CYLINDRICAL_SURFACE('',#6501,5.);
#5817=CYLINDRICAL_SURFACE('',#6514,3.);
#5818=CYLINDRICAL_SURFACE('',#6518,5.);
#5819=CYLINDRICAL_SURFACE('',#6531,3.00000000000001);
#5820=CYLINDRICAL_SURFACE('',#6535,5.00000000000001);
#5821=CYLINDRICAL_SURFACE('',#6547,6.35);
#5822=CYLINDRICAL_SURFACE('',#6549,6.35);
#5823=CYLINDRICAL_SURFACE('',#6551,6.35);
#5824=CYLINDRICAL_SURFACE('',#6553,6.35);
#5825=CYLINDRICAL_SURFACE('',#6555,6.35);
#5826=CYLINDRICAL_SURFACE('',#6557,6.35);
#5827=CYLINDRICAL_SURFACE('',#6576,2.);
#5828=CYLINDRICAL_SURFACE('',#6578,2.);
#5829=CYLINDRICAL_SURFACE('',#6580,2.);
#5830=CYLINDRICAL_SURFACE('',#6582,2.);
#5831=CYLINDRICAL_SURFACE('',#6584,2.);
#5832=CYLINDRICAL_SURFACE('',#6586,2.);
#5833=CYLINDRICAL_SURFACE('',#6591,1.);
#5834=CYLINDRICAL_SURFACE('',#6593,1.);
#5835=CYLINDRICAL_SURFACE('',#6599,1.);
#5836=CYLINDRICAL_SURFACE('',#6601,1.);
#5837=CYLINDRICAL_SURFACE('',#6607,1.);
#5838=CYLINDRICAL_SURFACE('',#6609,1.);
#5839=CYLINDRICAL_SURFACE('',#6612,5.);
#5840=CYLINDRICAL_SURFACE('',#6617,5.);
#5841=CYLINDRICAL_SURFACE('',#6618,5.);
#5842=CYLINDRICAL_SURFACE('',#6621,5.);
#5843=CYLINDRICAL_SURFACE('',#6626,5.);
#5844=CYLINDRICAL_SURFACE('',#6627,5.);
#5845=CYLINDRICAL_SURFACE('',#6630,5.);
#5846=CYLINDRICAL_SURFACE('',#6635,5.);
#5847=CYLINDRICAL_SURFACE('',#6636,5.);
#5848=CYLINDRICAL_SURFACE('',#6641,5.);
#5849=CYLINDRICAL_SURFACE('',#6644,5.);
#5850=CYLINDRICAL_SURFACE('',#6649,5.);
#5851=CYLINDRICAL_SURFACE('',#6650,5.);
#5852=CYLINDRICAL_SURFACE('',#6654,5.);
#5853=CYLINDRICAL_SURFACE('',#6659,1.);
#5854=CYLINDRICAL_SURFACE('',#6663,1.);
#5855=CYLINDRICAL_SURFACE('',#6667,1.);
#5856=CYLINDRICAL_SURFACE('',#6674,1.);
#5857=CYLINDRICAL_SURFACE('',#6678,1.);
#5858=CYLINDRICAL_SURFACE('',#6682,1.);
#5859=CYLINDRICAL_SURFACE('',#6689,1.);
#5860=CYLINDRICAL_SURFACE('',#6690,1.);
#5861=CYLINDRICAL_SURFACE('',#6694,1.);
#5862=CYLINDRICAL_SURFACE('',#6706,5.);
#5863=CYLINDRICAL_SURFACE('',#6708,7.4375);
#5864=CYLINDRICAL_SURFACE('',#6717,7.70000000000001);
#5865=CYLINDRICAL_SURFACE('',#6720,12.7);
#5866=CYLINDRICAL_SURFACE('',#6753,4.975);
#5867=CYLINDRICAL_SURFACE('',#6783,3.175);
#5868=CYLINDRICAL_SURFACE('',#6792,2.5527);
#5869=CYLINDRICAL_SURFACE('',#6793,2.5527);
#5870=CYLINDRICAL_SURFACE('',#6794,2.5527);
#5871=CYLINDRICAL_SURFACE('',#6795,2.5527);
#5872=CYLINDRICAL_SURFACE('',#6829,3.302);
#5873=CYLINDRICAL_SURFACE('',#6847,3.175);
#5874=CYLINDRICAL_SURFACE('',#6856,3.175);
#5875=CYLINDRICAL_SURFACE('',#6865,3.175);
#5876=CYLINDRICAL_SURFACE('',#6874,3.175);
#5877=CYLINDRICAL_SURFACE('',#6883,3.175);
#5878=CYLINDRICAL_SURFACE('',#6892,3.175);
#5879=CYLINDRICAL_SURFACE('',#6901,3.175);
#5880=CYLINDRICAL_SURFACE('',#6910,3.175);
#5881=CYLINDRICAL_SURFACE('',#6919,3.175);
#5882=CYLINDRICAL_SURFACE('',#6928,3.175);
#5883=CYLINDRICAL_SURFACE('',#6937,3.175);
#5884=CYLINDRICAL_SURFACE('',#6946,3.175);
#5885=CYLINDRICAL_SURFACE('',#6955,3.175);
#5886=CYLINDRICAL_SURFACE('',#6964,3.175);
#5887=CYLINDRICAL_SURFACE('',#6978,5.5626);
#5888=CYLINDRICAL_SURFACE('',#6986,3.175);
#5889=CYLINDRICAL_SURFACE('',#7015,3.175);
#5890=CYLINDRICAL_SURFACE('',#7018,7.94000000000001);
#5891=CYLINDRICAL_SURFACE('',#7021,3.175);
#5892=CYLINDRICAL_SURFACE('',#7028,7.94000000000001);
#5893=CYLINDRICAL_SURFACE('',#7041,7.0866);
#5894=CYLINDRICAL_SURFACE('',#7042,0.7366);
#5895=CYLINDRICAL_SURFACE('',#7049,0.7366);
#5896=CYLINDRICAL_SURFACE('',#7050,7.0866);
#5897=CYLINDRICAL_SURFACE('',#7109,3.49999999999999);
#5898=CYLINDRICAL_SURFACE('',#7110,3.49999999999999);
#5899=CYLINDRICAL_SURFACE('',#7111,3.5);
#5900=CYLINDRICAL_SURFACE('',#7112,3.5);
#5901=CYLINDRICAL_SURFACE('',#7113,3.5);
#5902=CYLINDRICAL_SURFACE('',#7114,3.);
#5903=CYLINDRICAL_SURFACE('',#7117,7.94);
#5904=CYLINDRICAL_SURFACE('',#7129,31.76);
#5905=CYLINDRICAL_SURFACE('',#7130,3.);
#5906=CYLINDRICAL_SURFACE('',#7135,15.88);
#5907=CYLINDRICAL_SURFACE('',#7139,0.500000000000002);
#5908=CYLINDRICAL_SURFACE('',#7141,0.5);
#5909=CYLINDRICAL_SURFACE('',#7147,0.499999999999991);
#5910=CYLINDRICAL_SURFACE('',#7148,0.5);
#5911=CYLINDRICAL_SURFACE('',#7151,0.500000000000002);
#5912=CYLINDRICAL_SURFACE('',#7153,0.5);
#5913=CYLINDRICAL_SURFACE('',#7159,0.499999999999989);
#5914=CYLINDRICAL_SURFACE('',#7160,0.5);
#5915=ADVANCED_FACE('',(#500),#5784,.F.);
#5916=ADVANCED_FACE('',(#501),#5785,.F.);
#5917=ADVANCED_FACE('',(#502),#5786,.F.);
#5918=ADVANCED_FACE('',(#503),#5787,.F.);
#5919=ADVANCED_FACE('',(#504),#5788,.F.);
#5920=ADVANCED_FACE('',(#505),#5789,.F.);
#5921=ADVANCED_FACE('',(#506),#5790,.F.);
#5922=ADVANCED_FACE('',(#507),#5791,.F.);
#5923=ADVANCED_FACE('',(#508),#5792,.F.);
#5924=ADVANCED_FACE('',(#509),#5793,.F.);
#5925=ADVANCED_FACE('',(#510),#5794,.F.);
#5926=ADVANCED_FACE('',(#511),#5795,.F.);
#5927=ADVANCED_FACE('',(#512),#5796,.F.);
#5928=ADVANCED_FACE('',(#513),#5797,.F.);
#5929=ADVANCED_FACE('',(#514),#5798,.F.);
#5930=ADVANCED_FACE('',(#515),#5799,.F.);
#5931=ADVANCED_FACE('',(#516),#5800,.F.);
#5932=ADVANCED_FACE('',(#517),#5801,.F.);
#5933=ADVANCED_FACE('',(#518),#5802,.F.);
#5934=ADVANCED_FACE('',(#519),#5803,.F.);
#5935=ADVANCED_FACE('',(#520),#5804,.F.);
#5936=ADVANCED_FACE('',(#521),#5805,.F.);
#5937=ADVANCED_FACE('',(#522),#463,.T.);
#5938=ADVANCED_FACE('',(#523),#464,.T.);
#5939=ADVANCED_FACE('',(#524),#465,.T.);
#5940=ADVANCED_FACE('',(#525),#5806,.T.);
#5941=ADVANCED_FACE('',(#526),#5807,.T.);
#5942=ADVANCED_FACE('',(#527),#5808,.T.);
#5943=ADVANCED_FACE('',(#528),#5809,.T.);
#5944=ADVANCED_FACE('',(#529),#369,.F.);
#5945=ADVANCED_FACE('',(#530),#466,.F.);
#5946=ADVANCED_FACE('',(#531),#467,.F.);
#5947=ADVANCED_FACE('',(#532),#468,.F.);
#5948=ADVANCED_FACE('',(#533),#5810,.F.);
#5949=ADVANCED_FACE('',(#534),#5811,.F.);
#5950=ADVANCED_FACE('',(#535),#5812,.F.);
#5951=ADVANCED_FACE('',(#536),#5813,.F.);
#5952=ADVANCED_FACE('',(#537,#335,#336),#5814,.T.);
#5953=ADVANCED_FACE('',(#538,#337),#249,.T.);
#5954=ADVANCED_FACE('',(#539),#250,.T.);
#5955=ADVANCED_FACE('',(#540),#251,.T.);
#5956=ADVANCED_FACE('',(#541),#252,.T.);
#5957=ADVANCED_FACE('',(#542),#253,.T.);
#5958=ADVANCED_FACE('',(#543),#254,.T.);
#5959=ADVANCED_FACE('',(#544),#255,.T.);
#5960=ADVANCED_FACE('',(#545,#338),#256,.F.);
#5961=ADVANCED_FACE('',(#546),#370,.F.);
#5962=ADVANCED_FACE('',(#547,#339),#257,.F.);
#5963=ADVANCED_FACE('',(#548,#340),#258,.T.);
#5964=ADVANCED_FACE('',(#549),#259,.F.);
#5965=ADVANCED_FACE('',(#550),#5815,.T.);
#5966=ADVANCED_FACE('',(#551),#260,.F.);
#5967=ADVANCED_FACE('',(#552),#5816,.T.);
#5968=ADVANCED_FACE('',(#553),#261,.F.);
#5969=ADVANCED_FACE('',(#554),#262,.F.);
#5970=ADVANCED_FACE('',(#555,#341),#263,.F.);
#5971=ADVANCED_FACE('',(#556),#264,.F.);
#5972=ADVANCED_FACE('',(#557),#5817,.T.);
#5973=ADVANCED_FACE('',(#558),#265,.F.);
#5974=ADVANCED_FACE('',(#559),#5818,.T.);
#5975=ADVANCED_FACE('',(#560),#266,.F.);
#5976=ADVANCED_FACE('',(#561),#267,.F.);
#5977=ADVANCED_FACE('',(#562,#342),#268,.T.);
#5978=ADVANCED_FACE('',(#563,#343),#269,.F.);
#5979=ADVANCED_FACE('',(#564),#270,.F.);
#5980=ADVANCED_FACE('',(#565),#5819,.T.);
#5981=ADVANCED_FACE('',(#566),#271,.F.);
#5982=ADVANCED_FACE('',(#567),#5820,.T.);
#5983=ADVANCED_FACE('',(#568),#272,.F.);
#5984=ADVANCED_FACE('',(#569),#273,.F.);
#5985=ADVANCED_FACE('',(#570,#344),#274,.T.);
#5986=ADVANCED_FACE('',(#571),#5821,.F.);
#5987=ADVANCED_FACE('',(#572),#5822,.F.);
#5988=ADVANCED_FACE('',(#573),#5823,.F.);
#5989=ADVANCED_FACE('',(#574),#5824,.F.);
#5990=ADVANCED_FACE('',(#575),#5825,.F.);
#5991=ADVANCED_FACE('',(#576),#5826,.F.);
#5992=ADVANCED_FACE('',(#577),#469,.F.);
#5993=ADVANCED_FACE('',(#578),#470,.F.);
#5994=ADVANCED_FACE('',(#579),#471,.F.);
#5995=ADVANCED_FACE('',(#580),#275,.T.);
#5996=ADVANCED_FACE('',(#581),#148,.T.);
#5997=ADVANCED_FACE('',(#582),#149,.T.);
#5998=ADVANCED_FACE('',(#583),#150,.T.);
#5999=ADVANCED_FACE('',(#584),#151,.T.);
#6000=ADVANCED_FACE('',(#585,#345),#276,.T.);
#6001=ADVANCED_FACE('',(#586),#371,.T.);
#6002=ADVANCED_FACE('',(#587),#372,.T.);
#6003=ADVANCED_FACE('',(#588),#373,.T.);
#6004=ADVANCED_FACE('',(#589),#374,.T.);
#6005=ADVANCED_FACE('',(#590),#375,.T.);
#6006=ADVANCED_FACE('',(#591),#376,.T.);
#6007=ADVANCED_FACE('',(#592),#5827,.T.);
#6008=ADVANCED_FACE('',(#593),#5828,.T.);
#6009=ADVANCED_FACE('',(#594),#5829,.T.);
#6010=ADVANCED_FACE('',(#595),#5830,.T.);
#6011=ADVANCED_FACE('',(#596),#5831,.T.);
#6012=ADVANCED_FACE('',(#597),#5832,.T.);
#6013=ADVANCED_FACE('',(#598),#472,.F.);
#6014=ADVANCED_FACE('',(#599),#5833,.F.);
#6015=ADVANCED_FACE('',(#600),#5834,.F.);
#6016=ADVANCED_FACE('',(#601),#473,.F.);
#6017=ADVANCED_FACE('',(#602),#474,.F.);
#6018=ADVANCED_FACE('',(#603),#5835,.F.);
#6019=ADVANCED_FACE('',(#604),#5836,.F.);
#6020=ADVANCED_FACE('',(#605),#475,.F.);
#6021=ADVANCED_FACE('',(#606),#476,.F.);
#6022=ADVANCED_FACE('',(#607),#5837,.F.);
#6023=ADVANCED_FACE('',(#608),#5838,.F.);
#6024=ADVANCED_FACE('',(#609),#477,.F.);
#6025=ADVANCED_FACE('',(#610),#5839,.T.);
#6026=ADVANCED_FACE('',(#611),#139,.T.);
#6027=ADVANCED_FACE('',(#612),#5840,.T.);
#6028=ADVANCED_FACE('',(#613),#152,.T.);
#6029=ADVANCED_FACE('',(#614),#5841,.T.);
#6030=ADVANCED_FACE('',(#615),#153,.T.);
#6031=ADVANCED_FACE('',(#616),#154,.T.);
#6032=ADVANCED_FACE('',(#617),#5842,.T.);
#6033=ADVANCED_FACE('',(#618),#140,.T.);
#6034=ADVANCED_FACE('',(#619),#5843,.T.);
#6035=ADVANCED_FACE('',(#620),#155,.T.);
#6036=ADVANCED_FACE('',(#621),#5844,.T.);
#6037=ADVANCED_FACE('',(#622),#156,.T.);
#6038=ADVANCED_FACE('',(#623),#157,.T.);
#6039=ADVANCED_FACE('',(#624),#5845,.T.);
#6040=ADVANCED_FACE('',(#625),#141,.T.);
#6041=ADVANCED_FACE('',(#626),#5846,.T.);
#6042=ADVANCED_FACE('',(#627),#158,.T.);
#6043=ADVANCED_FACE('',(#628),#5847,.T.);
#6044=ADVANCED_FACE('',(#629),#159,.T.);
#6045=ADVANCED_FACE('',(#630),#160,.T.);
#6046=ADVANCED_FACE('',(#631),#161,.T.);
#6047=ADVANCED_FACE('',(#632),#162,.T.);
#6048=ADVANCED_FACE('',(#633),#5848,.T.);
#6049=ADVANCED_FACE('',(#634),#163,.T.);
#6050=ADVANCED_FACE('',(#635),#142,.T.);
#6051=ADVANCED_FACE('',(#636),#143,.T.);
#6052=ADVANCED_FACE('',(#637),#164,.T.);
#6053=ADVANCED_FACE('',(#638),#5849,.T.);
#6054=ADVANCED_FACE('',(#639),#165,.T.);
#6055=ADVANCED_FACE('',(#640),#166,.T.);
#6056=ADVANCED_FACE('',(#641),#167,.T.);
#6057=ADVANCED_FACE('',(#642),#168,.T.);
#6058=ADVANCED_FACE('',(#643),#5850,.T.);
#6059=ADVANCED_FACE('',(#644),#169,.T.);
#6060=ADVANCED_FACE('',(#645),#5851,.T.);
#6061=ADVANCED_FACE('',(#646),#144,.T.);
#6062=ADVANCED_FACE('',(#647),#5852,.T.);
#6063=ADVANCED_FACE('',(#648),#170,.T.);
#6064=ADVANCED_FACE('',(#649),#478,.T.);
#6065=ADVANCED_FACE('',(#650),#5853,.T.);
#6066=ADVANCED_FACE('',(#651),#479,.T.);
#6067=ADVANCED_FACE('',(#652),#5854,.T.);
#6068=ADVANCED_FACE('',(#653),#480,.T.);
#6069=ADVANCED_FACE('',(#654),#5855,.T.);
#6070=ADVANCED_FACE('',(#655),#481,.T.);
#6071=ADVANCED_FACE('',(#656),#171,.T.);
#6072=ADVANCED_FACE('',(#657),#172,.T.);
#6073=ADVANCED_FACE('',(#658),#482,.T.);
#6074=ADVANCED_FACE('',(#659),#5856,.T.);
#6075=ADVANCED_FACE('',(#660),#483,.T.);
#6076=ADVANCED_FACE('',(#661),#5857,.T.);
#6077=ADVANCED_FACE('',(#662),#484,.T.);
#6078=ADVANCED_FACE('',(#663),#5858,.T.);
#6079=ADVANCED_FACE('',(#664),#485,.T.);
#6080=ADVANCED_FACE('',(#665),#173,.T.);
#6081=ADVANCED_FACE('',(#666),#174,.T.);
#6082=ADVANCED_FACE('',(#667),#486,.T.);
#6083=ADVANCED_FACE('',(#668),#5859,.T.);
#6084=ADVANCED_FACE('',(#669),#5860,.T.);
#6085=ADVANCED_FACE('',(#670),#487,.T.);
#6086=ADVANCED_FACE('',(#671),#5861,.T.);
#6087=ADVANCED_FACE('',(#672),#488,.T.);
#6088=ADVANCED_FACE('',(#673),#175,.T.);
#6089=ADVANCED_FACE('',(#674),#176,.T.);
#6090=ADVANCED_FACE('',(#675),#177,.T.);
#6091=ADVANCED_FACE('',(#676),#377,.T.);
#6092=ADVANCED_FACE('',(#677),#5862,.F.);
#6093=ADVANCED_FACE('',(#678),#5863,.T.);
#6094=ADVANCED_FACE('',(#679),#378,.T.);
#6095=ADVANCED_FACE('',(#680),#379,.T.);
#6096=ADVANCED_FACE('',(#681),#5864,.T.);
#6097=ADVANCED_FACE('',(#682,#346),#5865,.T.);
#6098=ADVANCED_FACE('',(#683,#347),#277,.F.);
#6099=ADVANCED_FACE('',(#684,#348),#278,.F.);
#6100=ADVANCED_FACE('',(#685),#178,.F.);
#6101=ADVANCED_FACE('',(#686),#179,.F.);
#6102=ADVANCED_FACE('',(#687),#180,.F.);
#6103=ADVANCED_FACE('',(#688,#349),#279,.F.);
#6104=ADVANCED_FACE('',(#689),#280,.T.);
#6105=ADVANCED_FACE('',(#690),#281,.T.);
#6106=ADVANCED_FACE('',(#691),#282,.T.);
#6107=ADVANCED_FACE('',(#692),#283,.T.);
#6108=ADVANCED_FACE('',(#693),#284,.T.);
#6109=ADVANCED_FACE('',(#694),#285,.T.);
#6110=ADVANCED_FACE('',(#695,#350),#286,.T.);
#6111=ADVANCED_FACE('',(#696),#380,.T.);
#6112=ADVANCED_FACE('',(#697),#381,.T.);
#6113=ADVANCED_FACE('',(#698),#382,.T.);
#6114=ADVANCED_FACE('',(#699),#383,.T.);
#6115=ADVANCED_FACE('',(#700),#384,.T.);
#6116=ADVANCED_FACE('',(#701),#287,.F.);
#6117=ADVANCED_FACE('',(#702),#181,.T.);
#6118=ADVANCED_FACE('',(#703),#182,.T.);
#6119=ADVANCED_FACE('',(#704),#145,.T.);
#6120=ADVANCED_FACE('',(#705),#146,.T.);
#6121=ADVANCED_FACE('',(#706),#5866,.T.);
#6122=ADVANCED_FACE('',(#707),#385,.F.);
#6123=ADVANCED_FACE('',(#708),#386,.F.);
#6124=ADVANCED_FACE('',(#709),#387,.F.);
#6125=ADVANCED_FACE('',(#710),#388,.F.);
#6126=ADVANCED_FACE('',(#711),#389,.F.);
#6127=ADVANCED_FACE('',(#712),#390,.F.);
#6128=ADVANCED_FACE('',(#713),#391,.F.);
#6129=ADVANCED_FACE('',(#714),#392,.F.);
#6130=ADVANCED_FACE('',(#715),#5867,.F.);
#6131=ADVANCED_FACE('',(#716),#393,.F.);
#6132=ADVANCED_FACE('',(#717),#394,.F.);
#6133=ADVANCED_FACE('',(#718),#5868,.F.);
#6134=ADVANCED_FACE('',(#719),#5869,.F.);
#6135=ADVANCED_FACE('',(#720),#5870,.F.);
#6136=ADVANCED_FACE('',(#721),#5871,.F.);
#6137=ADVANCED_FACE('',(#722),#288,.T.);
#6138=ADVANCED_FACE('',(#723),#289,.T.);
#6139=ADVANCED_FACE('',(#724),#290,.F.);
#6140=ADVANCED_FACE('',(#725),#291,.T.);
#6141=ADVANCED_FACE('',(#726),#292,.T.);
#6142=ADVANCED_FACE('',(#727),#293,.T.);
#6143=ADVANCED_FACE('',(#728,#351),#294,.T.);
#6144=ADVANCED_FACE('',(#729,#352),#295,.F.);
#6145=ADVANCED_FACE('',(#730),#395,.T.);
#6146=ADVANCED_FACE('',(#731),#396,.T.);
#6147=ADVANCED_FACE('',(#732),#397,.T.);
#6148=ADVANCED_FACE('',(#733),#398,.T.);
#6149=ADVANCED_FACE('',(#734),#399,.T.);
#6150=ADVANCED_FACE('',(#735),#400,.T.);
#6151=ADVANCED_FACE('',(#736),#401,.T.);
#6152=ADVANCED_FACE('',(#737),#402,.T.);
#6153=ADVANCED_FACE('',(#738),#403,.T.);
#6154=ADVANCED_FACE('',(#739),#404,.T.);
#6155=ADVANCED_FACE('',(#740),#405,.T.);
#6156=ADVANCED_FACE('',(#741),#406,.T.);
#6157=ADVANCED_FACE('',(#742),#5872,.T.);
#6158=ADVANCED_FACE('',(#743),#147,.T.);
#6159=ADVANCED_FACE('',(#744),#296,.T.);
#6160=ADVANCED_FACE('',(#745,#353),#297,.T.);
#6161=ADVANCED_FACE('',(#746),#407,.T.);
#6162=ADVANCED_FACE('',(#747),#408,.T.);
#6163=ADVANCED_FACE('',(#748),#409,.T.);
#6164=ADVANCED_FACE('',(#749),#5873,.T.);
#6165=ADVANCED_FACE('',(#750),#410,.T.);
#6166=ADVANCED_FACE('',(#751),#411,.T.);
#6167=ADVANCED_FACE('',(#752),#5874,.T.);
#6168=ADVANCED_FACE('',(#753),#412,.T.);
#6169=ADVANCED_FACE('',(#754),#413,.T.);
#6170=ADVANCED_FACE('',(#755),#5875,.T.);
#6171=ADVANCED_FACE('',(#756),#414,.T.);
#6172=ADVANCED_FACE('',(#757),#415,.T.);
#6173=ADVANCED_FACE('',(#758),#5876,.T.);
#6174=ADVANCED_FACE('',(#759),#416,.T.);
#6175=ADVANCED_FACE('',(#760),#417,.T.);
#6176=ADVANCED_FACE('',(#761),#5877,.T.);
#6177=ADVANCED_FACE('',(#762),#418,.T.);
#6178=ADVANCED_FACE('',(#763),#419,.T.);
#6179=ADVANCED_FACE('',(#764),#5878,.T.);
#6180=ADVANCED_FACE('',(#765),#420,.T.);
#6181=ADVANCED_FACE('',(#766),#421,.T.);
#6182=ADVANCED_FACE('',(#767),#5879,.T.);
#6183=ADVANCED_FACE('',(#768),#422,.T.);
#6184=ADVANCED_FACE('',(#769),#423,.T.);
#6185=ADVANCED_FACE('',(#770),#5880,.T.);
#6186=ADVANCED_FACE('',(#771),#424,.T.);
#6187=ADVANCED_FACE('',(#772),#425,.T.);
#6188=ADVANCED_FACE('',(#773),#5881,.T.);
#6189=ADVANCED_FACE('',(#774),#426,.T.);
#6190=ADVANCED_FACE('',(#775),#427,.T.);
#6191=ADVANCED_FACE('',(#776),#5882,.T.);
#6192=ADVANCED_FACE('',(#777),#428,.T.);
#6193=ADVANCED_FACE('',(#778),#429,.T.);
#6194=ADVANCED_FACE('',(#779),#5883,.T.);
#6195=ADVANCED_FACE('',(#780),#430,.T.);
#6196=ADVANCED_FACE('',(#781),#431,.T.);
#6197=ADVANCED_FACE('',(#782),#5884,.T.);
#6198=ADVANCED_FACE('',(#783),#432,.T.);
#6199=ADVANCED_FACE('',(#784),#433,.T.);
#6200=ADVANCED_FACE('',(#785),#5885,.T.);
#6201=ADVANCED_FACE('',(#786),#434,.T.);
#6202=ADVANCED_FACE('',(#787),#435,.T.);
#6203=ADVANCED_FACE('',(#788),#5886,.T.);
#6204=ADVANCED_FACE('',(#789),#436,.T.);
#6205=ADVANCED_FACE('',(#790),#437,.T.);
#6206=ADVANCED_FACE('',(#791),#489,.F.);
#6207=ADVANCED_FACE('',(#792),#5887,.T.);
#6208=ADVANCED_FACE('',(#793),#5888,.T.);
#6209=ADVANCED_FACE('',(#794,#354),#298,.T.);
#6210=ADVANCED_FACE('',(#795),#299,.T.);
#6211=ADVANCED_FACE('',(#796),#300,.T.);
#6212=ADVANCED_FACE('',(#797),#301,.T.);
#6213=ADVANCED_FACE('',(#798),#302,.T.);
#6214=ADVANCED_FACE('',(#799),#303,.T.);
#6215=ADVANCED_FACE('',(#800),#304,.T.);
#6216=ADVANCED_FACE('',(#801),#305,.F.);
#6217=ADVANCED_FACE('',(#802),#438,.T.);
#6218=ADVANCED_FACE('',(#803),#439,.T.);
#6219=ADVANCED_FACE('',(#804),#440,.T.);
#6220=ADVANCED_FACE('',(#805),#441,.T.);
#6221=ADVANCED_FACE('',(#806),#442,.T.);
#6222=ADVANCED_FACE('',(#807),#443,.T.);
#6223=ADVANCED_FACE('',(#808),#306,.F.);
#6224=ADVANCED_FACE('',(#809),#307,.F.);
#6225=ADVANCED_FACE('',(#810),#308,.F.);
#6226=ADVANCED_FACE('',(#811),#309,.F.);
#6227=ADVANCED_FACE('',(#812),#310,.F.);
#6228=ADVANCED_FACE('',(#813),#311,.F.);
#6229=ADVANCED_FACE('',(#814),#312,.F.);
#6230=ADVANCED_FACE('',(#815),#5889,.F.);
#6231=ADVANCED_FACE('',(#816),#5890,.T.);
#6232=ADVANCED_FACE('',(#817),#5891,.F.);
#6233=ADVANCED_FACE('',(#818),#313,.T.);
#6234=ADVANCED_FACE('',(#819),#314,.T.);
#6235=ADVANCED_FACE('',(#820),#315,.T.);
#6236=ADVANCED_FACE('',(#821),#316,.F.);
#6237=ADVANCED_FACE('',(#822),#5892,.T.);
#6238=ADVANCED_FACE('',(#823,#355),#317,.F.);
#6239=ADVANCED_FACE('',(#824),#318,.T.);
#6240=ADVANCED_FACE('',(#825,#356),#319,.T.);
#6241=ADVANCED_FACE('',(#826),#320,.T.);
#6242=ADVANCED_FACE('',(#827),#321,.T.);
#6243=ADVANCED_FACE('',(#828),#322,.T.);
#6244=ADVANCED_FACE('',(#829),#5893,.T.);
#6245=ADVANCED_FACE('',(#830),#5894,.F.);
#6246=ADVANCED_FACE('',(#831),#323,.F.);
#6247=ADVANCED_FACE('',(#832),#324,.F.);
#6248=ADVANCED_FACE('',(#833),#5895,.F.);
#6249=ADVANCED_FACE('',(#834),#5896,.T.);
#6250=ADVANCED_FACE('',(#835,#357),#325,.F.);
#6251=ADVANCED_FACE('',(#836),#326,.T.);
#6252=ADVANCED_FACE('',(#837,#358),#327,.T.);
#6253=ADVANCED_FACE('',(#838),#328,.T.);
#6254=ADVANCED_FACE('',(#839),#490,.T.);
#6255=ADVANCED_FACE('',(#840),#491,.T.);
#6256=ADVANCED_FACE('',(#841),#492,.T.);
#6257=ADVANCED_FACE('',(#842),#493,.T.);
#6258=ADVANCED_FACE('',(#843),#444,.F.);
#6259=ADVANCED_FACE('',(#844),#445,.F.);
#6260=ADVANCED_FACE('',(#845),#446,.F.);
#6261=ADVANCED_FACE('',(#846),#447,.F.);
#6262=ADVANCED_FACE('',(#847),#448,.F.);
#6263=ADVANCED_FACE('',(#848),#449,.F.);
#6264=ADVANCED_FACE('',(#849),#450,.F.);
#6265=ADVANCED_FACE('',(#850),#451,.F.);
#6266=ADVANCED_FACE('',(#851),#452,.F.);
#6267=ADVANCED_FACE('',(#852),#453,.F.);
#6268=ADVANCED_FACE('',(#853),#5897,.F.);
#6269=ADVANCED_FACE('',(#854),#5898,.F.);
#6270=ADVANCED_FACE('',(#855),#5899,.F.);
#6271=ADVANCED_FACE('',(#856),#5900,.F.);
#6272=ADVANCED_FACE('',(#857),#5901,.F.);
#6273=ADVANCED_FACE('',(#858),#5902,.T.);
#6274=ADVANCED_FACE('',(#859),#5903,.T.);
#6275=ADVANCED_FACE('',(#860,#359,#360,#361,#362,#363),#329,.T.);
#6276=ADVANCED_FACE('',(#861,#364,#365,#366,#367,#368),#330,.F.);
#6277=ADVANCED_FACE('',(#862),#331,.F.);
#6278=ADVANCED_FACE('',(#863),#5904,.T.);
#6279=ADVANCED_FACE('',(#864),#5905,.T.);
#6280=ADVANCED_FACE('',(#865),#332,.F.);
#6281=ADVANCED_FACE('',(#866),#333,.F.);
#6282=ADVANCED_FACE('',(#867),#5906,.F.);
#6283=ADVANCED_FACE('',(#868),#334,.F.);
#6284=ADVANCED_FACE('',(#869),#494,.T.);
#6285=ADVANCED_FACE('',(#870),#5907,.T.);
#6286=ADVANCED_FACE('',(#871),#5908,.T.);
#6287=ADVANCED_FACE('',(#872),#495,.T.);
#6288=ADVANCED_FACE('',(#873),#496,.T.);
#6289=ADVANCED_FACE('',(#874),#5909,.T.);
#6290=ADVANCED_FACE('',(#875),#5910,.T.);
#6291=ADVANCED_FACE('',(#876),#497,.T.);
#6292=ADVANCED_FACE('',(#877),#5911,.T.);
#6293=ADVANCED_FACE('',(#878),#5912,.T.);
#6294=ADVANCED_FACE('',(#879),#498,.T.);
#6295=ADVANCED_FACE('',(#880),#499,.T.);
#6296=ADVANCED_FACE('',(#881),#5913,.T.);
#6297=ADVANCED_FACE('',(#882),#5914,.T.);
#6298=CLOSED_SHELL('',(#5915,#5916,#5917,#5918,#5919,#5920,#5921,#5922,
#5923,#5924,#5925,#5926,#5927,#5928,#5929,#5930,#5931,#5932,#5933,#5934,
#5935,#5936,#5937,#5938,#5939,#5940,#5941,#5942,#5943,#5944,#5945,#5946,
#5947,#5948,#5949,#5950,#5951,#5952,#5953,#5954,#5955,#5956,#5957,#5958,
#5959,#5960,#5961,#5962,#5963,#5964,#5965,#5966,#5967,#5968,#5969,#5970,
#5971,#5972,#5973,#5974,#5975,#5976,#5977,#5978,#5979,#5980,#5981,#5982,
#5983,#5984,#5985,#5986,#5987,#5988,#5989,#5990,#5991,#5992,#5993,#5994,
#5995,#5996,#5997,#5998,#5999,#6000,#6001,#6002,#6003,#6004,#6005,#6006,
#6007,#6008,#6009,#6010,#6011,#6012,#6013,#6014,#6015,#6016,#6017,#6018,
#6019,#6020,#6021,#6022,#6023,#6024,#6025,#6026,#6027,#6028,#6029,#6030,
#6031,#6032,#6033,#6034,#6035,#6036,#6037,#6038,#6039,#6040,#6041,#6042,
#6043,#6044,#6045,#6046,#6047,#6048,#6049,#6050,#6051,#6052,#6053,#6054,
#6055,#6056,#6057,#6058,#6059,#6060,#6061,#6062,#6063,#6064,#6065,#6066,
#6067,#6068,#6069,#6070,#6071,#6072,#6073,#6074,#6075,#6076,#6077,#6078,
#6079,#6080,#6081,#6082,#6083,#6084,#6085,#6086,#6087,#6088));
#6299=CLOSED_SHELL('',(#6089,#6090,#6091,#6092,#6093,#6094,#6095,#6096,
#6097,#6098,#6099,#6100,#6101,#6102,#6103,#6104,#6105,#6106,#6107,#6108,
#6109,#6110,#6111,#6112,#6113,#6114,#6115,#6116,#6117,#6118));
#6300=CLOSED_SHELL('',(#6119,#6120,#6121));
#6301=CLOSED_SHELL('',(#6122,#6123,#6124,#6125,#6126,#6127,#6128,#6129,
#6130,#6131,#6132,#6133,#6134,#6135,#6136,#6137,#6138,#6139,#6140,#6141,
#6142,#6143,#6144,#6145,#6146,#6147,#6148,#6149,#6150,#6151,#6152,#6153,
#6154,#6155,#6156));
#6302=CLOSED_SHELL('',(#6157,#6158,#6159,#6160));
#6303=CLOSED_SHELL('',(#6161,#6162,#6163,#6164,#6165,#6166,#6167,#6168,
#6169,#6170,#6171,#6172,#6173,#6174,#6175,#6176,#6177,#6178,#6179,#6180,
#6181,#6182,#6183,#6184,#6185,#6186,#6187,#6188,#6189,#6190,#6191,#6192,
#6193,#6194,#6195,#6196,#6197,#6198,#6199,#6200,#6201,#6202,#6203,#6204,
#6205,#6206,#6207,#6208,#6209,#6210,#6211,#6212,#6213,#6214,#6215,#6216,
#6217,#6218,#6219,#6220,#6221,#6222,#6223,#6224,#6225,#6226,#6227,#6228,
#6229));
#6304=CLOSED_SHELL('',(#6230,#6231,#6232,#6233,#6234,#6235,#6236,#6237,
#6238,#6239,#6240,#6241,#6242,#6243,#6244,#6245,#6246,#6247,#6248,#6249,
#6250,#6251,#6252,#6253));
#6305=CLOSED_SHELL('',(#6254,#6255,#6256,#6257,#6258,#6259,#6260,#6261,
#6262,#6263,#6264,#6265,#6266,#6267,#6268,#6269,#6270,#6271,#6272,#6273,
#6274,#6275,#6276,#6277,#6278,#6279,#6280,#6281,#6282,#6283,#6284,#6285,
#6286,#6287,#6288,#6289,#6290,#6291,#6292,#6293,#6294,#6295,#6296,#6297));
#6306=DERIVED_UNIT_ELEMENT(#6322,1.);
#6307=DERIVED_UNIT_ELEMENT(#40811,-3.);
#6308=DERIVED_UNIT_ELEMENT(#6322,1.);
#6309=DERIVED_UNIT_ELEMENT(#40811,-3.);
#6310=DERIVED_UNIT_ELEMENT(#6322,1.);
#6311=DERIVED_UNIT_ELEMENT(#40811,-3.);
#6312=DERIVED_UNIT_ELEMENT(#6322,1.);
#6313=DERIVED_UNIT_ELEMENT(#40811,-3.);
#6314=DERIVED_UNIT_ELEMENT(#6322,1.);
#6315=DERIVED_UNIT_ELEMENT(#40811,-3.);
#6316=DERIVED_UNIT_ELEMENT(#6322,1.);
#6317=DERIVED_UNIT_ELEMENT(#40811,-3.);
#6318=DERIVED_UNIT_ELEMENT(#6322,1.);
#6319=DERIVED_UNIT_ELEMENT(#40811,-3.);
#6320=DERIVED_UNIT_ELEMENT(#6322,1.);
#6321=DERIVED_UNIT_ELEMENT(#40811,-3.);
#6322=(
MASS_UNIT()
NAMED_UNIT(*)
SI_UNIT(.KILO.,.GRAM.)
);
#6323=DERIVED_UNIT((#6306,#6307));
#6324=DERIVED_UNIT((#6308,#6309));
#6325=DERIVED_UNIT((#6310,#6311));
#6326=DERIVED_UNIT((#6312,#6313));
#6327=DERIVED_UNIT((#6314,#6315));
#6328=DERIVED_UNIT((#6316,#6317));
#6329=DERIVED_UNIT((#6318,#6319));
#6330=DERIVED_UNIT((#6320,#6321));
#6331=MEASURE_REPRESENTATION_ITEM('density measure',
POSITIVE_RATIO_MEASURE(7850.),#6323);
#6332=MEASURE_REPRESENTATION_ITEM('density measure',
POSITIVE_RATIO_MEASURE(7850.),#6324);
#6333=MEASURE_REPRESENTATION_ITEM('density measure',
POSITIVE_RATIO_MEASURE(7850.),#6325);
#6334=MEASURE_REPRESENTATION_ITEM('density measure',
POSITIVE_RATIO_MEASURE(7850.),#6326);
#6335=MEASURE_REPRESENTATION_ITEM('density measure',
POSITIVE_RATIO_MEASURE(7850.),#6327);
#6336=MEASURE_REPRESENTATION_ITEM('density measure',
POSITIVE_RATIO_MEASURE(7850.),#6328);
#6337=MEASURE_REPRESENTATION_ITEM('density measure',
POSITIVE_RATIO_MEASURE(7850.),#6329);
#6338=MEASURE_REPRESENTATION_ITEM('density measure',
POSITIVE_RATIO_MEASURE(7850.),#6330);
#6339=PROPERTY_DEFINITION_REPRESENTATION(#6379,#6355);
#6340=PROPERTY_DEFINITION_REPRESENTATION(#6380,#6356);
#6341=PROPERTY_DEFINITION_REPRESENTATION(#6381,#6357);
#6342=PROPERTY_DEFINITION_REPRESENTATION(#6382,#6358);
#6343=PROPERTY_DEFINITION_REPRESENTATION(#6383,#6359);
#6344=PROPERTY_DEFINITION_REPRESENTATION(#6384,#6360);
#6345=PROPERTY_DEFINITION_REPRESENTATION(#6385,#6361);
#6346=PROPERTY_DEFINITION_REPRESENTATION(#6386,#6362);
#6347=PROPERTY_DEFINITION_REPRESENTATION(#6387,#6363);
#6348=PROPERTY_DEFINITION_REPRESENTATION(#6388,#6364);
#6349=PROPERTY_DEFINITION_REPRESENTATION(#6389,#6365);
#6350=PROPERTY_DEFINITION_REPRESENTATION(#6390,#6366);
#6351=PROPERTY_DEFINITION_REPRESENTATION(#6391,#6367);
#6352=PROPERTY_DEFINITION_REPRESENTATION(#6392,#6368);
#6353=PROPERTY_DEFINITION_REPRESENTATION(#6393,#6369);
#6354=PROPERTY_DEFINITION_REPRESENTATION(#6394,#6370);
#6355=REPRESENTATION('material name',(#6371),#40801);
#6356=REPRESENTATION('density',(#6331),#40801);
#6357=REPRESENTATION('material name',(#6372),#40802);
#6358=REPRESENTATION('density',(#6332),#40802);
#6359=REPRESENTATION('material name',(#6373),#40803);
#6360=REPRESENTATION('density',(#6333),#40803);
#6361=REPRESENTATION('material name',(#6374),#40804);
#6362=REPRESENTATION('density',(#6334),#40804);
#6363=REPRESENTATION('material name',(#6375),#40805);
#6364=REPRESENTATION('density',(#6335),#40805);
#6365=REPRESENTATION('material name',(#6376),#40806);
#6366=REPRESENTATION('density',(#6336),#40806);
#6367=REPRESENTATION('material name',(#6377),#40807);
#6368=REPRESENTATION('density',(#6337),#40807);
#6369=REPRESENTATION('material name',(#6378),#40808);
#6370=REPRESENTATION('density',(#6338),#40808);
#6371=DESCRIPTIVE_REPRESENTATION_ITEM('Steel','Steel');
#6372=DESCRIPTIVE_REPRESENTATION_ITEM('Steel','Steel');
#6373=DESCRIPTIVE_REPRESENTATION_ITEM('Steel','Steel');
#6374=DESCRIPTIVE_REPRESENTATION_ITEM('Steel','Steel');
#6375=DESCRIPTIVE_REPRESENTATION_ITEM('Steel','Steel');
#6376=DESCRIPTIVE_REPRESENTATION_ITEM('Steel','Steel');
#6377=DESCRIPTIVE_REPRESENTATION_ITEM('Steel','Steel');
#6378=DESCRIPTIVE_REPRESENTATION_ITEM('Steel','Steel');
#6379=PROPERTY_DEFINITION('material property','material name',#40867);
#6380=PROPERTY_DEFINITION('material property','density of part',#40867);
#6381=PROPERTY_DEFINITION('material property','material name',#40868);
#6382=PROPERTY_DEFINITION('material property','density of part',#40868);
#6383=PROPERTY_DEFINITION('material property','material name',#40869);
#6384=PROPERTY_DEFINITION('material property','density of part',#40869);
#6385=PROPERTY_DEFINITION('material property','material name',#40870);
#6386=PROPERTY_DEFINITION('material property','density of part',#40870);
#6387=PROPERTY_DEFINITION('material property','material name',#40871);
#6388=PROPERTY_DEFINITION('material property','density of part',#40871);
#6389=PROPERTY_DEFINITION('material property','material name',#40872);
#6390=PROPERTY_DEFINITION('material property','density of part',#40872);
#6391=PROPERTY_DEFINITION('material property','material name',#40873);
#6392=PROPERTY_DEFINITION('material property','density of part',#40873);
#6393=PROPERTY_DEFINITION('material property','material name',#40874);
#6394=PROPERTY_DEFINITION('material property','density of part',#40874);
#6395=AXIS2_PLACEMENT_3D('',#9083,#7185,#7186);
#6396=AXIS2_PLACEMENT_3D('',#9084,#7187,#7188);
#6397=AXIS2_PLACEMENT_3D('',#9085,#7189,#7190);
#6398=AXIS2_PLACEMENT_3D('',#9127,#7192,#7193);
#6399=AXIS2_PLACEMENT_3D('',#9139,#7195,#7196);
#6400=AXIS2_PLACEMENT_3D('',#9176,#7197,#7198);
#6401=AXIS2_PLACEMENT_3D('',#9254,#7200,#7201);
#6402=AXIS2_PLACEMENT_3D('',#9330,#7203,#7204);
#6403=AXIS2_PLACEMENT_3D('',#9408,#7206,#7207);
#6404=AXIS2_PLACEMENT_3D('',#9484,#7209,#7210);
#6405=AXIS2_PLACEMENT_3D('',#9560,#7212,#7213);
#6406=AXIS2_PLACEMENT_3D('',#9636,#7215,#7216);
#6407=AXIS2_PLACEMENT_3D('',#9714,#7218,#7219);
#6408=AXIS2_PLACEMENT_3D('',#9790,#7221,#7222);
#6409=AXIS2_PLACEMENT_3D('',#9868,#7224,#7225);
#6410=AXIS2_PLACEMENT_3D('',#9944,#7227,#7228);
#6411=AXIS2_PLACEMENT_3D('',#10020,#7230,#7231);
#6412=AXIS2_PLACEMENT_3D('',#10096,#7233,#7234);
#6413=AXIS2_PLACEMENT_3D('',#10174,#7236,#7237);
#6414=AXIS2_PLACEMENT_3D('',#10250,#7239,#7240);
#6415=AXIS2_PLACEMENT_3D('',#10328,#7242,#7243);
#6416=AXIS2_PLACEMENT_3D('',#10404,#7245,#7246);
#6417=AXIS2_PLACEMENT_3D('',#10480,#7248,#7249);
#6418=AXIS2_PLACEMENT_3D('',#10556,#7251,#7252);
#6419=AXIS2_PLACEMENT_3D('',#10634,#7254,#7255);
#6420=AXIS2_PLACEMENT_3D('',#10710,#7257,#7258);
#6421=AXIS2_PLACEMENT_3D('',#10728,#7260,#7261);
#6422=AXIS2_PLACEMENT_3D('',#10747,#7262,#7263);
#6423=AXIS2_PLACEMENT_3D('',#10750,#7264,#7265);
#6424=AXIS2_PLACEMENT_3D('',#10751,#7266,#7267);
#6425=AXIS2_PLACEMENT_3D('',#10753,#7268,#7269);
#6426=AXIS2_PLACEMENT_3D('',#10754,#7270,#7271);
#6427=AXIS2_PLACEMENT_3D('',#10755,#7272,#7273);
#6428=AXIS2_PLACEMENT_3D('',#10757,#7274,#7275);
#6429=AXIS2_PLACEMENT_3D('',#10759,#7276,#7277);
#6430=AXIS2_PLACEMENT_3D('',#10761,#7278,#7279);
#6431=AXIS2_PLACEMENT_3D('',#10762,#7280,#7281);
#6432=AXIS2_PLACEMENT_3D('',#10763,#7282,#7283);
#6433=AXIS2_PLACEMENT_3D('',#10766,#7284,#7285);
#6434=AXIS2_PLACEMENT_3D('',#10768,#7286,#7287);
#6435=AXIS2_PLACEMENT_3D('',#10770,#7288,#7289);
#6436=AXIS2_PLACEMENT_3D('',#10771,#7290,#7291);
#6437=AXIS2_PLACEMENT_3D('',#10772,#7292,#7293);
#6438=AXIS2_PLACEMENT_3D('',#10775,#7294,#7295);
#6439=AXIS2_PLACEMENT_3D('',#10779,#7297,#7298);
#6440=AXIS2_PLACEMENT_3D('',#10837,#7300,#7301);
#6441=AXIS2_PLACEMENT_3D('',#10840,#7303,#7304);
#6442=AXIS2_PLACEMENT_3D('',#10842,#7306,#7307);
#6443=AXIS2_PLACEMENT_3D('',#10845,#7308,#7309);
#6444=AXIS2_PLACEMENT_3D('',#10849,#7311,#7312);
#6445=AXIS2_PLACEMENT_3D('',#10851,#7314,#7315);
#6446=AXIS2_PLACEMENT_3D('',#10910,#7316,#7317);
#6447=AXIS2_PLACEMENT_3D('',#10913,#7319,#7320);
#6448=AXIS2_PLACEMENT_3D('',#10915,#7322,#7323);
#6449=AXIS2_PLACEMENT_3D('',#10918,#7325,#7326);
#6450=AXIS2_PLACEMENT_3D('',#10919,#7327,#7328);
#6451=AXIS2_PLACEMENT_3D('',#11022,#7329,#7330);
#6452=AXIS2_PLACEMENT_3D('',#11124,#7331,#7332);
#6453=AXIS2_PLACEMENT_3D('',#11132,#7333,#7334);
#6454=AXIS2_PLACEMENT_3D('',#11135,#7335,#7336);
#6455=AXIS2_PLACEMENT_3D('',#11178,#7337,#7338);
#6456=AXIS2_PLACEMENT_3D('',#11180,#7339,#7340);
#6457=AXIS2_PLACEMENT_3D('',#11224,#7341,#7342);
#6458=AXIS2_PLACEMENT_3D('',#11227,#7343,#7344);
#6459=AXIS2_PLACEMENT_3D('',#11270,#7345,#7346);
#6460=AXIS2_PLACEMENT_3D('',#11314,#7347,#7348);
#6461=AXIS2_PLACEMENT_3D('',#11389,#7349,#7350);
#6462=AXIS2_PLACEMENT_3D('',#11391,#7351,#7352);
#6463=AXIS2_PLACEMENT_3D('',#11394,#7354,#7355);
#6464=AXIS2_PLACEMENT_3D('',#11395,#7356,#7357);
#6465=AXIS2_PLACEMENT_3D('',#11397,#7358,#7359);
#6466=AXIS2_PLACEMENT_3D('',#11400,#7361,#7362);
#6467=AXIS2_PLACEMENT_3D('',#11401,#7363,#7364);
#6468=AXIS2_PLACEMENT_3D('',#11403,#7365,#7366);
#6469=AXIS2_PLACEMENT_3D('',#11406,#7368,#7369);
#6470=AXIS2_PLACEMENT_3D('',#11407,#7370,#7371);
#6471=AXIS2_PLACEMENT_3D('',#11412,#7374,#7375);
#6472=AXIS2_PLACEMENT_3D('',#11415,#7377,#7378);
#6473=AXIS2_PLACEMENT_3D('',#11420,#7381,#7382);
#6474=AXIS2_PLACEMENT_3D('',#11426,#7386,#7387);
#6475=AXIS2_PLACEMENT_3D('',#11427,#7388,#7389);
#6476=AXIS2_PLACEMENT_3D('',#11430,#7390,#7391);
#6477=AXIS2_PLACEMENT_3D('',#11432,#7392,#7393);
#6478=AXIS2_PLACEMENT_3D('',#11434,#7394,#7395);
#6479=AXIS2_PLACEMENT_3D('',#11436,#7396,#7397);
#6480=AXIS2_PLACEMENT_3D('',#11438,#7398,#7399);
#6481=AXIS2_PLACEMENT_3D('',#11439,#7400,#7401);
#6482=AXIS2_PLACEMENT_3D('',#11440,#7402,#7403);
#6483=AXIS2_PLACEMENT_3D('',#11454,#7407,#7408);
#6484=AXIS2_PLACEMENT_3D('',#11468,#7412,#7413);
#6485=AXIS2_PLACEMENT_3D('',#11482,#7417,#7418);
#6486=AXIS2_PLACEMENT_3D('',#11496,#7422,#7423);
#6487=AXIS2_PLACEMENT_3D('',#11510,#7427,#7428);
#6488=AXIS2_PLACEMENT_3D('',#11524,#7432,#7433);
#6489=AXIS2_PLACEMENT_3D('',#11556,#7434,#7435);
#6490=AXIS2_PLACEMENT_3D('',#11557,#7436,#7437);
#6491=AXIS2_PLACEMENT_3D('',#11606,#7438,#7439);
#6492=AXIS2_PLACEMENT_3D('',#11615,#7443,#7444);
#6493=AXIS2_PLACEMENT_3D('',#11619,#7447,#7448);
#6494=AXIS2_PLACEMENT_3D('',#11631,#7454,#7455);
#6495=AXIS2_PLACEMENT_3D('',#11632,#7456,#7457);
#6496=AXIS2_PLACEMENT_3D('',#11639,#7460,#7461);
#6497=AXIS2_PLACEMENT_3D('',#11641,#7463,#7464);
#6498=AXIS2_PLACEMENT_3D('',#11645,#7466,#7467);
#6499=AXIS2_PLACEMENT_3D('',#11646,#7468,#7469);
#6500=AXIS2_PLACEMENT_3D('',#11647,#7470,#7471);
#6501=AXIS2_PLACEMENT_3D('',#11653,#7475,#7476);
#6502=AXIS2_PLACEMENT_3D('',#11657,#7478,#7479);
#6503=AXIS2_PLACEMENT_3D('',#11658,#7480,#7481);
#6504=AXIS2_PLACEMENT_3D('',#11659,#7482,#7483);
#6505=AXIS2_PLACEMENT_3D('',#11665,#7487,#7488);
#6506=AXIS2_PLACEMENT_3D('',#11667,#7489,#7490);
#6507=AXIS2_PLACEMENT_3D('',#11671,#7492,#7493);
#6508=AXIS2_PLACEMENT_3D('',#11675,#7495,#7496);
#6509=AXIS2_PLACEMENT_3D('',#11678,#7498,#7499);
#6510=AXIS2_PLACEMENT_3D('',#11679,#7500,#7501);
#6511=AXIS2_PLACEMENT_3D('',#11688,#7505,#7506);
#6512=AXIS2_PLACEMENT_3D('',#11692,#7509,#7510);
#6513=AXIS2_PLACEMENT_3D('',#11699,#7513,#7514);
#6514=AXIS2_PLACEMENT_3D('',#11701,#7516,#7517);
#6515=AXIS2_PLACEMENT_3D('',#11702,#7518,#7519);
#6516=AXIS2_PLACEMENT_3D('',#11705,#7521,#7522);
#6517=AXIS2_PLACEMENT_3D('',#11706,#7523,#7524);
#6518=AXIS2_PLACEMENT_3D('',#11710,#7527,#7528);
#6519=AXIS2_PLACEMENT_3D('',#11711,#7529,#7530);
#6520=AXIS2_PLACEMENT_3D('',#11714,#7532,#7533);
#6521=AXIS2_PLACEMENT_3D('',#11715,#7534,#7535);
#6522=AXIS2_PLACEMENT_3D('',#11719,#7538,#7539);
#6523=AXIS2_PLACEMENT_3D('',#11721,#7540,#7541);
#6524=AXIS2_PLACEMENT_3D('',#11725,#7543,#7544);
#6525=AXIS2_PLACEMENT_3D('',#11729,#7547,#7548);
#6526=AXIS2_PLACEMENT_3D('',#11730,#7549,#7550);
#6527=AXIS2_PLACEMENT_3D('',#11737,#7554,#7555);
#6528=AXIS2_PLACEMENT_3D('',#11738,#7556,#7557);
#6529=AXIS2_PLACEMENT_3D('',#11744,#7560,#7561);
#6530=AXIS2_PLACEMENT_3D('',#11746,#7563,#7564);
#6531=AXIS2_PLACEMENT_3D('',#11752,#7568,#7569);
#6532=AXIS2_PLACEMENT_3D('',#11754,#7570,#7571);
#6533=AXIS2_PLACEMENT_3D('',#11756,#7573,#7574);
#6534=AXIS2_PLACEMENT_3D('',#11757,#7575,#7576);
#6535=AXIS2_PLACEMENT_3D('',#11761,#7579,#7580);
#6536=AXIS2_PLACEMENT_3D('',#11763,#7581,#7582);
#6537=AXIS2_PLACEMENT_3D('',#11765,#7584,#7585);
#6538=AXIS2_PLACEMENT_3D('',#11766,#7586,#7587);
#6539=AXIS2_PLACEMENT_3D('',#11770,#7590,#7591);
#6540=AXIS2_PLACEMENT_3D('',#11773,#7592,#7593);
#6541=AXIS2_PLACEMENT_3D('',#11775,#7594,#7595);
#6542=AXIS2_PLACEMENT_3D('',#11779,#7597,#7598);
#6543=AXIS2_PLACEMENT_3D('',#11783,#7600,#7601);
#6544=AXIS2_PLACEMENT_3D('',#11786,#7603,#7604);
#6545=AXIS2_PLACEMENT_3D('',#11787,#7605,#7606);
#6546=AXIS2_PLACEMENT_3D('',#11799,#7612,#7613);
#6547=AXIS2_PLACEMENT_3D('',#11800,#7614,#7615);
#6548=AXIS2_PLACEMENT_3D('',#11842,#7616,#7617);
#6549=AXIS2_PLACEMENT_3D('',#11922,#7618,#7619);
#6550=AXIS2_PLACEMENT_3D('',#11924,#7620,#7621);
#6551=AXIS2_PLACEMENT_3D('',#12041,#7622,#7623);
#6552=AXIS2_PLACEMENT_3D('',#12083,#7624,#7625);
#6553=AXIS2_PLACEMENT_3D('',#12163,#7626,#7627);
#6554=AXIS2_PLACEMENT_3D('',#12165,#7628,#7629);
#6555=AXIS2_PLACEMENT_3D('',#12282,#7630,#7631);
#6556=AXIS2_PLACEMENT_3D('',#12324,#7632,#7633);
#6557=AXIS2_PLACEMENT_3D('',#12404,#7634,#7635);
#6558=AXIS2_PLACEMENT_3D('',#12406,#7636,#7637);
#6559=AXIS2_PLACEMENT_3D('',#12523,#7638,#7639);
#6560=AXIS2_PLACEMENT_3D('',#12607,#7640,#7641);
#6561=AXIS2_PLACEMENT_3D('',#12806,#7642,#7643);
#6562=AXIS2_PLACEMENT_3D('',#13005,#7644,#7645);
#6563=AXIS2_PLACEMENT_3D('',#25550,#7646,#7647);
#6564=AXIS2_PLACEMENT_3D('',#25555,#7649,#7650);
#6565=AXIS2_PLACEMENT_3D('',#25559,#7652,#7653);
#6566=AXIS2_PLACEMENT_3D('',#25563,#7655,#7656);
#6567=AXIS2_PLACEMENT_3D('',#25567,#7658,#7659);
#6568=AXIS2_PLACEMENT_3D('',#25571,#7661,#7662);
#6569=AXIS2_PLACEMENT_3D('',#25574,#7664,#7665);
#6570=AXIS2_PLACEMENT_3D('',#25575,#7666,#7667);
#6571=AXIS2_PLACEMENT_3D('',#25586,#7668,#7669);
#6572=AXIS2_PLACEMENT_3D('',#25597,#7670,#7671);
#6573=AXIS2_PLACEMENT_3D('',#25608,#7672,#7673);
#6574=AXIS2_PLACEMENT_3D('',#25619,#7674,#7675);
#6575=AXIS2_PLACEMENT_3D('',#25630,#7676,#7677);
#6576=AXIS2_PLACEMENT_3D('',#25641,#7678,#7679);
#6577=AXIS2_PLACEMENT_3D('',#25642,#7680,#7681);
#6578=AXIS2_PLACEMENT_3D('',#25643,#7682,#7683);
#6579=AXIS2_PLACEMENT_3D('',#25644,#7684,#7685);
#6580=AXIS2_PLACEMENT_3D('',#25645,#7686,#7687);
#6581=AXIS2_PLACEMENT_3D('',#25646,#7688,#7689);
#6582=AXIS2_PLACEMENT_3D('',#25647,#7690,#7691);
#6583=AXIS2_PLACEMENT_3D('',#25648,#7692,#7693);
#6584=AXIS2_PLACEMENT_3D('',#25649,#7694,#7695);
#6585=AXIS2_PLACEMENT_3D('',#25650,#7696,#7697);
#6586=AXIS2_PLACEMENT_3D('',#25651,#7698,#7699);
#6587=AXIS2_PLACEMENT_3D('',#25652,#7700,#7701);
#6588=AXIS2_PLACEMENT_3D('',#25653,#7702,#7703);
#6589=AXIS2_PLACEMENT_3D('',#25654,#7704,#7705);
#6590=AXIS2_PLACEMENT_3D('',#25655,#7706,#7707);
#6591=AXIS2_PLACEMENT_3D('',#25656,#7708,#7709);
#6592=AXIS2_PLACEMENT_3D('',#25657,#7710,#7711);
#6593=AXIS2_PLACEMENT_3D('',#25658,#7712,#7713);
#6594=AXIS2_PLACEMENT_3D('',#25659,#7714,#7715);
#6595=AXIS2_PLACEMENT_3D('',#25660,#7716,#7717);
#6596=AXIS2_PLACEMENT_3D('',#25661,#7718,#7719);
#6597=AXIS2_PLACEMENT_3D('',#25662,#7720,#7721);
#6598=AXIS2_PLACEMENT_3D('',#25663,#7722,#7723);
#6599=AXIS2_PLACEMENT_3D('',#25664,#7724,#7725);
#6600=AXIS2_PLACEMENT_3D('',#25665,#7726,#7727);
#6601=AXIS2_PLACEMENT_3D('',#25666,#7728,#7729);
#6602=AXIS2_PLACEMENT_3D('',#25667,#7730,#7731);
#6603=AXIS2_PLACEMENT_3D('',#25668,#7732,#7733);
#6604=AXIS2_PLACEMENT_3D('',#25669,#7734,#7735);
#6605=AXIS2_PLACEMENT_3D('',#25670,#7736,#7737);
#6606=AXIS2_PLACEMENT_3D('',#25671,#7738,#7739);
#6607=AXIS2_PLACEMENT_3D('',#25672,#7740,#7741);
#6608=AXIS2_PLACEMENT_3D('',#25673,#7742,#7743);
#6609=AXIS2_PLACEMENT_3D('',#25674,#7744,#7745);
#6610=AXIS2_PLACEMENT_3D('',#25675,#7746,#7747);
#6611=AXIS2_PLACEMENT_3D('',#25676,#7748,#7749);
#6612=AXIS2_PLACEMENT_3D('',#25677,#7750,#7751);
#6613=AXIS2_PLACEMENT_3D('',#25678,#7752,#7753);
#6614=AXIS2_PLACEMENT_3D('',#25679,#7754,#7755);
#6615=AXIS2_PLACEMENT_3D('',#25680,#7756,#7757);
#6616=AXIS2_PLACEMENT_3D('',#25681,#7758,#7759);
#6617=AXIS2_PLACEMENT_3D('',#25682,#7760,#7761);
#6618=AXIS2_PLACEMENT_3D('',#25859,#7762,#7763);
#6619=AXIS2_PLACEMENT_3D('',#25860,#7764,#7765);
#6620=AXIS2_PLACEMENT_3D('',#25873,#7766,#7767);
#6621=AXIS2_PLACEMENT_3D('',#25916,#7768,#7769);
#6622=AXIS2_PLACEMENT_3D('',#25917,#7770,#7771);
#6623=AXIS2_PLACEMENT_3D('',#25918,#7772,#7773);
#6624=AXIS2_PLACEMENT_3D('',#25919,#7774,#7775);
#6625=AXIS2_PLACEMENT_3D('',#25920,#7776,#7777);
#6626=AXIS2_PLACEMENT_3D('',#25921,#7778,#7779);
#6627=AXIS2_PLACEMENT_3D('',#26098,#7780,#7781);
#6628=AXIS2_PLACEMENT_3D('',#26099,#7782,#7783);
#6629=AXIS2_PLACEMENT_3D('',#26112,#7784,#7785);
#6630=AXIS2_PLACEMENT_3D('',#26161,#7786,#7787);
#6631=AXIS2_PLACEMENT_3D('',#26162,#7788,#7789);
#6632=AXIS2_PLACEMENT_3D('',#26163,#7790,#7791);
#6633=AXIS2_PLACEMENT_3D('',#26164,#7792,#7793);
#6634=AXIS2_PLACEMENT_3D('',#26165,#7794,#7795);
#6635=AXIS2_PLACEMENT_3D('',#26166,#7796,#7797);
#6636=AXIS2_PLACEMENT_3D('',#26343,#7798,#7799);
#6637=AXIS2_PLACEMENT_3D('',#26344,#7800,#7801);
#6638=AXIS2_PLACEMENT_3D('',#26357,#7802,#7803);
#6639=AXIS2_PLACEMENT_3D('',#26448,#7804,#7805);
#6640=AXIS2_PLACEMENT_3D('',#26461,#7806,#7807);
#6641=AXIS2_PLACEMENT_3D('',#26462,#7808,#7809);
#6642=AXIS2_PLACEMENT_3D('',#26569,#7810,#7811);
#6643=AXIS2_PLACEMENT_3D('',#26570,#7812,#7813);
#6644=AXIS2_PLACEMENT_3D('',#26677,#7814,#7815);
#6645=AXIS2_PLACEMENT_3D('',#26678,#7816,#7817);
#6646=AXIS2_PLACEMENT_3D('',#26691,#7818,#7819);
#6647=AXIS2_PLACEMENT_3D('',#26782,#7820,#7821);
#6648=AXIS2_PLACEMENT_3D('',#26795,#7822,#7823);
#6649=AXIS2_PLACEMENT_3D('',#26796,#7824,#7825);
#6650=AXIS2_PLACEMENT_3D('',#26973,#7826,#7827);
#6651=AXIS2_PLACEMENT_3D('',#26974,#7828,#7829);
#6652=AXIS2_PLACEMENT_3D('',#26975,#7830,#7831);
#6653=AXIS2_PLACEMENT_3D('',#26976,#7832,#7833);
#6654=AXIS2_PLACEMENT_3D('',#26977,#7834,#7835);
#6655=AXIS2_PLACEMENT_3D('',#26978,#7836,#7837);
#6656=AXIS2_PLACEMENT_3D('',#27003,#7838,#7839);
#6657=AXIS2_PLACEMENT_3D('',#27004,#7840,#7841);
#6658=AXIS2_PLACEMENT_3D('',#27005,#7842,#7843);
#6659=AXIS2_PLACEMENT_3D('',#27006,#7844,#7845);
#6660=AXIS2_PLACEMENT_3D('',#27007,#7846,#7847);
#6661=AXIS2_PLACEMENT_3D('',#27008,#7848,#7849);
#6662=AXIS2_PLACEMENT_3D('',#27009,#7850,#7851);
#6663=AXIS2_PLACEMENT_3D('',#27010,#7852,#7853);
#6664=AXIS2_PLACEMENT_3D('',#27011,#7854,#7855);
#6665=AXIS2_PLACEMENT_3D('',#27012,#7856,#7857);
#6666=AXIS2_PLACEMENT_3D('',#27013,#7858,#7859);
#6667=AXIS2_PLACEMENT_3D('',#27014,#7860,#7861);
#6668=AXIS2_PLACEMENT_3D('',#27015,#7862,#7863);
#6669=AXIS2_PLACEMENT_3D('',#27016,#7864,#7865);
#6670=AXIS2_PLACEMENT_3D('',#27017,#7866,#7867);
#6671=AXIS2_PLACEMENT_3D('',#27066,#7868,#7869);
#6672=AXIS2_PLACEMENT_3D('',#27067,#7870,#7871);
#6673=AXIS2_PLACEMENT_3D('',#27068,#7872,#7873);
#6674=AXIS2_PLACEMENT_3D('',#27069,#7874,#7875);
#6675=AXIS2_PLACEMENT_3D('',#27070,#7876,#7877);
#6676=AXIS2_PLACEMENT_3D('',#27071,#7878,#7879);
#6677=AXIS2_PLACEMENT_3D('',#27072,#7880,#7881);
#6678=AXIS2_PLACEMENT_3D('',#27073,#7882,#7883);
#6679=AXIS2_PLACEMENT_3D('',#27074,#7884,#7885);
#6680=AXIS2_PLACEMENT_3D('',#27075,#7886,#7887);
#6681=AXIS2_PLACEMENT_3D('',#27076,#7888,#7889);
#6682=AXIS2_PLACEMENT_3D('',#27077,#7890,#7891);
#6683=AXIS2_PLACEMENT_3D('',#27078,#7892,#7893);
#6684=AXIS2_PLACEMENT_3D('',#27079,#7894,#7895);
#6685=AXIS2_PLACEMENT_3D('',#27080,#7896,#7897);
#6686=AXIS2_PLACEMENT_3D('',#27129,#7898,#7899);
#6687=AXIS2_PLACEMENT_3D('',#27130,#7900,#7901);
#6688=AXIS2_PLACEMENT_3D('',#27131,#7902,#7903);
#6689=AXIS2_PLACEMENT_3D('',#27132,#7904,#7905);
#6690=AXIS2_PLACEMENT_3D('',#27133,#7906,#7907);
#6691=AXIS2_PLACEMENT_3D('',#27134,#7908,#7909);
#6692=AXIS2_PLACEMENT_3D('',#27135,#7910,#7911);
#6693=AXIS2_PLACEMENT_3D('',#27136,#7912,#7913);
#6694=AXIS2_PLACEMENT_3D('',#27137,#7914,#7915);
#6695=AXIS2_PLACEMENT_3D('',#27138,#7916,#7917);
#6696=AXIS2_PLACEMENT_3D('',#27139,#7918,#7919);
#6697=AXIS2_PLACEMENT_3D('',#27140,#7920,#7921);
#6698=AXIS2_PLACEMENT_3D('',#27165,#7922,#7923);
#6699=AXIS2_PLACEMENT_3D('',#27467,#7924,#7925);
#6700=AXIS2_PLACEMENT_3D('',#27573,#7926,#7927);
#6701=AXIS2_PLACEMENT_3D('',#27792,#7928,#7929);
#6702=AXIS2_PLACEMENT_3D('',#27988,#7930,#7931);
#6703=AXIS2_PLACEMENT_3D('',#27990,#7932,#7933);
#6704=AXIS2_PLACEMENT_3D('',#28076,#7934,#7935);
#6705=AXIS2_PLACEMENT_3D('',#28079,#7936,#7937);
#6706=AXIS2_PLACEMENT_3D('',#28087,#7938,#7939);
#6707=AXIS2_PLACEMENT_3D('',#28167,#7941,#7942);
#6708=AXIS2_PLACEMENT_3D('',#28344,#7943,#7944);
#6709=AXIS2_PLACEMENT_3D('',#28347,#7945,#7946);
#6710=AXIS2_PLACEMENT_3D('',#28348,#7947,#7948);
#6711=AXIS2_PLACEMENT_3D('',#28351,#7950,#7951);
#6712=AXIS2_PLACEMENT_3D('',#28352,#7952,#7953);
#6713=AXIS2_PLACEMENT_3D('',#28355,#7955,#7956);
#6714=AXIS2_PLACEMENT_3D('',#28358,#7957,#7958);
#6715=AXIS2_PLACEMENT_3D('',#28359,#7959,#7960);
#6716=AXIS2_PLACEMENT_3D('',#28362,#7962,#7963);
#6717=AXIS2_PLACEMENT_3D('',#28363,#7964,#7965);
#6718=AXIS2_PLACEMENT_3D('',#28365,#7966,#7967);
#6719=AXIS2_PLACEMENT_3D('',#28368,#7969,#7970);
#6720=AXIS2_PLACEMENT_3D('',#28369,#7971,#7972);
#6721=AXIS2_PLACEMENT_3D('',#28462,#7975,#7976);
#6722=AXIS2_PLACEMENT_3D('',#28543,#7977,#7978);
#6723=AXIS2_PLACEMENT_3D('',#28725,#7979,#7980);
#6724=AXIS2_PLACEMENT_3D('',#28726,#7981,#7982);
#6725=AXIS2_PLACEMENT_3D('',#39438,#7983,#7984);
#6726=AXIS2_PLACEMENT_3D('',#39439,#7985,#7986);
#6727=AXIS2_PLACEMENT_3D('',#39456,#7991,#7992);
#6728=AXIS2_PLACEMENT_3D('',#39470,#7996,#7997);
#6729=AXIS2_PLACEMENT_3D('',#39484,#8001,#8002);
#6730=AXIS2_PLACEMENT_3D('',#39498,#8006,#8007);
#6731=AXIS2_PLACEMENT_3D('',#39507,#8011,#8012);
#6732=AXIS2_PLACEMENT_3D('',#39514,#8015,#8016);
#6733=AXIS2_PLACEMENT_3D('',#39515,#8017,#8018);
#6734=AXIS2_PLACEMENT_3D('',#39516,#8019,#8020);
#6735=AXIS2_PLACEMENT_3D('',#39517,#8021,#8022);
#6736=AXIS2_PLACEMENT_3D('',#39518,#8023,#8024);
#6737=AXIS2_PLACEMENT_3D('',#39519,#8025,#8026);
#6738=AXIS2_PLACEMENT_3D('',#39520,#8027,#8028);
#6739=AXIS2_PLACEMENT_3D('',#39521,#8029,#8030);
#6740=AXIS2_PLACEMENT_3D('',#39522,#8031,#8032);
#6741=AXIS2_PLACEMENT_3D('',#39523,#8033,#8034);
#6742=AXIS2_PLACEMENT_3D('',#39524,#8035,#8036);
#6743=AXIS2_PLACEMENT_3D('',#39525,#8037,#8038);
#6744=AXIS2_PLACEMENT_3D('',#39784,#8039,#8040);
#6745=AXIS2_PLACEMENT_3D('',#39785,#8041,#8042);
#6746=AXIS2_PLACEMENT_3D('',#39788,#8043,#8044);
#6747=AXIS2_PLACEMENT_3D('',#39790,#8045,#8046);
#6748=AXIS2_PLACEMENT_3D('',#39791,#8047,#8048);
#6749=AXIS2_PLACEMENT_3D('',#39792,#8049,#8050);
#6750=AXIS2_PLACEMENT_3D('',#39795,#8051,#8052);
#6751=AXIS2_PLACEMENT_3D('',#39797,#8053,#8054);
#6752=AXIS2_PLACEMENT_3D('',#39798,#8055,#8056);
#6753=AXIS2_PLACEMENT_3D('',#39799,#8057,#8058);
#6754=AXIS2_PLACEMENT_3D('',#39801,#8060,#8061);
#6755=AXIS2_PLACEMENT_3D('',#39802,#8062,#8063);
#6756=AXIS2_PLACEMENT_3D('',#39804,#8064,#8065);
#6757=AXIS2_PLACEMENT_3D('',#39808,#8067,#8068);
#6758=AXIS2_PLACEMENT_3D('',#39809,#8069,#8070);
#6759=AXIS2_PLACEMENT_3D('',#39810,#8071,#8072);
#6760=AXIS2_PLACEMENT_3D('',#39813,#8073,#8074);
#6761=AXIS2_PLACEMENT_3D('',#39814,#8075,#8076);
#6762=AXIS2_PLACEMENT_3D('',#39816,#8078,#8079);
#6763=AXIS2_PLACEMENT_3D('',#39818,#8080,#8081);
#6764=AXIS2_PLACEMENT_3D('',#39822,#8083,#8084);
#6765=AXIS2_PLACEMENT_3D('',#39823,#8085,#8086);
#6766=AXIS2_PLACEMENT_3D('',#39824,#8087,#8088);
#6767=AXIS2_PLACEMENT_3D('',#39827,#8089,#8090);
#6768=AXIS2_PLACEMENT_3D('',#39828,#8091,#8092);
#6769=AXIS2_PLACEMENT_3D('',#39830,#8094,#8095);
#6770=AXIS2_PLACEMENT_3D('',#39832,#8096,#8097);
#6771=AXIS2_PLACEMENT_3D('',#39836,#8099,#8100);
#6772=AXIS2_PLACEMENT_3D('',#39837,#8101,#8102);
#6773=AXIS2_PLACEMENT_3D('',#39838,#8103,#8104);
#6774=AXIS2_PLACEMENT_3D('',#39841,#8105,#8106);
#6775=AXIS2_PLACEMENT_3D('',#39842,#8107,#8108);
#6776=AXIS2_PLACEMENT_3D('',#39844,#8110,#8111);
#6777=AXIS2_PLACEMENT_3D('',#39846,#8112,#8113);
#6778=AXIS2_PLACEMENT_3D('',#39850,#8115,#8116);
#6779=AXIS2_PLACEMENT_3D('',#39851,#8117,#8118);
#6780=AXIS2_PLACEMENT_3D('',#39852,#8119,#8120);
#6781=AXIS2_PLACEMENT_3D('',#39855,#8121,#8122);
#6782=AXIS2_PLACEMENT_3D('',#39857,#8124,#8125);
#6783=AXIS2_PLACEMENT_3D('',#39858,#8126,#8127);
#6784=AXIS2_PLACEMENT_3D('',#39860,#8128,#8129);
#6785=AXIS2_PLACEMENT_3D('',#39864,#8131,#8132);
#6786=AXIS2_PLACEMENT_3D('',#39865,#8133,#8134);
#6787=AXIS2_PLACEMENT_3D('',#39866,#8135,#8136);
#6788=AXIS2_PLACEMENT_3D('',#39869,#8137,#8138);
#6789=AXIS2_PLACEMENT_3D('',#39871,#8140,#8141);
#6790=AXIS2_PLACEMENT_3D('',#39872,#8142,#8143);
#6791=AXIS2_PLACEMENT_3D('',#39875,#8145,#8146);
#6792=AXIS2_PLACEMENT_3D('',#39876,#8147,#8148);
#6793=AXIS2_PLACEMENT_3D('',#39878,#8150,#8151);
#6794=AXIS2_PLACEMENT_3D('',#39880,#8153,#8154);
#6795=AXIS2_PLACEMENT_3D('',#39882,#8156,#8157);
#6796=AXIS2_PLACEMENT_3D('',#39884,#8159,#8160);
#6797=AXIS2_PLACEMENT_3D('',#39905,#8163,#8164);
#6798=AXIS2_PLACEMENT_3D('',#39923,#8166,#8167);
#6799=AXIS2_PLACEMENT_3D('',#39941,#8169,#8170);
#6800=AXIS2_PLACEMENT_3D('',#39959,#8172,#8173);
#6801=AXIS2_PLACEMENT_3D('',#39977,#8175,#8176);
#6802=AXIS2_PLACEMENT_3D('',#39992,#8177,#8178);
#6803=AXIS2_PLACEMENT_3D('',#39993,#8179,#8180);
#6804=AXIS2_PLACEMENT_3D('',#39994,#8181,#8182);
#6805=AXIS2_PLACEMENT_3D('',#39995,#8183,#8184);
#6806=AXIS2_PLACEMENT_3D('',#39996,#8185,#8186);
#6807=AXIS2_PLACEMENT_3D('',#39997,#8187,#8188);
#6808=AXIS2_PLACEMENT_3D('',#39998,#8189,#8190);
#6809=AXIS2_PLACEMENT_3D('',#39999,#8191,#8192);
#6810=AXIS2_PLACEMENT_3D('',#40000,#8193,#8194);
#6811=AXIS2_PLACEMENT_3D('',#40001,#8195,#8196);
#6812=AXIS2_PLACEMENT_3D('',#40002,#8197,#8198);
#6813=AXIS2_PLACEMENT_3D('',#40003,#8199,#8200);
#6814=AXIS2_PLACEMENT_3D('',#40004,#8201,#8202);
#6815=AXIS2_PLACEMENT_3D('',#40005,#8203,#8204);
#6816=AXIS2_PLACEMENT_3D('',#40006,#8205,#8206);
#6817=AXIS2_PLACEMENT_3D('',#40007,#8207,#8208);
#6818=AXIS2_PLACEMENT_3D('',#40008,#8209,#8210);
#6819=AXIS2_PLACEMENT_3D('',#40009,#8211,#8212);
#6820=AXIS2_PLACEMENT_3D('',#40010,#8213,#8214);
#6821=AXIS2_PLACEMENT_3D('',#40011,#8215,#8216);
#6822=AXIS2_PLACEMENT_3D('',#40012,#8217,#8218);
#6823=AXIS2_PLACEMENT_3D('',#40013,#8219,#8220);
#6824=AXIS2_PLACEMENT_3D('',#40014,#8221,#8222);
#6825=AXIS2_PLACEMENT_3D('',#40015,#8223,#8224);
#6826=AXIS2_PLACEMENT_3D('',#40016,#8225,#8226);
#6827=AXIS2_PLACEMENT_3D('',#40017,#8227,#8228);
#6828=AXIS2_PLACEMENT_3D('',#40018,#8229,#8230);
#6829=AXIS2_PLACEMENT_3D('',#40019,#8231,#8232);
#6830=AXIS2_PLACEMENT_3D('',#40021,#8233,#8234);
#6831=AXIS2_PLACEMENT_3D('',#40024,#8236,#8237);
#6832=AXIS2_PLACEMENT_3D('',#40025,#8238,#8239);
#6833=AXIS2_PLACEMENT_3D('',#40027,#8240,#8241);
#6834=AXIS2_PLACEMENT_3D('',#40028,#8242,#8243);
#6835=AXIS2_PLACEMENT_3D('',#40029,#8244,#8245);
#6836=AXIS2_PLACEMENT_3D('',#40030,#8246,#8247);
#6837=AXIS2_PLACEMENT_3D('',#40031,#8248,#8249);
#6838=AXIS2_PLACEMENT_3D('',#40034,#8250,#8251);
#6839=AXIS2_PLACEMENT_3D('',#40035,#8252,#8253);
#6840=AXIS2_PLACEMENT_3D('',#40038,#8255,#8256);
#6841=AXIS2_PLACEMENT_3D('',#40039,#8257,#8258);
#6842=AXIS2_PLACEMENT_3D('',#40042,#8259,#8260);
#6843=AXIS2_PLACEMENT_3D('',#40043,#8261,#8262);
#6844=AXIS2_PLACEMENT_3D('',#40047,#8264,#8265);
#6845=AXIS2_PLACEMENT_3D('',#40048,#8266,#8267);
#6846=AXIS2_PLACEMENT_3D('',#40049,#8268,#8269);
#6847=AXIS2_PLACEMENT_3D('',#40051,#8271,#8272);
#6848=AXIS2_PLACEMENT_3D('',#40054,#8273,#8274);
#6849=AXIS2_PLACEMENT_3D('',#40055,#8275,#8276);
#6850=AXIS2_PLACEMENT_3D('',#40057,#8278,#8279);
#6851=AXIS2_PLACEMENT_3D('',#40060,#8280,#8281);
#6852=AXIS2_PLACEMENT_3D('',#40061,#8282,#8283);
#6853=AXIS2_PLACEMENT_3D('',#40065,#8285,#8286);
#6854=AXIS2_PLACEMENT_3D('',#40066,#8287,#8288);
#6855=AXIS2_PLACEMENT_3D('',#40067,#8289,#8290);
#6856=AXIS2_PLACEMENT_3D('',#40069,#8292,#8293);
#6857=AXIS2_PLACEMENT_3D('',#40072,#8294,#8295);
#6858=AXIS2_PLACEMENT_3D('',#40073,#8296,#8297);
#6859=AXIS2_PLACEMENT_3D('',#40075,#8299,#8300);
#6860=AXIS2_PLACEMENT_3D('',#40078,#8301,#8302);
#6861=AXIS2_PLACEMENT_3D('',#40079,#8303,#8304);
#6862=AXIS2_PLACEMENT_3D('',#40083,#8306,#8307);
#6863=AXIS2_PLACEMENT_3D('',#40084,#8308,#8309);
#6864=AXIS2_PLACEMENT_3D('',#40085,#8310,#8311);
#6865=AXIS2_PLACEMENT_3D('',#40087,#8313,#8314);
#6866=AXIS2_PLACEMENT_3D('',#40090,#8315,#8316);
#6867=AXIS2_PLACEMENT_3D('',#40091,#8317,#8318);
#6868=AXIS2_PLACEMENT_3D('',#40093,#8320,#8321);
#6869=AXIS2_PLACEMENT_3D('',#40096,#8322,#8323);
#6870=AXIS2_PLACEMENT_3D('',#40097,#8324,#8325);
#6871=AXIS2_PLACEMENT_3D('',#40101,#8327,#8328);
#6872=AXIS2_PLACEMENT_3D('',#40102,#8329,#8330);
#6873=AXIS2_PLACEMENT_3D('',#40103,#8331,#8332);
#6874=AXIS2_PLACEMENT_3D('',#40105,#8334,#8335);
#6875=AXIS2_PLACEMENT_3D('',#40108,#8336,#8337);
#6876=AXIS2_PLACEMENT_3D('',#40109,#8338,#8339);
#6877=AXIS2_PLACEMENT_3D('',#40111,#8341,#8342);
#6878=AXIS2_PLACEMENT_3D('',#40114,#8343,#8344);
#6879=AXIS2_PLACEMENT_3D('',#40115,#8345,#8346);
#6880=AXIS2_PLACEMENT_3D('',#40119,#8348,#8349);
#6881=AXIS2_PLACEMENT_3D('',#40120,#8350,#8351);
#6882=AXIS2_PLACEMENT_3D('',#40121,#8352,#8353);
#6883=AXIS2_PLACEMENT_3D('',#40123,#8355,#8356);
#6884=AXIS2_PLACEMENT_3D('',#40126,#8357,#8358);
#6885=AXIS2_PLACEMENT_3D('',#40127,#8359,#8360);
#6886=AXIS2_PLACEMENT_3D('',#40129,#8362,#8363);
#6887=AXIS2_PLACEMENT_3D('',#40132,#8364,#8365);
#6888=AXIS2_PLACEMENT_3D('',#40133,#8366,#8367);
#6889=AXIS2_PLACEMENT_3D('',#40137,#8369,#8370);
#6890=AXIS2_PLACEMENT_3D('',#40138,#8371,#8372);
#6891=AXIS2_PLACEMENT_3D('',#40139,#8373,#8374);
#6892=AXIS2_PLACEMENT_3D('',#40141,#8376,#8377);
#6893=AXIS2_PLACEMENT_3D('',#40144,#8378,#8379);
#6894=AXIS2_PLACEMENT_3D('',#40145,#8380,#8381);
#6895=AXIS2_PLACEMENT_3D('',#40147,#8383,#8384);
#6896=AXIS2_PLACEMENT_3D('',#40150,#8385,#8386);
#6897=AXIS2_PLACEMENT_3D('',#40151,#8387,#8388);
#6898=AXIS2_PLACEMENT_3D('',#40155,#8390,#8391);
#6899=AXIS2_PLACEMENT_3D('',#40156,#8392,#8393);
#6900=AXIS2_PLACEMENT_3D('',#40157,#8394,#8395);
#6901=AXIS2_PLACEMENT_3D('',#40159,#8397,#8398);
#6902=AXIS2_PLACEMENT_3D('',#40162,#8399,#8400);
#6903=AXIS2_PLACEMENT_3D('',#40163,#8401,#8402);
#6904=AXIS2_PLACEMENT_3D('',#40165,#8404,#8405);
#6905=AXIS2_PLACEMENT_3D('',#40168,#8406,#8407);
#6906=AXIS2_PLACEMENT_3D('',#40169,#8408,#8409);
#6907=AXIS2_PLACEMENT_3D('',#40173,#8411,#8412);
#6908=AXIS2_PLACEMENT_3D('',#40174,#8413,#8414);
#6909=AXIS2_PLACEMENT_3D('',#40175,#8415,#8416);
#6910=AXIS2_PLACEMENT_3D('',#40177,#8418,#8419);
#6911=AXIS2_PLACEMENT_3D('',#40180,#8420,#8421);
#6912=AXIS2_PLACEMENT_3D('',#40181,#8422,#8423);
#6913=AXIS2_PLACEMENT_3D('',#40183,#8425,#8426);
#6914=AXIS2_PLACEMENT_3D('',#40186,#8427,#8428);
#6915=AXIS2_PLACEMENT_3D('',#40187,#8429,#8430);
#6916=AXIS2_PLACEMENT_3D('',#40191,#8432,#8433);
#6917=AXIS2_PLACEMENT_3D('',#40192,#8434,#8435);
#6918=AXIS2_PLACEMENT_3D('',#40193,#8436,#8437);
#6919=AXIS2_PLACEMENT_3D('',#40195,#8439,#8440);
#6920=AXIS2_PLACEMENT_3D('',#40198,#8441,#8442);
#6921=AXIS2_PLACEMENT_3D('',#40199,#8443,#8444);
#6922=AXIS2_PLACEMENT_3D('',#40201,#8446,#8447);
#6923=AXIS2_PLACEMENT_3D('',#40204,#8448,#8449);
#6924=AXIS2_PLACEMENT_3D('',#40205,#8450,#8451);
#6925=AXIS2_PLACEMENT_3D('',#40209,#8453,#8454);
#6926=AXIS2_PLACEMENT_3D('',#40210,#8455,#8456);
#6927=AXIS2_PLACEMENT_3D('',#40211,#8457,#8458);
#6928=AXIS2_PLACEMENT_3D('',#40213,#8460,#8461);
#6929=AXIS2_PLACEMENT_3D('',#40216,#8462,#8463);
#6930=AXIS2_PLACEMENT_3D('',#40217,#8464,#8465);
#6931=AXIS2_PLACEMENT_3D('',#40219,#8467,#8468);
#6932=AXIS2_PLACEMENT_3D('',#40222,#8469,#8470);
#6933=AXIS2_PLACEMENT_3D('',#40223,#8471,#8472);
#6934=AXIS2_PLACEMENT_3D('',#40227,#8474,#8475);
#6935=AXIS2_PLACEMENT_3D('',#40228,#8476,#8477);
#6936=AXIS2_PLACEMENT_3D('',#40229,#8478,#8479);
#6937=AXIS2_PLACEMENT_3D('',#40231,#8481,#8482);
#6938=AXIS2_PLACEMENT_3D('',#40234,#8483,#8484);
#6939=AXIS2_PLACEMENT_3D('',#40235,#8485,#8486);
#6940=AXIS2_PLACEMENT_3D('',#40237,#8488,#8489);
#6941=AXIS2_PLACEMENT_3D('',#40240,#8490,#8491);
#6942=AXIS2_PLACEMENT_3D('',#40241,#8492,#8493);
#6943=AXIS2_PLACEMENT_3D('',#40245,#8495,#8496);
#6944=AXIS2_PLACEMENT_3D('',#40246,#8497,#8498);
#6945=AXIS2_PLACEMENT_3D('',#40247,#8499,#8500);
#6946=AXIS2_PLACEMENT_3D('',#40249,#8502,#8503);
#6947=AXIS2_PLACEMENT_3D('',#40252,#8504,#8505);
#6948=AXIS2_PLACEMENT_3D('',#40253,#8506,#8507);
#6949=AXIS2_PLACEMENT_3D('',#40255,#8509,#8510);
#6950=AXIS2_PLACEMENT_3D('',#40258,#8511,#8512);
#6951=AXIS2_PLACEMENT_3D('',#40259,#8513,#8514);
#6952=AXIS2_PLACEMENT_3D('',#40263,#8516,#8517);
#6953=AXIS2_PLACEMENT_3D('',#40264,#8518,#8519);
#6954=AXIS2_PLACEMENT_3D('',#40265,#8520,#8521);
#6955=AXIS2_PLACEMENT_3D('',#40267,#8523,#8524);
#6956=AXIS2_PLACEMENT_3D('',#40270,#8525,#8526);
#6957=AXIS2_PLACEMENT_3D('',#40271,#8527,#8528);
#6958=AXIS2_PLACEMENT_3D('',#40273,#8530,#8531);
#6959=AXIS2_PLACEMENT_3D('',#40276,#8532,#8533);
#6960=AXIS2_PLACEMENT_3D('',#40277,#8534,#8535);
#6961=AXIS2_PLACEMENT_3D('',#40281,#8537,#8538);
#6962=AXIS2_PLACEMENT_3D('',#40282,#8539,#8540);
#6963=AXIS2_PLACEMENT_3D('',#40283,#8541,#8542);
#6964=AXIS2_PLACEMENT_3D('',#40285,#8544,#8545);
#6965=AXIS2_PLACEMENT_3D('',#40288,#8546,#8547);
#6966=AXIS2_PLACEMENT_3D('',#40289,#8548,#8549);
#6967=AXIS2_PLACEMENT_3D('',#40291,#8551,#8552);
#6968=AXIS2_PLACEMENT_3D('',#40294,#8553,#8554);
#6969=AXIS2_PLACEMENT_3D('',#40295,#8555,#8556);
#6970=AXIS2_PLACEMENT_3D('',#40299,#8558,#8559);
#6971=AXIS2_PLACEMENT_3D('',#40300,#8560,#8561);
#6972=AXIS2_PLACEMENT_3D('',#40301,#8562,#8563);
#6973=AXIS2_PLACEMENT_3D('',#40303,#8565,#8566);
#6974=AXIS2_PLACEMENT_3D('',#40306,#8567,#8568);
#6975=AXIS2_PLACEMENT_3D('',#40307,#8569,#8570);
#6976=AXIS2_PLACEMENT_3D('',#40309,#8571,#8572);
#6977=AXIS2_PLACEMENT_3D('',#40310,#8573,#8574);
#6978=AXIS2_PLACEMENT_3D('',#40311,#8575,#8576);
#6979=AXIS2_PLACEMENT_3D('',#40314,#8577,#8578);
#6980=AXIS2_PLACEMENT_3D('',#40316,#8579,#8580);
#6981=AXIS2_PLACEMENT_3D('',#40318,#8581,#8582);
#6982=AXIS2_PLACEMENT_3D('',#40321,#8584,#8585);
#6983=AXIS2_PLACEMENT_3D('',#40323,#8586,#8587);
#6984=AXIS2_PLACEMENT_3D('',#40325,#8588,#8589);
#6985=AXIS2_PLACEMENT_3D('',#40326,#8590,#8591);
#6986=AXIS2_PLACEMENT_3D('',#40327,#8592,#8593);
#6987=AXIS2_PLACEMENT_3D('',#40329,#8595,#8596);
#6988=AXIS2_PLACEMENT_3D('',#40330,#8597,#8598);
#6989=AXIS2_PLACEMENT_3D('',#40334,#8601,#8602);
#6990=AXIS2_PLACEMENT_3D('',#40338,#8605,#8606);
#6991=AXIS2_PLACEMENT_3D('',#40342,#8609,#8610);
#6992=AXIS2_PLACEMENT_3D('',#40346,#8613,#8614);
#6993=AXIS2_PLACEMENT_3D('',#40350,#8617,#8618);
#6994=AXIS2_PLACEMENT_3D('',#40354,#8621,#8622);
#6995=AXIS2_PLACEMENT_3D('',#40357,#8623,#8624);
#6996=AXIS2_PLACEMENT_3D('',#40359,#8625,#8626);
#6997=AXIS2_PLACEMENT_3D('',#40361,#8627,#8628);
#6998=AXIS2_PLACEMENT_3D('',#40363,#8629,#8630);
#6999=AXIS2_PLACEMENT_3D('',#40365,#8631,#8632);
#7000=AXIS2_PLACEMENT_3D('',#40366,#8633,#8634);
#7001=AXIS2_PLACEMENT_3D('',#40367,#8635,#8636);
#7002=AXIS2_PLACEMENT_3D('',#40375,#8637,#8638);
#7003=AXIS2_PLACEMENT_3D('',#40383,#8639,#8640);
#7004=AXIS2_PLACEMENT_3D('',#40391,#8641,#8642);
#7005=AXIS2_PLACEMENT_3D('',#40399,#8643,#8644);
#7006=AXIS2_PLACEMENT_3D('',#40407,#8645,#8646);
#7007=AXIS2_PLACEMENT_3D('',#40415,#8647,#8648);
#7008=AXIS2_PLACEMENT_3D('',#40418,#8651,#8652);
#7009=AXIS2_PLACEMENT_3D('',#40420,#8654,#8655);
#7010=AXIS2_PLACEMENT_3D('',#40422,#8657,#8658);
#7011=AXIS2_PLACEMENT_3D('',#40424,#8660,#8661);
#7012=AXIS2_PLACEMENT_3D('',#40426,#8663,#8664);
#7013=AXIS2_PLACEMENT_3D('',#40427,#8665,#8666);
#7014=AXIS2_PLACEMENT_3D('',#40428,#8667,#8668);
#7015=AXIS2_PLACEMENT_3D('',#40429,#8669,#8670);
#7016=AXIS2_PLACEMENT_3D('',#40431,#8671,#8672);
#7017=AXIS2_PLACEMENT_3D('',#40434,#8674,#8675);
#7018=AXIS2_PLACEMENT_3D('',#40435,#8676,#8677);
#7019=AXIS2_PLACEMENT_3D('',#40438,#8678,#8679);
#7020=AXIS2_PLACEMENT_3D('',#40442,#8681,#8682);
#7021=AXIS2_PLACEMENT_3D('',#40444,#8684,#8685);
#7022=AXIS2_PLACEMENT_3D('',#40446,#8686,#8687);
#7023=AXIS2_PLACEMENT_3D('',#40449,#8689,#8690);
#7024=AXIS2_PLACEMENT_3D('',#40450,#8691,#8692);
#7025=AXIS2_PLACEMENT_3D('',#40459,#8697,#8698);
#7026=AXIS2_PLACEMENT_3D('',#40465,#8702,#8703);
#7027=AXIS2_PLACEMENT_3D('',#40471,#8707,#8708);
#7028=AXIS2_PLACEMENT_3D('',#40474,#8711,#8712);
#7029=AXIS2_PLACEMENT_3D('',#40477,#8713,#8714);
#7030=AXIS2_PLACEMENT_3D('',#40481,#8716,#8717);
#7031=AXIS2_PLACEMENT_3D('',#40483,#8719,#8720);
#7032=AXIS2_PLACEMENT_3D('',#40489,#8724,#8725);
#7033=AXIS2_PLACEMENT_3D('',#40493,#8728,#8729);
#7034=AXIS2_PLACEMENT_3D('',#40497,#8732,#8733);
#7035=AXIS2_PLACEMENT_3D('',#40499,#8735,#8736);
#7036=AXIS2_PLACEMENT_3D('',#40500,#8737,#8738);
#7037=AXIS2_PLACEMENT_3D('',#40501,#8739,#8740);
#7038=AXIS2_PLACEMENT_3D('',#40502,#8741,#8742);
#7039=AXIS2_PLACEMENT_3D('',#40503,#8743,#8744);
#7040=AXIS2_PLACEMENT_3D('',#40504,#8745,#8746);
#7041=AXIS2_PLACEMENT_3D('',#40505,#8747,#8748);
#7042=AXIS2_PLACEMENT_3D('',#40506,#8749,#8750);
#7043=AXIS2_PLACEMENT_3D('',#40507,#8751,#8752);
#7044=AXIS2_PLACEMENT_3D('',#40511,#8754,#8755);
#7045=AXIS2_PLACEMENT_3D('',#40512,#8756,#8757);
#7046=AXIS2_PLACEMENT_3D('',#40513,#8758,#8759);
#7047=AXIS2_PLACEMENT_3D('',#40515,#8760,#8761);
#7048=AXIS2_PLACEMENT_3D('',#40518,#8763,#8764);
#7049=AXIS2_PLACEMENT_3D('',#40519,#8765,#8766);
#7050=AXIS2_PLACEMENT_3D('',#40521,#8768,#8769);
#7051=AXIS2_PLACEMENT_3D('',#40523,#8771,#8772);
#7052=AXIS2_PLACEMENT_3D('',#40526,#8775,#8776);
#7053=AXIS2_PLACEMENT_3D('',#40528,#8778,#8779);
#7054=AXIS2_PLACEMENT_3D('',#40530,#8781,#8782);
#7055=AXIS2_PLACEMENT_3D('',#40531,#8783,#8784);
#7056=AXIS2_PLACEMENT_3D('',#40532,#8785,#8786);
#7057=AXIS2_PLACEMENT_3D('',#40535,#8787,#8788);
#7058=AXIS2_PLACEMENT_3D('',#40552,#8789,#8790);
#7059=AXIS2_PLACEMENT_3D('',#40553,#8791,#8792);
#7060=AXIS2_PLACEMENT_3D('',#40554,#8793,#8794);
#7061=AXIS2_PLACEMENT_3D('',#40557,#8795,#8796);
#7062=AXIS2_PLACEMENT_3D('',#40559,#8797,#8798);
#7063=AXIS2_PLACEMENT_3D('',#40561,#8799,#8800);
#7064=AXIS2_PLACEMENT_3D('',#40562,#8801,#8802);
#7065=AXIS2_PLACEMENT_3D('',#40563,#8803,#8804);
#7066=AXIS2_PLACEMENT_3D('',#40566,#8805,#8806);
#7067=AXIS2_PLACEMENT_3D('',#40583,#8807,#8808);
#7068=AXIS2_PLACEMENT_3D('',#40584,#8809,#8810);
#7069=AXIS2_PLACEMENT_3D('',#40585,#8811,#8812);
#7070=AXIS2_PLACEMENT_3D('',#40588,#8813,#8814);
#7071=AXIS2_PLACEMENT_3D('',#40590,#8815,#8816);
#7072=AXIS2_PLACEMENT_3D('',#40592,#8817,#8818);
#7073=AXIS2_PLACEMENT_3D('',#40593,#8819,#8820);
#7074=AXIS2_PLACEMENT_3D('',#40594,#8821,#8822);
#7075=AXIS2_PLACEMENT_3D('',#40597,#8823,#8824);
#7076=AXIS2_PLACEMENT_3D('',#40598,#8825,#8826);
#7077=AXIS2_PLACEMENT_3D('',#40601,#8828,#8829);
#7078=AXIS2_PLACEMENT_3D('',#40602,#8830,#8831);
#7079=AXIS2_PLACEMENT_3D('',#40604,#8832,#8833);
#7080=AXIS2_PLACEMENT_3D('',#40607,#8835,#8836);
#7081=AXIS2_PLACEMENT_3D('',#40608,#8837,#8838);
#7082=AXIS2_PLACEMENT_3D('',#40611,#8839,#8840);
#7083=AXIS2_PLACEMENT_3D('',#40612,#8841,#8842);
#7084=AXIS2_PLACEMENT_3D('',#40615,#8844,#8845);
#7085=AXIS2_PLACEMENT_3D('',#40616,#8846,#8847);
#7086=AXIS2_PLACEMENT_3D('',#40618,#8848,#8849);
#7087=AXIS2_PLACEMENT_3D('',#40621,#8851,#8852);
#7088=AXIS2_PLACEMENT_3D('',#40622,#8853,#8854);
#7089=AXIS2_PLACEMENT_3D('',#40625,#8855,#8856);
#7090=AXIS2_PLACEMENT_3D('',#40626,#8857,#8858);
#7091=AXIS2_PLACEMENT_3D('',#40629,#8860,#8861);
#7092=AXIS2_PLACEMENT_3D('',#40630,#8862,#8863);
#7093=AXIS2_PLACEMENT_3D('',#40632,#8864,#8865);
#7094=AXIS2_PLACEMENT_3D('',#40635,#8867,#8868);
#7095=AXIS2_PLACEMENT_3D('',#40636,#8869,#8870);
#7096=AXIS2_PLACEMENT_3D('',#40639,#8871,#8872);
#7097=AXIS2_PLACEMENT_3D('',#40640,#8873,#8874);
#7098=AXIS2_PLACEMENT_3D('',#40643,#8876,#8877);
#7099=AXIS2_PLACEMENT_3D('',#40644,#8878,#8879);
#7100=AXIS2_PLACEMENT_3D('',#40646,#8880,#8881);
#7101=AXIS2_PLACEMENT_3D('',#40649,#8883,#8884);
#7102=AXIS2_PLACEMENT_3D('',#40650,#8885,#8886);
#7103=AXIS2_PLACEMENT_3D('',#40653,#8887,#8888);
#7104=AXIS2_PLACEMENT_3D('',#40654,#8889,#8890);
#7105=AXIS2_PLACEMENT_3D('',#40657,#8892,#8893);
#7106=AXIS2_PLACEMENT_3D('',#40658,#8894,#8895);
#7107=AXIS2_PLACEMENT_3D('',#40660,#8896,#8897);
#7108=AXIS2_PLACEMENT_3D('',#40663,#8899,#8900);
#7109=AXIS2_PLACEMENT_3D('',#40664,#8901,#8902);
#7110=AXIS2_PLACEMENT_3D('',#40666,#8904,#8905);
#7111=AXIS2_PLACEMENT_3D('',#40668,#8907,#8908);
#7112=AXIS2_PLACEMENT_3D('',#40670,#8910,#8911);
#7113=AXIS2_PLACEMENT_3D('',#40672,#8913,#8914);
#7114=AXIS2_PLACEMENT_3D('',#40674,#8916,#8917);
#7115=AXIS2_PLACEMENT_3D('',#40677,#8918,#8919);
#7116=AXIS2_PLACEMENT_3D('',#40681,#8921,#8922);
#7117=AXIS2_PLACEMENT_3D('',#40683,#8924,#8925);
#7118=AXIS2_PLACEMENT_3D('',#40686,#8926,#8927);
#7119=AXIS2_PLACEMENT_3D('',#40690,#8929,#8930);
#7120=AXIS2_PLACEMENT_3D('',#40692,#8932,#8933);
#7121=AXIS2_PLACEMENT_3D('',#40698,#8936,#8937);
#7122=AXIS2_PLACEMENT_3D('',#40701,#8939,#8940);
#7123=AXIS2_PLACEMENT_3D('',#40704,#8942,#8943);
#7124=AXIS2_PLACEMENT_3D('',#40705,#8944,#8945);
#7125=AXIS2_PLACEMENT_3D('',#40711,#8948,#8949);
#7126=AXIS2_PLACEMENT_3D('',#40714,#8951,#8952);
#7127=AXIS2_PLACEMENT_3D('',#40717,#8954,#8955);
#7128=AXIS2_PLACEMENT_3D('',#40718,#8956,#8957);
#7129=AXIS2_PLACEMENT_3D('',#40722,#8961,#8962);
#7130=AXIS2_PLACEMENT_3D('',#40724,#8964,#8965);
#7131=AXIS2_PLACEMENT_3D('',#40726,#8966,#8967);
#7132=AXIS2_PLACEMENT_3D('',#40729,#8969,#8970);
#7133=AXIS2_PLACEMENT_3D('',#40730,#8971,#8972);
#7134=AXIS2_PLACEMENT_3D('',#40733,#8975,#8976);
#7135=AXIS2_PLACEMENT_3D('',#40737,#8980,#8981);
#7136=AXIS2_PLACEMENT_3D('',#40739,#8983,#8984);
#7137=AXIS2_PLACEMENT_3D('',#40742,#8987,#8988);
#7138=AXIS2_PLACEMENT_3D('',#40743,#8989,#8990);
#7139=AXIS2_PLACEMENT_3D('',#40744,#8991,#8992);
#7140=AXIS2_PLACEMENT_3D('',#40745,#8993,#8994);
#7141=AXIS2_PLACEMENT_3D('',#40746,#8995,#8996);
#7142=AXIS2_PLACEMENT_3D('',#40747,#8997,#8998);
#7143=AXIS2_PLACEMENT_3D('',#40748,#8999,#9000);
#7144=AXIS2_PLACEMENT_3D('',#40749,#9001,#9002);
#7145=AXIS2_PLACEMENT_3D('',#40750,#9003,#9004);
#7146=AXIS2_PLACEMENT_3D('',#40751,#9005,#9006);
#7147=AXIS2_PLACEMENT_3D('',#40752,#9007,#9008);
#7148=AXIS2_PLACEMENT_3D('',#40753,#9009,#9010);
#7149=AXIS2_PLACEMENT_3D('',#40754,#9011,#9012);
#7150=AXIS2_PLACEMENT_3D('',#40755,#9013,#9014);
#7151=AXIS2_PLACEMENT_3D('',#40756,#9015,#9016);
#7152=AXIS2_PLACEMENT_3D('',#40757,#9017,#9018);
#7153=AXIS2_PLACEMENT_3D('',#40758,#9019,#9020);
#7154=AXIS2_PLACEMENT_3D('',#40759,#9021,#9022);
#7155=AXIS2_PLACEMENT_3D('',#40760,#9023,#9024);
#7156=AXIS2_PLACEMENT_3D('',#40761,#9025,#9026);
#7157=AXIS2_PLACEMENT_3D('',#40762,#9027,#9028);
#7158=AXIS2_PLACEMENT_3D('',#40763,#9029,#9030);
#7159=AXIS2_PLACEMENT_3D('',#40764,#9031,#9032);
#7160=AXIS2_PLACEMENT_3D('',#40765,#9033,#9034);
#7161=AXIS2_PLACEMENT_3D('',#40766,#9035,#9036);
#7162=AXIS2_PLACEMENT_3D('',#40767,#9037,#9038);
#7163=AXIS2_PLACEMENT_3D('',#40768,#9039,#9040);
#7164=AXIS2_PLACEMENT_3D('',#40769,#9041,#9042);
#7165=AXIS2_PLACEMENT_3D('',#40770,#9043,#9044);
#7166=AXIS2_PLACEMENT_3D('',#40771,#9045,#9046);
#7167=AXIS2_PLACEMENT_3D('',#40772,#9047,#9048);
#7168=AXIS2_PLACEMENT_3D('',#40773,#9049,#9050);
#7169=AXIS2_PLACEMENT_3D('',#40774,#9051,#9052);
#7170=AXIS2_PLACEMENT_3D('',#40775,#9053,#9054);
#7171=AXIS2_PLACEMENT_3D('',#40776,#9055,#9056);
#7172=AXIS2_PLACEMENT_3D('',#40777,#9057,#9058);
#7173=AXIS2_PLACEMENT_3D('',#40778,#9059,#9060);
#7174=AXIS2_PLACEMENT_3D('',#40779,#9061,#9062);
#7175=AXIS2_PLACEMENT_3D('',#40780,#9063,#9064);
#7176=AXIS2_PLACEMENT_3D('',#40781,#9065,#9066);
#7177=AXIS2_PLACEMENT_3D('',#40782,#9067,#9068);
#7178=AXIS2_PLACEMENT_3D('',#40783,#9069,#9070);
#7179=AXIS2_PLACEMENT_3D('',#40784,#9071,#9072);
#7180=AXIS2_PLACEMENT_3D('',#40785,#9073,#9074);
#7181=AXIS2_PLACEMENT_3D('',#40786,#9075,#9076);
#7182=AXIS2_PLACEMENT_3D('',#40787,#9077,#9078);
#7183=AXIS2_PLACEMENT_3D('',#40788,#9079,#9080);
#7184=AXIS2_PLACEMENT_3D('',#40789,#9081,#9082);
#7185=DIRECTION('axis',(0.,0.,1.));
#7186=DIRECTION('refdir',(1.,0.,0.));
#7187=DIRECTION('axis',(0.,0.,1.));
#7188=DIRECTION('refdir',(1.,0.,0.));
#7189=DIRECTION('center_axis',(0.,1.,0.));
#7190=DIRECTION('ref_axis',(0.,0.,1.));
#7191=DIRECTION('',(0.,1.,0.));
#7192=DIRECTION('center_axis',(0.,1.,0.));
#7193=DIRECTION('ref_axis',(0.,0.,-1.));
#7194=DIRECTION('',(0.,1.,0.));
#7195=DIRECTION('center_axis',(0.,1.,0.));
#7196=DIRECTION('ref_axis',(0.,0.,1.));
#7197=DIRECTION('center_axis',(0.,1.,0.));
#7198=DIRECTION('ref_axis',(0.,0.,1.));
#7199=DIRECTION('',(0.,1.,0.));
#7200=DIRECTION('center_axis',(0.,1.,0.));
#7201=DIRECTION('ref_axis',(0.,0.,1.));
#7202=DIRECTION('',(0.,1.,0.));
#7203=DIRECTION('center_axis',(0.,1.,0.));
#7204=DIRECTION('ref_axis',(0.,0.,1.));
#7205=DIRECTION('',(0.,1.,0.));
#7206=DIRECTION('center_axis',(0.,1.,0.));
#7207=DIRECTION('ref_axis',(0.,0.,1.));
#7208=DIRECTION('',(0.,1.,0.));
#7209=DIRECTION('center_axis',(0.,1.,0.));
#7210=DIRECTION('ref_axis',(0.,0.,1.));
#7211=DIRECTION('',(0.,1.,0.));
#7212=DIRECTION('center_axis',(0.,1.,0.));
#7213=DIRECTION('ref_axis',(0.,0.,1.));
#7214=DIRECTION('',(0.,1.,0.));
#7215=DIRECTION('center_axis',(0.,1.,0.));
#7216=DIRECTION('ref_axis',(0.,0.,1.));
#7217=DIRECTION('',(0.,1.,0.));
#7218=DIRECTION('center_axis',(0.,1.,0.));
#7219=DIRECTION('ref_axis',(0.,0.,1.));
#7220=DIRECTION('',(0.,1.,0.));
#7221=DIRECTION('center_axis',(0.,1.,0.));
#7222=DIRECTION('ref_axis',(0.,0.,1.));
#7223=DIRECTION('',(0.,1.,0.));
#7224=DIRECTION('center_axis',(0.,1.,0.));
#7225=DIRECTION('ref_axis',(0.,0.,1.));
#7226=DIRECTION('',(0.,1.,0.));
#7227=DIRECTION('center_axis',(0.,1.,0.));
#7228=DIRECTION('ref_axis',(0.,0.,1.));
#7229=DIRECTION('',(0.,1.,0.));
#7230=DIRECTION('center_axis',(0.,1.,0.));
#7231=DIRECTION('ref_axis',(0.,0.,1.));
#7232=DIRECTION('',(0.,1.,0.));
#7233=DIRECTION('center_axis',(0.,1.,0.));
#7234=DIRECTION('ref_axis',(0.,0.,1.));
#7235=DIRECTION('',(0.,1.,0.));
#7236=DIRECTION('center_axis',(0.,1.,0.));
#7237=DIRECTION('ref_axis',(0.,0.,1.));
#7238=DIRECTION('',(0.,1.,0.));
#7239=DIRECTION('center_axis',(0.,1.,0.));
#7240=DIRECTION('ref_axis',(0.,0.,1.));
#7241=DIRECTION('',(0.,1.,0.));
#7242=DIRECTION('center_axis',(0.,1.,0.));
#7243=DIRECTION('ref_axis',(0.,0.,1.));
#7244=DIRECTION('',(0.,1.,0.));
#7245=DIRECTION('center_axis',(0.,1.,0.));
#7246=DIRECTION('ref_axis',(0.,0.,1.));
#7247=DIRECTION('',(0.,1.,0.));
#7248=DIRECTION('center_axis',(0.,1.,0.));
#7249=DIRECTION('ref_axis',(0.,0.,1.));
#7250=DIRECTION('',(0.,1.,0.));
#7251=DIRECTION('center_axis',(0.,1.,0.));
#7252=DIRECTION('ref_axis',(0.,0.,1.));
#7253=DIRECTION('',(0.,1.,0.));
#7254=DIRECTION('center_axis',(0.,1.,0.));
#7255=DIRECTION('ref_axis',(0.,0.,1.));
#7256=DIRECTION('',(0.,1.,0.));
#7257=DIRECTION('center_axis',(0.,1.,0.));
#7258=DIRECTION('ref_axis',(0.,0.,1.));
#7259=DIRECTION('',(0.,1.,0.));
#7260=DIRECTION('center_axis',(0.,-1.,0.));
#7261=DIRECTION('ref_axis',(1.77635683940025E-15,0.,1.));
#7262=DIRECTION('center_axis',(0.,1.,0.));
#7263=DIRECTION('ref_axis',(0.,0.,1.));
#7264=DIRECTION('center_axis',(0.,1.,0.));
#7265=DIRECTION('ref_axis',(0.,0.,1.));
#7266=DIRECTION('center_axis',(0.,1.,0.));
#7267=DIRECTION('ref_axis',(0.,0.,1.));
#7268=DIRECTION('center_axis',(-1.,0.,1.22464679914735E-16));
#7269=DIRECTION('ref_axis',(-1.22464679914735E-16,0.,-1.));
#7270=DIRECTION('center_axis',(0.,-1.,0.));
#7271=DIRECTION('ref_axis',(0.,0.,1.));
#7272=DIRECTION('center_axis',(0.,1.,0.));
#7273=DIRECTION('ref_axis',(0.,0.,1.));
#7274=DIRECTION('center_axis',(0.,1.,0.));
#7275=DIRECTION('ref_axis',(0.,0.,1.));
#7276=DIRECTION('center_axis',(-1.,0.,1.22464679914735E-16));
#7277=DIRECTION('ref_axis',(-1.22464679914735E-16,0.,-1.));
#7278=DIRECTION('center_axis',(0.,-1.,0.));
#7279=DIRECTION('ref_axis',(0.,0.,1.));
#7280=DIRECTION('center_axis',(0.,-1.,0.));
#7281=DIRECTION('ref_axis',(0.,0.,1.));
#7282=DIRECTION('center_axis',(9.81918948666102E-17,1.,1.70073350800434E-16));
#7283=DIRECTION('ref_axis',(0.,0.,1.));
#7284=DIRECTION('center_axis',(-9.81918948666102E-17,-1.,-1.70073350800434E-16));
#7285=DIRECTION('ref_axis',(-1.66998245814083E-32,-1.70073350800434E-16,
1.));
#7286=DIRECTION('center_axis',(0.866025403784444,0.,-0.499999999999991));
#7287=DIRECTION('ref_axis',(-0.499999999999991,0.,-0.866025403784444));
#7288=DIRECTION('center_axis',(9.81918948666102E-17,1.,1.70073350800434E-16));
#7289=DIRECTION('ref_axis',(-1.66998245814083E-32,-1.70073350800434E-16,
1.));
#7290=DIRECTION('center_axis',(0.499999999999993,2.60208521396517E-15,0.866025403784443));
#7291=DIRECTION('ref_axis',(0.866025403784443,2.19996346842361E-31,-0.499999999999993));
#7292=DIRECTION('center_axis',(-0.333155558300967,0.745673853566471,-0.577042353801262));
#7293=DIRECTION('ref_axis',(-2.59234872084442E-17,0.612005054639087,0.790853850655232));
#7294=DIRECTION('center_axis',(-0.333155558300967,0.745673853566471,-0.577042353801262));
#7295=DIRECTION('ref_axis',(-3.14843324929394E-17,0.612005054639087,0.790853850655232));
#7296=DIRECTION('',(0.333155558300967,-0.745673853566471,0.577042353801262));
#7297=DIRECTION('center_axis',(-0.393636804027377,0.616603816125408,-0.681798944304475));
#7298=DIRECTION('ref_axis',(0.308301907969892,0.787273608054776,0.533994568888617));
#7299=DIRECTION('',(-0.333155558300967,0.745673853566471,-0.577042353801262));
#7300=DIRECTION('center_axis',(0.,1.,0.));
#7301=DIRECTION('ref_axis',(0.,0.,1.));
#7302=DIRECTION('',(0.,-1.,0.));
#7303=DIRECTION('center_axis',(0.,1.,0.));
#7304=DIRECTION('ref_axis',(0.,0.,1.));
#7305=DIRECTION('',(0.,1.,0.));
#7306=DIRECTION('center_axis',(0.,-1.,0.));
#7307=DIRECTION('ref_axis',(0.,0.,-1.));
#7308=DIRECTION('center_axis',(0.,-1.,0.));
#7309=DIRECTION('ref_axis',(0.,0.,-1.));
#7310=DIRECTION('',(0.,1.,0.));
#7311=DIRECTION('center_axis',(9.81918948666125E-17,1.,-1.70073350800433E-16));
#7312=DIRECTION('ref_axis',(1.66998245814086E-32,1.70073350800433E-16,1.));
#7313=DIRECTION('',(0.,-1.,0.));
#7314=DIRECTION('center_axis',(0.333155558300975,-0.745673853566471,-0.577042353801257));
#7315=DIRECTION('ref_axis',(-7.49624866032534E-17,0.612005054639084,-0.790853850655234));
#7316=DIRECTION('center_axis',(0.393636804027381,-0.616603816125443,-0.681798944304441));
#7317=DIRECTION('ref_axis',(0.308301907935341,0.787273608054748,-0.533994568908606));
#7318=DIRECTION('',(-0.333155558300975,0.745673853566471,0.577042353801257));
#7319=DIRECTION('center_axis',(0.333155558300975,-0.745673853566471,-0.577042353801257));
#7320=DIRECTION('ref_axis',(-2.33037419662539E-17,0.612005054639083,-0.790853850655235));
#7321=DIRECTION('',(0.333155558300975,-0.745673853566471,-0.577042353801257));
#7322=DIRECTION('center_axis',(0.,1.,0.));
#7323=DIRECTION('ref_axis',(0.,0.,1.));
#7324=DIRECTION('',(-8.65956056235492E-17,0.707106781186549,-0.707106781186546));
#7325=DIRECTION('center_axis',(0.,-1.,0.));
#7326=DIRECTION('ref_axis',(0.,0.,1.));
#7327=DIRECTION('center_axis',(0.,-1.,0.));
#7328=DIRECTION('ref_axis',(0.,0.,-1.));
#7329=DIRECTION('center_axis',(0.,1.,0.));
#7330=DIRECTION('ref_axis',(8.88178419700125E-16,0.,-1.));
#7331=DIRECTION('center_axis',(0.,-1.,0.));
#7332=DIRECTION('ref_axis',(0.,0.,-1.));
#7333=DIRECTION('center_axis',(9.81918948666102E-17,1.,1.70073350800434E-16));
#7334=DIRECTION('ref_axis',(2.91276184253032E-34,-1.77192702184564E-16,
1.));
#7335=DIRECTION('center_axis',(9.81918948666102E-17,1.,1.70073350800434E-16));
#7336=DIRECTION('ref_axis',(7.25831191047442E-34,-1.70073350800434E-16,
1.));
#7337=DIRECTION('center_axis',(-9.81918948666102E-17,-1.,-1.70073350800434E-16));
#7338=DIRECTION('ref_axis',(-1.77635683940025E-15,-1.70073350800434E-16,
1.));
#7339=DIRECTION('center_axis',(-9.81918948666102E-17,-1.,-1.70073350800434E-16));
#7340=DIRECTION('ref_axis',(-1.77635683940025E-15,-1.70073350800434E-16,
1.));
#7341=DIRECTION('center_axis',(-1.96383789733223E-16,1.,0.));
#7342=DIRECTION('ref_axis',(-1.,-1.77192702184564E-16,0.));
#7343=DIRECTION('center_axis',(-1.96383789733223E-16,1.,0.));
#7344=DIRECTION('ref_axis',(-1.,-1.96383789733223E-16,0.));
#7345=DIRECTION('center_axis',(1.96383789733223E-16,-1.,0.));
#7346=DIRECTION('ref_axis',(-1.,-1.96383789733223E-16,-3.5527136788005E-15));
#7347=DIRECTION('center_axis',(0.,1.,0.));
#7348=DIRECTION('ref_axis',(0.,0.,1.));
#7349=DIRECTION('center_axis',(0.866025403784436,0.,0.500000000000004));
#7350=DIRECTION('ref_axis',(0.500000000000004,0.,-0.866025403784436));
#7351=DIRECTION('center_axis',(-0.866025403784436,0.,-0.500000000000004));
#7352=DIRECTION('ref_axis',(-0.500000000000004,0.,0.866025403784436));
#7353=DIRECTION('',(0.866025403784436,0.,0.500000000000004));
#7354=DIRECTION('center_axis',(-0.866025403784436,0.,-0.500000000000004));
#7355=DIRECTION('ref_axis',(-0.500000000000004,0.,0.866025403784436));
#7356=DIRECTION('center_axis',(-0.866025403784443,0.,0.499999999999992));
#7357=DIRECTION('ref_axis',(0.499999999999992,0.,0.866025403784443));
#7358=DIRECTION('center_axis',(0.866025403784443,0.,-0.499999999999992));
#7359=DIRECTION('ref_axis',(-0.499999999999992,0.,-0.866025403784443));
#7360=DIRECTION('',(-0.866025403784443,0.,0.499999999999992));
#7361=DIRECTION('center_axis',(0.866025403784443,0.,-0.499999999999992));
#7362=DIRECTION('ref_axis',(-0.499999999999992,0.,-0.866025403784443));
#7363=DIRECTION('center_axis',(0.,0.,-1.));
#7364=DIRECTION('ref_axis',(-1.,0.,0.));
#7365=DIRECTION('center_axis',(0.,0.,1.));
#7366=DIRECTION('ref_axis',(1.,0.,0.));
#7367=DIRECTION('',(0.,0.,-1.));
#7368=DIRECTION('center_axis',(0.,0.,1.));
#7369=DIRECTION('ref_axis',(1.,0.,0.));
#7370=DIRECTION('center_axis',(0.,-1.,0.));
#7371=DIRECTION('ref_axis',(0.,0.,-1.));
#7372=DIRECTION('',(0.,1.,0.));
#7373=DIRECTION('',(0.,1.,0.));
#7374=DIRECTION('center_axis',(0.,1.,0.));
#7375=DIRECTION('ref_axis',(-8.88178419700125E-16,0.,-1.));
#7376=DIRECTION('',(0.,1.,0.));
#7377=DIRECTION('center_axis',(0.,1.,0.));
#7378=DIRECTION('ref_axis',(-8.88178419700125E-16,0.,-1.));
#7379=DIRECTION('',(0.,-1.,0.));
#7380=DIRECTION('',(0.,-1.,0.));
#7381=DIRECTION('center_axis',(-9.81918948666125E-17,-1.,1.70073350800433E-16));
#7382=DIRECTION('ref_axis',(-1.18319748428791E-33,1.70073350800433E-16,
1.));
#7383=DIRECTION('',(0.,1.,0.));
#7384=DIRECTION('',(0.,-1.,0.));
#7385=DIRECTION('',(0.,1.,0.));
#7386=DIRECTION('center_axis',(0.,1.,0.));
#7387=DIRECTION('ref_axis',(0.,0.,-1.));
#7388=DIRECTION('center_axis',(0.,1.,0.));
#7389=DIRECTION('ref_axis',(0.,0.,1.));
#7390=DIRECTION('center_axis',(0.,1.,0.));
#7391=DIRECTION('ref_axis',(0.,0.,1.));
#7392=DIRECTION('center_axis',(0.,1.,0.));
#7393=DIRECTION('ref_axis',(0.,0.,1.));
#7394=DIRECTION('center_axis',(0.,1.,0.));
#7395=DIRECTION('ref_axis',(0.,0.,1.));
#7396=DIRECTION('center_axis',(0.,1.,0.));
#7397=DIRECTION('ref_axis',(0.,0.,1.));
#7398=DIRECTION('center_axis',(0.,1.,0.));
#7399=DIRECTION('ref_axis',(0.,0.,1.));
#7400=DIRECTION('center_axis',(0.,1.,0.));
#7401=DIRECTION('ref_axis',(0.,0.,1.));
#7402=DIRECTION('center_axis',(-1.36592399683213E-16,0.,1.));
#7403=DIRECTION('ref_axis',(1.,0.,1.36592399683213E-16));
#7404=DIRECTION('',(0.,-1.,0.));
#7405=DIRECTION('',(1.,0.,1.36592399683213E-16));
#7406=DIRECTION('',(0.,1.,0.));
#7407=DIRECTION('center_axis',(-0.866025403784439,0.,0.5));
#7408=DIRECTION('ref_axis',(0.5,0.,0.866025403784439));
#7409=DIRECTION('',(0.,-1.,0.));
#7410=DIRECTION('',(0.5,0.,0.866025403784439));
#7411=DIRECTION('',(0.,1.,0.));
#7412=DIRECTION('center_axis',(-0.866025403784439,0.,-0.5));
#7413=DIRECTION('ref_axis',(-0.5,0.,0.866025403784439));
#7414=DIRECTION('',(0.,-1.,0.));
#7415=DIRECTION('',(-0.5,0.,0.866025403784439));
#7416=DIRECTION('',(0.,1.,0.));
#7417=DIRECTION('center_axis',(0.,0.,-1.));
#7418=DIRECTION('ref_axis',(-1.,0.,0.));
#7419=DIRECTION('',(0.,-1.,0.));
#7420=DIRECTION('',(-1.,0.,0.));
#7421=DIRECTION('',(0.,1.,0.));
#7422=DIRECTION('center_axis',(0.866025403784439,0.,-0.5));
#7423=DIRECTION('ref_axis',(-0.5,0.,-0.866025403784439));
#7424=DIRECTION('',(0.,-1.,0.));
#7425=DIRECTION('',(-0.5,0.,-0.866025403784439));
#7426=DIRECTION('',(0.,1.,0.));
#7427=DIRECTION('center_axis',(0.866025403784439,0.,0.5));
#7428=DIRECTION('ref_axis',(0.5,0.,-0.866025403784439));
#7429=DIRECTION('',(0.,-1.,0.));
#7430=DIRECTION('',(0.5,0.,-0.866025403784439));
#7431=DIRECTION('',(0.,1.,0.));
#7432=DIRECTION('center_axis',(0.,1.,0.));
#7433=DIRECTION('ref_axis',(0.,0.,1.));
#7434=DIRECTION('center_axis',(0.,1.,0.));
#7435=DIRECTION('ref_axis',(0.,0.,1.));
#7436=DIRECTION('center_axis',(0.,-1.,0.));
#7437=DIRECTION('ref_axis',(-0.297077312093106,0.,0.954853428877718));
#7438=DIRECTION('center_axis',(0.,0.,-1.));
#7439=DIRECTION('ref_axis',(-1.,0.,0.));
#7440=DIRECTION('',(0.,-1.,0.));
#7441=DIRECTION('',(1.,1.96383789733223E-16,0.));
#7442=DIRECTION('',(0.,1.,0.));
#7443=DIRECTION('center_axis',(0.,0.,-1.));
#7444=DIRECTION('ref_axis',(-0.0422331972043614,0.99910778049913,0.));
#7445=DIRECTION('',(-1.,0.,0.));
#7446=DIRECTION('',(-0.666311116601944,-0.745673853566471,0.));
#7447=DIRECTION('center_axis',(0.,0.,-1.));
#7448=DIRECTION('ref_axis',(-1.,0.,0.));
#7449=DIRECTION('',(0.,-1.,0.));
#7450=DIRECTION('',(-1.,-1.96383789733223E-16,0.));
#7451=DIRECTION('',(0.,1.,0.));
#7452=DIRECTION('',(0.666311116601944,0.745673853566471,0.));
#7453=DIRECTION('',(1.,0.,0.));
#7454=DIRECTION('center_axis',(0.,0.,1.));
#7455=DIRECTION('ref_axis',(0.0422331972609955,-0.999107780496736,0.));
#7456=DIRECTION('center_axis',(0.,-1.,0.));
#7457=DIRECTION('ref_axis',(0.,0.,-1.));
#7458=DIRECTION('',(0.,0.,-1.));
#7459=DIRECTION('',(1.,0.,0.));
#7460=DIRECTION('center_axis',(0.,-1.,0.));
#7461=DIRECTION('ref_axis',(0.,0.,-1.));
#7462=DIRECTION('',(-1.,0.,0.));
#7463=DIRECTION('center_axis',(0.,0.,-1.));
#7464=DIRECTION('ref_axis',(-1.,0.,0.));
#7465=DIRECTION('',(0.,0.,-1.));
#7466=DIRECTION('center_axis',(0.,0.,-1.));
#7467=DIRECTION('ref_axis',(-1.,0.,0.));
#7468=DIRECTION('center_axis',(0.,0.,1.));
#7469=DIRECTION('ref_axis',(1.,0.,0.));
#7470=DIRECTION('center_axis',(0.745673853566471,-0.666311116601944,0.));
#7471=DIRECTION('ref_axis',(0.666311116601944,0.745673853566471,0.));
#7472=DIRECTION('',(0.,0.,-1.));
#7473=DIRECTION('',(0.666311116601944,0.745673853566471,0.));
#7474=DIRECTION('',(-0.666311116601944,-0.745673853566471,0.));
#7475=DIRECTION('center_axis',(0.,0.,-1.));
#7476=DIRECTION('ref_axis',(-1.,0.,0.));
#7477=DIRECTION('',(0.,0.,-1.));
#7478=DIRECTION('center_axis',(0.,0.,-1.));
#7479=DIRECTION('ref_axis',(-1.,0.,0.));
#7480=DIRECTION('center_axis',(0.,0.,1.));
#7481=DIRECTION('ref_axis',(-1.,-1.04083408558608E-15,0.));
#7482=DIRECTION('center_axis',(1.,0.,0.));
#7483=DIRECTION('ref_axis',(0.,0.,-1.));
#7484=DIRECTION('',(0.,-1.,0.));
#7485=DIRECTION('',(0.,0.,1.));
#7486=DIRECTION('',(0.,1.,0.));
#7487=DIRECTION('center_axis',(-1.96383789733223E-16,1.,0.));
#7488=DIRECTION('ref_axis',(-1.,-1.96383789733223E-16,0.));
#7489=DIRECTION('center_axis',(-1.96383789733223E-16,1.,0.));
#7490=DIRECTION('ref_axis',(-1.,-1.96383789733223E-16,0.));
#7491=DIRECTION('',(-1.,-1.96383789733223E-16,0.));
#7492=DIRECTION('center_axis',(1.96383789733223E-16,-1.,0.));
#7493=DIRECTION('ref_axis',(-1.,-1.96383789733223E-16,0.));
#7494=DIRECTION('',(0.,0.,-1.));
#7495=DIRECTION('center_axis',(1.96383789733223E-16,-1.,0.));
#7496=DIRECTION('ref_axis',(-1.,-1.96383789733223E-16,0.));
#7497=DIRECTION('',(1.,1.96383789733223E-16,0.));
#7498=DIRECTION('center_axis',(-1.96383789733223E-16,1.,0.));
#7499=DIRECTION('ref_axis',(-1.,-1.96383789733223E-16,0.));
#7500=DIRECTION('center_axis',(-0.866025403784443,0.,0.499999999999992));
#7501=DIRECTION('ref_axis',(0.499999999999992,0.,0.866025403784443));
#7502=DIRECTION('',(0.,-1.,0.));
#7503=DIRECTION('',(-0.499999999999992,1.96383789733223E-16,-0.866025403784443));
#7504=DIRECTION('',(0.,1.,0.));
#7505=DIRECTION('center_axis',(-0.86602540378444,6.35182550169207E-14,0.499999999999998));
#7506=DIRECTION('ref_axis',(-0.0211165986195528,-0.999107780497666,-0.0365750216919776));
#7507=DIRECTION('',(0.499999999999992,0.,0.866025403784443));
#7508=DIRECTION('',(0.333155558300967,-0.745673853566471,0.577042353801262));
#7509=DIRECTION('center_axis',(0.,-1.,0.));
#7510=DIRECTION('ref_axis',(-0.866025403784443,0.,0.499999999999992));
#7511=DIRECTION('',(-0.866025403784443,0.,0.499999999999992));
#7512=DIRECTION('',(-0.499999999999992,0.,-0.866025403784443));
#7513=DIRECTION('center_axis',(0.,-1.,0.));
#7514=DIRECTION('ref_axis',(0.,0.,-1.));
#7515=DIRECTION('',(0.499999999999992,0.,0.866025403784443));
#7516=DIRECTION('center_axis',(-0.866025403784443,0.,0.499999999999992));
#7517=DIRECTION('ref_axis',(0.499999999999992,0.,0.866025403784443));
#7518=DIRECTION('center_axis',(0.866025403784444,0.,-0.499999999999991));
#7519=DIRECTION('ref_axis',(-0.499999999999991,0.,-0.866025403784444));
#7520=DIRECTION('',(-0.866025403784443,0.,0.499999999999992));
#7521=DIRECTION('center_axis',(-0.866025403784443,5.78241158658927E-16,
0.499999999999992));
#7522=DIRECTION('ref_axis',(0.499999999999992,-2.45729362005254E-31,0.866025403784443));
#7523=DIRECTION('center_axis',(-0.372836926783229,-0.666311116601944,-0.645772500126405));
#7524=DIRECTION('ref_axis',(-0.333155558300967,0.745673853566471,-0.577042353801262));
#7525=DIRECTION('',(-0.866025403784443,0.,0.499999999999992));
#7526=DIRECTION('',(-0.333155558300967,0.745673853566471,-0.577042353801262));
#7527=DIRECTION('center_axis',(-0.866025403784443,0.,0.499999999999992));
#7528=DIRECTION('ref_axis',(0.499999999999992,0.,0.866025403784443));
#7529=DIRECTION('center_axis',(0.866025403784443,0.,-0.499999999999992));
#7530=DIRECTION('ref_axis',(0.499999999999992,-2.77555756156289E-15,0.866025403784443));
#7531=DIRECTION('',(-0.866025403784443,0.,0.499999999999992));
#7532=DIRECTION('center_axis',(-0.866025403784443,0.,0.499999999999992));
#7533=DIRECTION('ref_axis',(0.499999999999992,0.,0.866025403784443));
#7534=DIRECTION('center_axis',(-0.499999999999992,0.,-0.866025403784443));
#7535=DIRECTION('ref_axis',(-0.866025403784443,0.,0.499999999999992));
#7536=DIRECTION('',(0.866025403784443,-1.23259516440783E-32,-0.499999999999992));
#7537=DIRECTION('',(0.,1.,0.));
#7538=DIRECTION('center_axis',(9.81918948666102E-17,1.,1.70073350800434E-16));
#7539=DIRECTION('ref_axis',(0.499999999999992,-1.96383789733223E-16,0.866025403784443));
#7540=DIRECTION('center_axis',(9.81918948666102E-17,1.,1.70073350800434E-16));
#7541=DIRECTION('ref_axis',(-1.66998245814083E-32,-1.70073350800434E-16,
1.));
#7542=DIRECTION('',(0.499999999999992,-1.96383789733223E-16,0.866025403784443));
#7543=DIRECTION('center_axis',(-9.81918948666102E-17,-1.,-1.70073350800434E-16));
#7544=DIRECTION('ref_axis',(-1.66998245814083E-32,-1.70073350800434E-16,
1.));
#7545=DIRECTION('',(-0.866025403784443,1.23259516440783E-32,0.499999999999992));
#7546=DIRECTION('',(-0.499999999999992,1.96383789733223E-16,-0.866025403784443));
#7547=DIRECTION('center_axis',(9.81918948666102E-17,1.,1.70073350800434E-16));
#7548=DIRECTION('ref_axis',(-1.66998245814083E-32,-1.70073350800434E-16,
1.));
#7549=DIRECTION('center_axis',(-0.866025403784443,0.,0.499999999999992));
#7550=DIRECTION('ref_axis',(0.499999999999992,0.,0.866025403784443));
#7551=DIRECTION('',(0.,-1.,0.));
#7552=DIRECTION('',(0.499999999999992,-1.96383789733223E-16,0.866025403784443));
#7553=DIRECTION('',(-0.499999999999992,0.,-0.866025403784443));
#7554=DIRECTION('center_axis',(0.866025403784441,-2.51426426109907E-14,
-0.499999999999997));
#7555=DIRECTION('ref_axis',(0.021116598590189,0.999107780500145,0.0365750216411948));
#7556=DIRECTION('center_axis',(0.866025403784436,0.,0.500000000000004));
#7557=DIRECTION('ref_axis',(0.500000000000004,0.,-0.866025403784436));
#7558=DIRECTION('',(-0.500000000000004,1.96383789733224E-16,0.866025403784436));
#7559=DIRECTION('',(0.,1.,0.));
#7560=DIRECTION('center_axis',(0.866025403784437,-2.51426426109492E-14,
0.500000000000004));
#7561=DIRECTION('ref_axis',(-0.0211165986015709,-0.999107780499183,0.0365750216609081));
#7562=DIRECTION('',(0.500000000000004,0.,-0.866025403784436));
#7563=DIRECTION('center_axis',(0.,-1.,0.));
#7564=DIRECTION('ref_axis',(0.866025403784436,0.,0.500000000000004));
#7565=DIRECTION('',(0.866025403784436,0.,0.500000000000004));
#7566=DIRECTION('',(-0.500000000000004,0.,0.866025403784436));
#7567=DIRECTION('',(0.500000000000004,0.,-0.866025403784436));
#7568=DIRECTION('center_axis',(0.866025403784436,0.,0.500000000000004));
#7569=DIRECTION('ref_axis',(0.500000000000004,0.,-0.866025403784436));
#7570=DIRECTION('center_axis',(-0.866025403784434,0.,-0.500000000000008));
#7571=DIRECTION('ref_axis',(-0.500000000000008,0.,0.866025403784434));
#7572=DIRECTION('',(0.866025403784436,0.,0.500000000000004));
#7573=DIRECTION('center_axis',(0.866025403784436,-6.55710784405496E-16,
0.500000000000004));
#7574=DIRECTION('ref_axis',(0.500000000000004,1.88743283563644E-31,-0.866025403784436));
#7575=DIRECTION('center_axis',(-0.372836926783238,-0.666311116601944,0.6457725001264));
#7576=DIRECTION('ref_axis',(-0.333155558300975,0.745673853566471,0.577042353801257));
#7577=DIRECTION('',(0.333155558300975,-0.745673853566471,-0.577042353801257));
#7578=DIRECTION('',(0.866025403784436,0.,0.500000000000004));
#7579=DIRECTION('center_axis',(0.866025403784436,0.,0.500000000000004));
#7580=DIRECTION('ref_axis',(0.500000000000004,0.,-0.866025403784436));
#7581=DIRECTION('center_axis',(-0.866025403784436,0.,-0.500000000000004));
#7582=DIRECTION('ref_axis',(0.500000000000004,0.,-0.866025403784436));
#7583=DIRECTION('',(0.866025403784436,0.,0.500000000000004));
#7584=DIRECTION('center_axis',(0.866025403784436,0.,0.500000000000004));
#7585=DIRECTION('ref_axis',(0.500000000000004,0.,-0.866025403784436));
#7586=DIRECTION('center_axis',(-0.500000000000004,0.,0.866025403784436));
#7587=DIRECTION('ref_axis',(0.866025403784436,0.,0.500000000000004));
#7588=DIRECTION('',(0.,-1.,0.));
#7589=DIRECTION('',(-0.866025403784436,-1.23259516440783E-32,-0.500000000000004));
#7590=DIRECTION('center_axis',(9.81918948666125E-17,1.,-1.70073350800433E-16));
#7591=DIRECTION('ref_axis',(0.500000000000004,-1.96383789733223E-16,-0.866025403784436));
#7592=DIRECTION('center_axis',(9.81918948666125E-17,1.,-1.70073350800433E-16));
#7593=DIRECTION('ref_axis',(-7.25831191047587E-34,1.70073350800433E-16,
1.));
#7594=DIRECTION('center_axis',(9.81918948666125E-17,1.,-1.70073350800433E-16));
#7595=DIRECTION('ref_axis',(1.66998245814086E-32,1.70073350800433E-16,1.));
#7596=DIRECTION('',(0.500000000000004,-1.96383789733224E-16,-0.866025403784436));
#7597=DIRECTION('center_axis',(-9.81918948666125E-17,-1.,1.70073350800433E-16));
#7598=DIRECTION('ref_axis',(1.66998245814086E-32,1.70073350800433E-16,1.));
#7599=DIRECTION('',(0.866025403784436,1.23259516440783E-32,0.500000000000004));
#7600=DIRECTION('center_axis',(-9.81918948666125E-17,-1.,1.70073350800433E-16));
#7601=DIRECTION('ref_axis',(1.73472347597681E-15,1.70073350800433E-16,1.));
#7602=DIRECTION('',(-0.500000000000004,1.96383789733224E-16,0.866025403784436));
#7603=DIRECTION('center_axis',(9.81918948666125E-17,1.,-1.70073350800433E-16));
#7604=DIRECTION('ref_axis',(1.66998245814086E-32,1.70073350800433E-16,1.));
#7605=DIRECTION('center_axis',(0.866025403784436,0.,0.500000000000004));
#7606=DIRECTION('ref_axis',(0.500000000000004,0.,-0.866025403784436));
#7607=DIRECTION('',(0.,-1.,0.));
#7608=DIRECTION('',(0.500000000000004,-1.96383789733224E-16,-0.866025403784436));
#7609=DIRECTION('',(0.,1.,0.));
#7610=DIRECTION('',(-0.333155558300975,0.745673853566471,0.577042353801257));
#7611=DIRECTION('',(-0.500000000000004,0.,0.866025403784436));
#7612=DIRECTION('center_axis',(-0.866025403784436,-2.24960486516661E-14,
-0.500000000000004));
#7613=DIRECTION('ref_axis',(0.0211165986566772,0.999107780494521,-0.0365750217564501));
#7614=DIRECTION('center_axis',(0.,-1.,0.));
#7615=DIRECTION('ref_axis',(0.,0.,-1.));
#7616=DIRECTION('center_axis',(1.96383789733223E-16,-1.,0.));
#7617=DIRECTION('ref_axis',(-1.,-1.96383789733223E-16,6.01006558606138E-15));
#7618=DIRECTION('center_axis',(0.,-1.,0.));
#7619=DIRECTION('ref_axis',(0.,0.,-1.));
#7620=DIRECTION('center_axis',(-9.81918948666125E-17,-1.,1.70073350800433E-16));
#7621=DIRECTION('ref_axis',(2.48598167423448E-14,1.7007335080043E-16,1.));
#7622=DIRECTION('center_axis',(0.,-1.,0.));
#7623=DIRECTION('ref_axis',(0.,0.,-1.));
#7624=DIRECTION('center_axis',(-9.81918948666125E-17,-1.,1.70073350800433E-16));
#7625=DIRECTION('ref_axis',(-1.63910879619856E-15,1.70073350800433E-16,
1.));
#7626=DIRECTION('center_axis',(0.,-1.,0.));
#7627=DIRECTION('ref_axis',(0.,0.,-1.));
#7628=DIRECTION('center_axis',(-9.81918948666102E-17,-1.,-1.70073350800434E-16));
#7629=DIRECTION('ref_axis',(-1.66998245814083E-32,-1.70073350800434E-16,
1.));
#7630=DIRECTION('center_axis',(0.,-1.,0.));
#7631=DIRECTION('ref_axis',(0.,0.,-1.));
#7632=DIRECTION('center_axis',(-9.81918948666102E-17,-1.,-1.70073350800434E-16));
#7633=DIRECTION('ref_axis',(-1.06542071752906E-14,-1.70073350800433E-16,
1.));
#7634=DIRECTION('center_axis',(0.,-1.,0.));
#7635=DIRECTION('ref_axis',(0.,0.,-1.));
#7636=DIRECTION('center_axis',(1.96383789733223E-16,-1.,0.));
#7637=DIRECTION('ref_axis',(-1.,-1.96383789733223E-16,-1.63910879619856E-15));
#7638=DIRECTION('center_axis',(9.81918948666125E-17,1.,-1.70073350800433E-16));
#7639=DIRECTION('ref_axis',(0.500000000000005,-1.77192702184564E-16,-0.866025403784436));
#7640=DIRECTION('center_axis',(0.,-1.,0.));
#7641=DIRECTION('ref_axis',(0.499999999999993,0.,0.866025403784443));
#7642=DIRECTION('center_axis',(0.,-1.,0.));
#7643=DIRECTION('ref_axis',(0.,0.,-1.));
#7644=DIRECTION('center_axis',(0.,-1.,0.));
#7645=DIRECTION('ref_axis',(0.,0.,-1.));
#7646=DIRECTION('center_axis',(0.,1.,0.));
#7647=DIRECTION('ref_axis',(0.,0.,1.));
#7648=DIRECTION('',(0.5,0.,-0.866025403784439));
#7649=DIRECTION('center_axis',(0.,-1.,0.));
#7650=DIRECTION('ref_axis',(1.73472347597681E-15,0.,1.));
#7651=DIRECTION('',(1.,0.,0.));
#7652=DIRECTION('center_axis',(0.,-1.,0.));
#7653=DIRECTION('ref_axis',(2.60208521396521E-15,0.,1.));
#7654=DIRECTION('',(0.5,0.,0.866025403784439));
#7655=DIRECTION('center_axis',(0.,-1.,0.));
#7656=DIRECTION('ref_axis',(1.73472347597681E-15,0.,1.));
#7657=DIRECTION('',(-0.5,0.,0.866025403784439));
#7658=DIRECTION('center_axis',(0.,-1.,0.));
#7659=DIRECTION('ref_axis',(-3.46944695195362E-15,0.,1.));
#7660=DIRECTION('',(-1.,0.,-1.36592399683213E-16));
#7661=DIRECTION('center_axis',(0.,-1.,0.));
#7662=DIRECTION('ref_axis',(0.,0.,1.));
#7663=DIRECTION('',(-0.5,0.,-0.866025403784439));
#7664=DIRECTION('center_axis',(0.,-1.,0.));
#7665=DIRECTION('ref_axis',(0.,0.,1.));
#7666=DIRECTION('center_axis',(0.,-1.,0.));
#7667=DIRECTION('ref_axis',(0.,0.,1.));
#7668=DIRECTION('center_axis',(0.,-1.,0.));
#7669=DIRECTION('ref_axis',(0.,0.,1.));
#7670=DIRECTION('center_axis',(0.,-1.,0.));
#7671=DIRECTION('ref_axis',(0.,0.,1.));
#7672=DIRECTION('center_axis',(0.,-1.,0.));
#7673=DIRECTION('ref_axis',(0.,0.,1.));
#7674=DIRECTION('center_axis',(0.,-1.,0.));
#7675=DIRECTION('ref_axis',(0.,0.,1.));
#7676=DIRECTION('center_axis',(0.,-1.,0.));
#7677=DIRECTION('ref_axis',(0.,0.,1.));
#7678=DIRECTION('center_axis',(0.,1.,0.));
#7679=DIRECTION('ref_axis',(0.,0.,1.));
#7680=DIRECTION('center_axis',(0.,1.,0.));
#7681=DIRECTION('ref_axis',(0.,0.,1.));
#7682=DIRECTION('center_axis',(0.,1.,0.));
#7683=DIRECTION('ref_axis',(0.,0.,1.));
#7684=DIRECTION('center_axis',(0.,1.,0.));
#7685=DIRECTION('ref_axis',(0.,0.,1.));
#7686=DIRECTION('center_axis',(0.,1.,0.));
#7687=DIRECTION('ref_axis',(0.,0.,1.));
#7688=DIRECTION('center_axis',(0.,1.,0.));
#7689=DIRECTION('ref_axis',(0.,0.,1.));
#7690=DIRECTION('center_axis',(0.,1.,0.));
#7691=DIRECTION('ref_axis',(0.,0.,1.));
#7692=DIRECTION('center_axis',(0.,1.,0.));
#7693=DIRECTION('ref_axis',(0.,0.,1.));
#7694=DIRECTION('center_axis',(0.,1.,0.));
#7695=DIRECTION('ref_axis',(0.,0.,1.));
#7696=DIRECTION('center_axis',(0.,1.,0.));
#7697=DIRECTION('ref_axis',(0.,0.,1.));
#7698=DIRECTION('center_axis',(0.,1.,0.));
#7699=DIRECTION('ref_axis',(0.,0.,1.));
#7700=DIRECTION('center_axis',(0.,1.,0.));
#7701=DIRECTION('ref_axis',(0.,0.,1.));
#7702=DIRECTION('center_axis',(0.,1.,0.));
#7703=DIRECTION('ref_axis',(0.,0.,1.));
#7704=DIRECTION('center_axis',(-0.499999999999999,1.93599546773136E-15,
0.866025403784439));
#7705=DIRECTION('ref_axis',(0.866025403784439,9.70515073617369E-31,0.499999999999999));
#7706=DIRECTION('center_axis',(1.,0.,0.));
#7707=DIRECTION('ref_axis',(0.,0.,-1.));
#7708=DIRECTION('center_axis',(-1.,0.,-1.36592399683213E-16));
#7709=DIRECTION('ref_axis',(-1.36592399683213E-16,0.,1.));
#7710=DIRECTION('center_axis',(1.,0.,0.));
#7711=DIRECTION('ref_axis',(0.,0.,-1.));
#7712=DIRECTION('center_axis',(-0.5,0.,0.866025403784439));
#7713=DIRECTION('ref_axis',(0.866025403784439,0.,0.5));
#7714=DIRECTION('center_axis',(-0.5,2.29809145050324E-15,0.866025403784439));
#7715=DIRECTION('ref_axis',(0.866025403784439,6.9389298859906E-31,0.5));
#7716=DIRECTION('center_axis',(0.,1.,0.));
#7717=DIRECTION('ref_axis',(0.,0.,1.));
#7718=DIRECTION('center_axis',(0.5,0.,0.866025403784438));
#7719=DIRECTION('ref_axis',(0.866025403784438,0.,-0.5));
#7720=DIRECTION('center_axis',(0.,1.,0.));
#7721=DIRECTION('ref_axis',(0.,0.,1.));
#7722=DIRECTION('center_axis',(0.5,0.,0.866025403784439));
#7723=DIRECTION('ref_axis',(0.866025403784439,0.,-0.5));
#7724=DIRECTION('center_axis',(-0.5,0.,-0.866025403784439));
#7725=DIRECTION('ref_axis',(-0.866025403784439,0.,0.5));
#7726=DIRECTION('center_axis',(0.5,0.,0.866025403784439));
#7727=DIRECTION('ref_axis',(0.866025403784439,0.,-0.5));
#7728=DIRECTION('center_axis',(0.5,0.,0.866025403784439));
#7729=DIRECTION('ref_axis',(0.866025403784439,0.,-0.5));
#7730=DIRECTION('center_axis',(0.5,4.33680868994203E-16,0.866025403784438));
#7731=DIRECTION('ref_axis',(0.866025403784438,5.77289724224632E-33,-0.5));
#7732=DIRECTION('center_axis',(0.,1.,0.));
#7733=DIRECTION('ref_axis',(0.,0.,1.));
#7734=DIRECTION('center_axis',(-0.5,0.,0.866025403784439));
#7735=DIRECTION('ref_axis',(0.866025403784439,0.,0.5));
#7736=DIRECTION('center_axis',(0.,1.,0.));
#7737=DIRECTION('ref_axis',(0.,0.,1.));
#7738=DIRECTION('center_axis',(1.,0.,0.));
#7739=DIRECTION('ref_axis',(0.,0.,-1.));
#7740=DIRECTION('center_axis',(0.5,0.,-0.866025403784439));
#7741=DIRECTION('ref_axis',(-0.866025403784439,0.,-0.5));
#7742=DIRECTION('center_axis',(-0.5,0.,0.866025403784439));
#7743=DIRECTION('ref_axis',(0.866025403784439,0.,0.5));
#7744=DIRECTION('center_axis',(1.,0.,0.));
#7745=DIRECTION('ref_axis',(0.,0.,-1.));
#7746=DIRECTION('center_axis',(1.,0.,0.));
#7747=DIRECTION('ref_axis',(0.,0.,-1.));
#7748=DIRECTION('center_axis',(0.,1.,0.));
#7749=DIRECTION('ref_axis',(0.,0.,1.));
#7750=DIRECTION('center_axis',(0.,-1.,0.));
#7751=DIRECTION('ref_axis',(0.,0.,-1.));
#7752=DIRECTION('center_axis',(-1.96383789733223E-16,1.,0.));
#7753=DIRECTION('ref_axis',(-1.,-1.96383789733223E-16,0.));
#7754=DIRECTION('center_axis',(0.,1.,0.));
#7755=DIRECTION('ref_axis',(0.,0.,1.));
#7756=DIRECTION('center_axis',(0.,1.,0.));
#7757=DIRECTION('ref_axis',(-1.,0.,0.));
#7758=DIRECTION('center_axis',(0.666311116601944,0.745673853566471,0.));
#7759=DIRECTION('ref_axis',(-0.745673853566471,0.666311116601944,0.));
#7760=DIRECTION('center_axis',(-0.666311116601944,-0.745673853566471,0.));
#7761=DIRECTION('ref_axis',(0.745673853566471,-0.666311116601944,0.));
#7762=DIRECTION('center_axis',(-1.,0.,0.));
#7763=DIRECTION('ref_axis',(0.,0.,1.));
#7764=DIRECTION('center_axis',(1.,0.,0.));
#7765=DIRECTION('ref_axis',(0.,0.,-1.));
#7766=DIRECTION('center_axis',(0.984161952974649,0.177271685040576,2.82385335648104E-15));
#7767=DIRECTION('ref_axis',(-0.177271685040576,0.984161952974649,-4.640930146752E-31));
#7768=DIRECTION('center_axis',(0.,1.,0.));
#7769=DIRECTION('ref_axis',(0.,0.,1.));
#7770=DIRECTION('center_axis',(-1.96383789733223E-16,1.,0.));
#7771=DIRECTION('ref_axis',(-1.,-1.96383789733223E-16,0.));
#7772=DIRECTION('center_axis',(0.,1.,0.));
#7773=DIRECTION('ref_axis',(0.,0.,1.));
#7774=DIRECTION('center_axis',(0.,1.,0.));
#7775=DIRECTION('ref_axis',(-1.,0.,0.));
#7776=DIRECTION('center_axis',(0.666311116601944,0.745673853566471,0.));
#7777=DIRECTION('ref_axis',(-0.745673853566471,0.666311116601944,0.));
#7778=DIRECTION('center_axis',(0.666311116601944,0.745673853566471,0.));
#7779=DIRECTION('ref_axis',(-0.745673853566471,0.666311116601944,0.));
#7780=DIRECTION('center_axis',(1.,0.,0.));
#7781=DIRECTION('ref_axis',(0.,0.,-1.));
#7782=DIRECTION('center_axis',(1.,0.,0.));
#7783=DIRECTION('ref_axis',(0.,0.,-1.));
#7784=DIRECTION('center_axis',(0.984161952974649,0.177271685040574,0.));
#7785=DIRECTION('ref_axis',(-0.177271685040574,0.984161952974649,0.));
#7786=DIRECTION('center_axis',(0.,1.,0.));
#7787=DIRECTION('ref_axis',(0.,0.,1.));
#7788=DIRECTION('center_axis',(9.81918948666125E-17,1.,-1.70073350800433E-16));
#7789=DIRECTION('ref_axis',(1.66998245814086E-32,1.70073350800433E-16,1.));
#7790=DIRECTION('center_axis',(0.,1.,0.));
#7791=DIRECTION('ref_axis',(0.,0.,1.));
#7792=DIRECTION('center_axis',(0.,1.,0.));
#7793=DIRECTION('ref_axis',(0.500000000000005,0.,-0.866025403784436));
#7794=DIRECTION('center_axis',(-0.333155558300976,0.74567385356647,0.577042353801258));
#7795=DIRECTION('ref_axis',(-8.34044259913248E-17,-0.612005054639085,0.790853850655234));
#7796=DIRECTION('center_axis',(-0.333155558300975,0.745673853566471,0.577042353801257));
#7797=DIRECTION('ref_axis',(7.49624866032534E-17,-0.612005054639084,0.790853850655234));
#7798=DIRECTION('center_axis',(-0.500000000000004,0.,0.866025403784436));
#7799=DIRECTION('ref_axis',(0.866025403784436,0.,0.500000000000004));
#7800=DIRECTION('center_axis',(-0.500000000000004,-9.29635508958665E-17,
0.866025403784436));
#7801=DIRECTION('ref_axis',(0.866025403784436,2.67365344803013E-32,0.500000000000004));
#7802=DIRECTION('center_axis',(-0.492080976487329,0.177271685040574,0.85230925271415));
#7803=DIRECTION('ref_axis',(0.866025403784436,9.07442760845917E-18,0.500000000000004));
#7804=DIRECTION('center_axis',(0.492080976487328,-0.177271685040574,-0.85230925271415));
#7805=DIRECTION('ref_axis',(-0.866025403784436,1.51531198058906E-18,-0.500000000000004));
#7806=DIRECTION('center_axis',(0.500000000000004,-4.33680868994205E-16,
-0.866025403784436));
#7807=DIRECTION('ref_axis',(-0.866025403784436,-4.66515379724155E-32,-0.500000000000004));
#7808=DIRECTION('center_axis',(0.500000000000004,0.,-0.866025403784436));
#7809=DIRECTION('ref_axis',(-0.866025403784436,0.,-0.500000000000004));
#7810=DIRECTION('center_axis',(0.,1.,0.));
#7811=DIRECTION('ref_axis',(0.500000000000004,0.,-0.866025403784436));
#7812=DIRECTION('center_axis',(0.,1.,0.));
#7813=DIRECTION('ref_axis',(0.499999999999993,0.,0.866025403784443));
#7814=DIRECTION('center_axis',(-0.499999999999992,0.,-0.866025403784443));
#7815=DIRECTION('ref_axis',(-0.866025403784443,0.,0.499999999999992));
#7816=DIRECTION('center_axis',(-0.499999999999992,3.46944695195356E-16,
-0.866025403784443));
#7817=DIRECTION('ref_axis',(-0.866025403784443,3.51994154947752E-32,0.499999999999992));
#7818=DIRECTION('center_axis',(-0.492080976487317,0.177271685040573,-0.852309252714157));
#7819=DIRECTION('ref_axis',(-0.866025403784443,6.20279384261769E-18,0.499999999999992));
#7820=DIRECTION('center_axis',(0.492080976487317,-0.177271685040574,0.852309252714157));
#7821=DIRECTION('ref_axis',(0.866025403784443,8.18616803104063E-18,-0.499999999999992));
#7822=DIRECTION('center_axis',(0.499999999999992,3.00462919747434E-16,0.866025403784443));
#7823=DIRECTION('ref_axis',(0.866025403784443,-2.69630192211791E-33,-0.499999999999992));
#7824=DIRECTION('center_axis',(0.499999999999992,0.,0.866025403784443));
#7825=DIRECTION('ref_axis',(0.866025403784443,0.,-0.499999999999992));
#7826=DIRECTION('center_axis',(0.333155558300967,-0.745673853566471,0.577042353801262));
#7827=DIRECTION('ref_axis',(2.59234872084442E-17,-0.612005054639087,-0.790853850655232));
#7828=DIRECTION('center_axis',(0.333155558300966,-0.745673853566471,0.577042353801261));
#7829=DIRECTION('ref_axis',(-1.20939466035638E-17,-0.612005054639087,-0.790853850655232));
#7830=DIRECTION('center_axis',(0.,1.,0.));
#7831=DIRECTION('ref_axis',(0.499999999999991,0.,0.866025403784444));
#7832=DIRECTION('center_axis',(0.,-1.,0.));
#7833=DIRECTION('ref_axis',(0.,0.,-1.));
#7834=DIRECTION('center_axis',(0.,-1.,0.));
#7835=DIRECTION('ref_axis',(0.,0.,-1.));
#7836=DIRECTION('center_axis',(9.81918948666102E-17,1.,1.70073350800434E-16));
#7837=DIRECTION('ref_axis',(-1.66998245814083E-32,-1.70073350800434E-16,
1.));
#7838=DIRECTION('center_axis',(-0.986265445452608,8.54626199733501E-15,
-0.165168008724958));
#7839=DIRECTION('ref_axis',(-0.165168008724958,-6.85891870706028E-33,0.986265445452608));
#7840=DIRECTION('center_axis',(-1.96383789733223E-16,1.,0.));
#7841=DIRECTION('ref_axis',(-1.,0.,0.));
#7842=DIRECTION('center_axis',(-1.,0.,0.));
#7843=DIRECTION('ref_axis',(0.,0.,1.));
#7844=DIRECTION('center_axis',(1.,1.96383789733223E-16,0.));
#7845=DIRECTION('ref_axis',(-1.96383789733223E-16,1.,0.));
#7846=DIRECTION('center_axis',(-1.,0.,0.));
#7847=DIRECTION('ref_axis',(0.,0.,1.));
#7848=DIRECTION('center_axis',(-1.96383789733223E-16,1.,0.));
#7849=DIRECTION('ref_axis',(-1.,0.,0.));
#7850=DIRECTION('center_axis',(0.,0.,-1.));
#7851=DIRECTION('ref_axis',(-1.,0.,0.));
#7852=DIRECTION('center_axis',(0.,0.,-1.));
#7853=DIRECTION('ref_axis',(-1.,0.,0.));
#7854=DIRECTION('center_axis',(0.,0.,-1.));
#7855=DIRECTION('ref_axis',(-1.,0.,0.));
#7856=DIRECTION('center_axis',(-1.96383789733223E-16,1.,0.));
#7857=DIRECTION('ref_axis',(-1.,0.,0.));
#7858=DIRECTION('center_axis',(1.,0.,0.));
#7859=DIRECTION('ref_axis',(0.,0.,-1.));
#7860=DIRECTION('center_axis',(-1.,-1.96383789733223E-16,0.));
#7861=DIRECTION('ref_axis',(1.96383789733223E-16,-1.,0.));
#7862=DIRECTION('center_axis',(1.,0.,0.));
#7863=DIRECTION('ref_axis',(0.,0.,-1.));
#7864=DIRECTION('center_axis',(-1.96383789733223E-16,1.,0.));
#7865=DIRECTION('ref_axis',(-1.,0.,0.));
#7866=DIRECTION('center_axis',(0.986265445452611,0.,-0.165168008724946));
#7867=DIRECTION('ref_axis',(-0.165168008724946,0.,-0.98626544545261));
#7868=DIRECTION('center_axis',(0.350093031278016,8.12470694020607E-16,-0.936714934999208));
#7869=DIRECTION('ref_axis',(-0.936714934999208,-6.70893457146978E-32,-0.350093031278016));
#7870=DIRECTION('center_axis',(9.81918948666125E-17,1.,-1.70073350800433E-16));
#7871=DIRECTION('ref_axis',(0.,0.,1.));
#7872=DIRECTION('center_axis',(0.500000000000005,-1.50231459873715E-15,
-0.866025403784436));
#7873=DIRECTION('ref_axis',(-0.866025403784435,2.19556013660713E-32,-0.500000000000005));
#7874=DIRECTION('center_axis',(0.500000000000004,-1.96383789733224E-16,
-0.866025403784436));
#7875=DIRECTION('ref_axis',(-0.866025403784436,1.62736006015126E-32,-0.500000000000004));
#7876=DIRECTION('center_axis',(0.500000000000007,0.,-0.866025403784435));
#7877=DIRECTION('ref_axis',(-0.866025403784435,0.,-0.500000000000007));
#7878=DIRECTION('center_axis',(9.81918948666125E-17,1.,-1.70073350800433E-16));
#7879=DIRECTION('ref_axis',(0.,0.,1.));
#7880=DIRECTION('center_axis',(-0.866025403784438,-3.46944695195362E-15,
-0.500000000000002));
#7881=DIRECTION('ref_axis',(-0.500000000000001,3.32427446512172E-33,0.866025403784438));
#7882=DIRECTION('center_axis',(0.866025403784436,1.23259516440783E-32,0.500000000000004));
#7883=DIRECTION('ref_axis',(0.500000000000004,-2.42099675731877E-49,-0.866025403784436));
#7884=DIRECTION('center_axis',(-0.866025403784436,-4.64817754479332E-16,
-0.500000000000004));
#7885=DIRECTION('ref_axis',(-0.500000000000004,5.15704192091073E-32,0.866025403784436));
#7886=DIRECTION('center_axis',(9.81918948666125E-17,1.,-1.70073350800433E-16));
#7887=DIRECTION('ref_axis',(-0.258819045102516,0.,-0.96592582628907));
#7888=DIRECTION('center_axis',(-0.500000000000007,8.67361737988414E-16,
0.866025403784435));
#7889=DIRECTION('ref_axis',(0.866025403784435,-6.81437383295693E-31,0.500000000000007));
#7890=DIRECTION('center_axis',(-0.500000000000004,1.96383789733224E-16,
0.866025403784436));
#7891=DIRECTION('ref_axis',(0.866025403784436,-5.83267376229116E-31,0.500000000000004));
#7892=DIRECTION('center_axis',(-0.500000000000004,0.,0.866025403784436));
#7893=DIRECTION('ref_axis',(0.866025403784436,0.,0.500000000000004));
#7894=DIRECTION('center_axis',(9.81918948666125E-17,1.,-1.70073350800433E-16));
#7895=DIRECTION('ref_axis',(0.,0.,1.));
#7896=DIRECTION('center_axis',(-0.636172414174605,5.51791610818759E-16,
0.771546926274258));
#7897=DIRECTION('ref_axis',(0.771546926274258,-2.75521141229581E-31,0.636172414174605));
#7898=DIRECTION('center_axis',(0.636172414174592,2.75895805409376E-16,0.771546926274269));
#7899=DIRECTION('ref_axis',(0.771546926274269,-8.00143989047643E-32,-0.636172414174592));
#7900=DIRECTION('center_axis',(9.81918948666102E-17,1.,1.70073350800434E-16));
#7901=DIRECTION('ref_axis',(0.,0.,1.));
#7902=DIRECTION('center_axis',(0.49999999999999,-2.78778876297724E-15,0.866025403784444));
#7903=DIRECTION('ref_axis',(0.866025403784444,1.07195328581195E-30,-0.49999999999999));
#7904=DIRECTION('center_axis',(0.499999999999992,-1.96383789733223E-16,
0.866025403784443));
#7905=DIRECTION('ref_axis',(0.866025403784443,-2.82965419628534E-32,-0.499999999999992));
#7906=DIRECTION('center_axis',(-0.866025403784443,1.23259516440783E-32,
0.499999999999992));
#7907=DIRECTION('ref_axis',(0.499999999999992,1.98035884533862E-47,0.866025403784443));
#7908=DIRECTION('center_axis',(0.866025403784442,0.,-0.499999999999993));
#7909=DIRECTION('ref_axis',(-0.499999999999993,0.,-0.866025403784443));
#7910=DIRECTION('center_axis',(9.81918948666102E-17,1.,1.70073350800434E-16));
#7911=DIRECTION('ref_axis',(0.,0.,1.));
#7912=DIRECTION('center_axis',(-0.499999999999993,0.,-0.866025403784443));
#7913=DIRECTION('ref_axis',(-0.866025403784443,0.,0.499999999999993));
#7914=DIRECTION('center_axis',(-0.499999999999992,1.96383789733223E-16,
-0.866025403784443));
#7915=DIRECTION('ref_axis',(-0.866025403784443,3.11793429776653E-31,0.499999999999992));
#7916=DIRECTION('center_axis',(-0.499999999999992,2.32408877239612E-16,
-0.866025403784443));
#7917=DIRECTION('ref_axis',(-0.866025403784443,-4.65759760521399E-33,0.499999999999992));
#7918=DIRECTION('center_axis',(9.81918948666102E-17,1.,1.70073350800434E-16));
#7919=DIRECTION('ref_axis',(0.,0.,1.));
#7920=DIRECTION('center_axis',(-0.350093031278002,3.65204128232947E-15,
-0.936714934999213));
#7921=DIRECTION('ref_axis',(-0.936714934999213,-9.98642723764943E-32,0.350093031278002));
#7922=DIRECTION('axis',(0.,0.,1.));
#7923=DIRECTION('refdir',(1.,0.,0.));
#7924=DIRECTION('center_axis',(0.010041653963972,-0.999936721719416,0.00507126637988255));
#7925=DIRECTION('ref_axis',(0.999949580025092,0.010041783090799,-1.60007301981504E-17));
#7926=DIRECTION('center_axis',(-0.00891671946192249,0.999950105367358,0.0045032088389469));
#7927=DIRECTION('ref_axis',(-0.999960244460585,-0.00891680987388346,-1.13603182561227E-17));
#7928=DIRECTION('center_axis',(-0.999091404712184,0.0388570551898569,0.0175069783860113));
#7929=DIRECTION('ref_axis',(-0.0388630112918391,-0.999244547822669,2.07434801815803E-18));
#7930=DIRECTION('center_axis',(-1.61571391014197E-6,0.424667837114185,0.90534922992078));
#7931=DIRECTION('ref_axis',(1.42145081289922E-6,0.905349229922022,-0.424667837112231));
#7932=DIRECTION('center_axis',(0.999152984554678,-0.0375175097387351,0.0169041390932047));
#7933=DIRECTION('ref_axis',(0.0375228712004652,0.999295769097855,-1.81623557326339E-18));
#7934=DIRECTION('center_axis',(0.,-1.,0.));
#7935=DIRECTION('ref_axis',(0.,0.,-1.));
#7936=DIRECTION('center_axis',(0.,1.,0.));
#7937=DIRECTION('ref_axis',(0.,0.,-1.));
#7938=DIRECTION('center_axis',(0.,0.,1.));
#7939=DIRECTION('ref_axis',(1.,0.,0.));
#7940=DIRECTION('',(0.,0.,1.));
#7941=DIRECTION('center_axis',(-0.489387119106713,-5.09160744540987E-5,
0.872066651730236));
#7942=DIRECTION('ref_axis',(-0.106617366365419,-0.992494824264684,-0.0598895733589422));
#7943=DIRECTION('center_axis',(0.,-1.,0.));
#7944=DIRECTION('ref_axis',(0.,0.,-1.));
#7945=DIRECTION('center_axis',(0.,-1.,0.));
#7946=DIRECTION('ref_axis',(0.,0.,-1.));
#7947=DIRECTION('center_axis',(0.,-1.,0.));
#7948=DIRECTION('ref_axis',(0.,0.,-1.));
#7949=DIRECTION('',(0.,1.,0.));
#7950=DIRECTION('center_axis',(0.,-1.,0.));
#7951=DIRECTION('ref_axis',(0.,0.,-1.));
#7952=DIRECTION('center_axis',(0.,1.,0.));
#7953=DIRECTION('ref_axis',(0.,0.,1.));
#7954=DIRECTION('',(8.65956056235489E-17,-0.707106781186551,0.707106781186544));
#7955=DIRECTION('center_axis',(0.,1.,0.));
#7956=DIRECTION('ref_axis',(0.,0.,1.));
#7957=DIRECTION('center_axis',(0.,1.,0.));
#7958=DIRECTION('ref_axis',(0.,0.,1.));
#7959=DIRECTION('center_axis',(0.,1.,0.));
#7960=DIRECTION('ref_axis',(0.,0.,1.));
#7961=DIRECTION('',(8.65956056235486E-17,-0.707106781186554,0.707106781186541));
#7962=DIRECTION('center_axis',(0.,-1.,0.));
#7963=DIRECTION('ref_axis',(0.,0.,1.));
#7964=DIRECTION('center_axis',(0.,-1.,0.));
#7965=DIRECTION('ref_axis',(0.,0.,-1.));
#7966=DIRECTION('center_axis',(0.,-1.,0.));
#7967=DIRECTION('ref_axis',(0.,0.,-1.));
#7968=DIRECTION('',(0.,1.,0.));
#7969=DIRECTION('center_axis',(0.,-1.,0.));
#7970=DIRECTION('ref_axis',(0.,0.,-1.));
#7971=DIRECTION('center_axis',(0.,-1.,0.));
#7972=DIRECTION('ref_axis',(0.,0.,-1.));
#7973=DIRECTION('',(0.,1.,0.));
#7974=DIRECTION('',(0.,1.,0.));
#7975=DIRECTION('center_axis',(0.,1.,0.));
#7976=DIRECTION('ref_axis',(0.,0.,1.));
#7977=DIRECTION('center_axis',(-6.90968518692092E-5,-0.425975505302661,
0.904734692662865));
#7978=DIRECTION('ref_axis',(0.000745635165897718,-0.904734465265813,-0.425975341291467));
#7979=DIRECTION('center_axis',(0.,1.,0.));
#7980=DIRECTION('ref_axis',(0.,0.,1.));
#7981=DIRECTION('center_axis',(0.,-1.,0.));
#7982=DIRECTION('ref_axis',(0.,0.,-1.));
#7983=DIRECTION('center_axis',(0.,1.,0.));
#7984=DIRECTION('ref_axis',(0.,0.,1.));
#7985=DIRECTION('center_axis',(-1.,0.,-2.76472863796254E-16));
#7986=DIRECTION('ref_axis',(-2.76472863796254E-16,0.,1.));
#7987=DIRECTION('',(0.,1.,0.));
#7988=DIRECTION('',(-2.76472863796254E-16,0.,1.));
#7989=DIRECTION('',(0.,1.,0.));
#7990=DIRECTION('',(-2.76472863796254E-16,0.,1.));
#7991=DIRECTION('center_axis',(-0.5,0.,0.866025403784438));
#7992=DIRECTION('ref_axis',(0.866025403784438,0.,0.5));
#7993=DIRECTION('',(0.866025403784438,0.,0.5));
#7994=DIRECTION('',(0.,1.,0.));
#7995=DIRECTION('',(0.866025403784438,0.,0.5));
#7996=DIRECTION('center_axis',(0.5,0.,0.866025403784439));
#7997=DIRECTION('ref_axis',(0.866025403784439,0.,-0.5));
#7998=DIRECTION('',(0.866025403784439,0.,-0.5));
#7999=DIRECTION('',(0.,1.,0.));
#8000=DIRECTION('',(0.866025403784439,0.,-0.5));
#8001=DIRECTION('center_axis',(1.,0.,0.));
#8002=DIRECTION('ref_axis',(0.,0.,-1.));
#8003=DIRECTION('',(0.,0.,-1.));
#8004=DIRECTION('',(0.,1.,0.));
#8005=DIRECTION('',(0.,0.,-1.));
#8006=DIRECTION('center_axis',(0.5,0.,-0.866025403784439));
#8007=DIRECTION('ref_axis',(-0.866025403784439,0.,-0.5));
#8008=DIRECTION('',(-0.866025403784438,0.,-0.5));
#8009=DIRECTION('',(0.,1.,0.));
#8010=DIRECTION('',(-0.866025403784438,0.,-0.5));
#8011=DIRECTION('center_axis',(-0.5,0.,-0.866025403784439));
#8012=DIRECTION('ref_axis',(-0.866025403784439,0.,0.5));
#8013=DIRECTION('',(-0.866025403784439,0.,0.5));
#8014=DIRECTION('',(-0.866025403784439,0.,0.5));
#8015=DIRECTION('center_axis',(0.,1.,0.));
#8016=DIRECTION('ref_axis',(0.,0.,1.));
#8017=DIRECTION('center_axis',(0.,-1.,0.));
#8018=DIRECTION('ref_axis',(0.,0.,-1.));
#8019=DIRECTION('center_axis',(0.,1.,0.));
#8020=DIRECTION('ref_axis',(0.,0.,-1.));
#8021=DIRECTION('center_axis',(0.,-1.,0.));
#8022=DIRECTION('ref_axis',(0.,0.,-1.));
#8023=DIRECTION('center_axis',(0.,1.,0.));
#8024=DIRECTION('ref_axis',(7.105427357601E-15,0.,-1.));
#8025=DIRECTION('center_axis',(0.,-1.,0.));
#8026=DIRECTION('ref_axis',(0.,0.,-1.));
#8027=DIRECTION('center_axis',(0.,1.,0.));
#8028=DIRECTION('ref_axis',(3.5527136788005E-15,0.,-1.));
#8029=DIRECTION('center_axis',(0.,-1.,0.));
#8030=DIRECTION('ref_axis',(1.22464679914735E-16,0.,1.));
#8031=DIRECTION('center_axis',(0.,1.,0.));
#8032=DIRECTION('ref_axis',(5.32907051820075E-15,0.,-1.));
#8033=DIRECTION('center_axis',(0.,-1.,0.));
#8034=DIRECTION('ref_axis',(0.,0.,-1.));
#8035=DIRECTION('center_axis',(0.,1.,0.));
#8036=DIRECTION('ref_axis',(-8.88178419700125E-16,0.,-1.));
#8037=DIRECTION('center_axis',(0.,-1.,0.));
#8038=DIRECTION('ref_axis',(0.,0.,-1.));
#8039=DIRECTION('axis',(0.,0.,1.));
#8040=DIRECTION('refdir',(1.,0.,0.));
#8041=DIRECTION('center_axis',(6.12323399573677E-17,0.,1.));
#8042=DIRECTION('ref_axis',(1.,0.,0.));
#8043=DIRECTION('center_axis',(0.,0.,1.));
#8044=DIRECTION('ref_axis',(1.,0.,0.));
#8045=DIRECTION('center_axis',(1.22464679914735E-16,-1.,0.));
#8046=DIRECTION('ref_axis',(-1.,-1.22464679914735E-16,0.));
#8047=DIRECTION('center_axis',(0.,0.,1.));
#8048=DIRECTION('ref_axis',(1.,0.,0.));
#8049=DIRECTION('center_axis',(6.12323399573677E-17,0.,1.));
#8050=DIRECTION('ref_axis',(1.,0.,0.));
#8051=DIRECTION('center_axis',(0.,0.,1.));
#8052=DIRECTION('ref_axis',(1.,0.,0.));
#8053=DIRECTION('center_axis',(1.22464679914735E-16,-1.,0.));
#8054=DIRECTION('ref_axis',(-1.,-1.22464679914735E-16,0.));
#8055=DIRECTION('center_axis',(0.,0.,1.));
#8056=DIRECTION('ref_axis',(1.,0.,0.));
#8057=DIRECTION('center_axis',(0.,0.,-1.));
#8058=DIRECTION('ref_axis',(-1.,0.,0.));
#8059=DIRECTION('',(0.,0.,1.));
#8060=DIRECTION('axis',(0.,0.,1.));
#8061=DIRECTION('refdir',(1.,0.,0.));
#8062=DIRECTION('center_axis',(0.,0.,1.));
#8063=DIRECTION('ref_axis',(1.,0.,0.));
#8064=DIRECTION('center_axis',(0.,0.,-1.));
#8065=DIRECTION('ref_axis',(-1.,0.,0.));
#8066=DIRECTION('',(-0.819152044288989,-1.00317192905352E-16,0.57357643635105));
#8067=DIRECTION('center_axis',(0.,0.,-1.));
#8068=DIRECTION('ref_axis',(-1.,0.,0.));
#8069=DIRECTION('center_axis',(0.,0.,-1.));
#8070=DIRECTION('ref_axis',(-1.,0.,0.));
#8071=DIRECTION('center_axis',(0.,0.,-1.));
#8072=DIRECTION('ref_axis',(-1.,0.,0.));
#8073=DIRECTION('center_axis',(0.,0.,-1.));
#8074=DIRECTION('ref_axis',(-1.,0.,0.));
#8075=DIRECTION('center_axis',(0.,0.,-1.));
#8076=DIRECTION('ref_axis',(-1.,0.,0.));
#8077=DIRECTION('',(0.819152044288998,-1.00317192905353E-16,-0.573576436351038));
#8078=DIRECTION('center_axis',(0.,0.,1.));
#8079=DIRECTION('ref_axis',(1.,0.,0.));
#8080=DIRECTION('center_axis',(0.,0.,-1.));
#8081=DIRECTION('ref_axis',(-1.,0.,0.));
#8082=DIRECTION('',(-0.819152044288989,-1.00317192905352E-16,0.57357643635105));
#8083=DIRECTION('center_axis',(0.,0.,-1.));
#8084=DIRECTION('ref_axis',(-1.,0.,0.));
#8085=DIRECTION('center_axis',(0.,0.,-1.));
#8086=DIRECTION('ref_axis',(-1.,0.,0.));
#8087=DIRECTION('center_axis',(0.,0.,-1.));
#8088=DIRECTION('ref_axis',(-1.,0.,0.));
#8089=DIRECTION('center_axis',(0.,0.,-1.));
#8090=DIRECTION('ref_axis',(-1.,0.,0.));
#8091=DIRECTION('center_axis',(0.,0.,-1.));
#8092=DIRECTION('ref_axis',(-1.,0.,0.));
#8093=DIRECTION('',(0.819152044288998,-1.00317192905353E-16,-0.573576436351038));
#8094=DIRECTION('center_axis',(0.,0.,1.));
#8095=DIRECTION('ref_axis',(1.,0.,0.));
#8096=DIRECTION('center_axis',(0.,0.,-1.));
#8097=DIRECTION('ref_axis',(-1.,0.,0.));
#8098=DIRECTION('',(-0.819152044288989,-1.00317192905352E-16,0.57357643635105));
#8099=DIRECTION('center_axis',(0.,0.,-1.));
#8100=DIRECTION('ref_axis',(-1.,0.,0.));
#8101=DIRECTION('center_axis',(0.,0.,-1.));
#8102=DIRECTION('ref_axis',(-1.,0.,0.));
#8103=DIRECTION('center_axis',(0.,0.,-1.));
#8104=DIRECTION('ref_axis',(-1.,0.,0.));
#8105=DIRECTION('center_axis',(0.,0.,-1.));
#8106=DIRECTION('ref_axis',(-1.,0.,0.));
#8107=DIRECTION('center_axis',(0.,0.,-1.));
#8108=DIRECTION('ref_axis',(-1.,0.,0.));
#8109=DIRECTION('',(0.819152044288998,-1.00317192905353E-16,-0.573576436351038));
#8110=DIRECTION('center_axis',(0.,0.,1.));
#8111=DIRECTION('ref_axis',(1.,0.,0.));
#8112=DIRECTION('center_axis',(0.,0.,-1.));
#8113=DIRECTION('ref_axis',(-1.,0.,0.));
#8114=DIRECTION('',(-0.819152044288989,-1.00317192905352E-16,0.57357643635105));
#8115=DIRECTION('center_axis',(0.,0.,-1.));
#8116=DIRECTION('ref_axis',(-1.,0.,0.));
#8117=DIRECTION('center_axis',(0.,0.,-1.));
#8118=DIRECTION('ref_axis',(-1.,0.,0.));
#8119=DIRECTION('center_axis',(0.,0.,-1.));
#8120=DIRECTION('ref_axis',(-1.,0.,0.));
#8121=DIRECTION('center_axis',(0.,0.,1.));
#8122=DIRECTION('ref_axis',(-1.,0.,0.));
#8123=DIRECTION('',(0.819152044288998,-1.00317192905353E-16,-0.573576436351038));
#8124=DIRECTION('center_axis',(0.,0.,1.));
#8125=DIRECTION('ref_axis',(-1.,0.,0.));
#8126=DIRECTION('center_axis',(0.,0.,1.));
#8127=DIRECTION('ref_axis',(1.,0.,0.));
#8128=DIRECTION('center_axis',(0.,0.,-1.));
#8129=DIRECTION('ref_axis',(1.,0.,0.));
#8130=DIRECTION('',(0.,0.,1.));
#8131=DIRECTION('center_axis',(0.,0.,1.));
#8132=DIRECTION('ref_axis',(1.,0.,0.));
#8133=DIRECTION('center_axis',(0.,0.,1.));
#8134=DIRECTION('ref_axis',(1.,0.,0.));
#8135=DIRECTION('center_axis',(0.,0.,-1.));
#8136=DIRECTION('ref_axis',(-1.,0.,0.));
#8137=DIRECTION('center_axis',(0.,0.,1.));
#8138=DIRECTION('ref_axis',(-1.,0.,0.));
#8139=DIRECTION('',(0.819152044288991,-1.00317192905352E-16,-0.573576436351047));
#8140=DIRECTION('center_axis',(0.,0.,1.));
#8141=DIRECTION('ref_axis',(-1.,0.,0.));
#8142=DIRECTION('center_axis',(0.,0.,1.));
#8143=DIRECTION('ref_axis',(1.,0.,0.));
#8144=DIRECTION('',(-0.81915204428899,-1.00317192905352E-16,0.573576436351049));
#8145=DIRECTION('center_axis',(0.,0.,1.));
#8146=DIRECTION('ref_axis',(1.,0.,0.));
#8147=DIRECTION('center_axis',(0.,0.,1.));
#8148=DIRECTION('ref_axis',(1.,0.,0.));
#8149=DIRECTION('',(0.,0.,1.));
#8150=DIRECTION('center_axis',(0.,0.,1.));
#8151=DIRECTION('ref_axis',(1.,0.,0.));
#8152=DIRECTION('',(0.,0.,1.));
#8153=DIRECTION('center_axis',(0.,0.,1.));
#8154=DIRECTION('ref_axis',(1.,0.,0.));
#8155=DIRECTION('',(0.,0.,1.));
#8156=DIRECTION('center_axis',(0.,0.,1.));
#8157=DIRECTION('ref_axis',(1.,0.,0.));
#8158=DIRECTION('',(0.,0.,1.));
#8159=DIRECTION('center_axis',(-0.500000000000003,0.866025403784437,0.));
#8160=DIRECTION('ref_axis',(-0.866025403784437,-0.500000000000003,0.));
#8161=DIRECTION('',(0.,0.,1.));
#8162=DIRECTION('',(0.,0.,1.));
#8163=DIRECTION('center_axis',(0.500000000000003,0.866025403784437,0.));
#8164=DIRECTION('ref_axis',(-0.866025403784437,0.500000000000003,0.));
#8165=DIRECTION('',(0.,0.,1.));
#8166=DIRECTION('center_axis',(-1.,0.,0.));
#8167=DIRECTION('ref_axis',(0.,0.,1.));
#8168=DIRECTION('',(0.,0.,1.));
#8169=DIRECTION('center_axis',(0.500000000000003,-0.866025403784437,0.));
#8170=DIRECTION('ref_axis',(0.866025403784437,0.500000000000003,0.));
#8171=DIRECTION('',(0.,0.,1.));
#8172=DIRECTION('center_axis',(-0.500000000000003,-0.866025403784437,0.));
#8173=DIRECTION('ref_axis',(0.866025403784437,-0.500000000000004,0.));
#8174=DIRECTION('',(0.,0.,1.));
#8175=DIRECTION('center_axis',(-1.,0.,0.));
#8176=DIRECTION('ref_axis',(0.,0.,1.));
#8177=DIRECTION('center_axis',(0.,0.,1.));
#8178=DIRECTION('ref_axis',(1.,0.,0.));
#8179=DIRECTION('center_axis',(0.,0.,1.));
#8180=DIRECTION('ref_axis',(1.,0.,0.));
#8181=DIRECTION('center_axis',(0.,0.,1.));
#8182=DIRECTION('ref_axis',(1.,0.,0.));
#8183=DIRECTION('center_axis',(0.,0.,1.));
#8184=DIRECTION('ref_axis',(1.,0.,0.));
#8185=DIRECTION('center_axis',(0.,0.,1.));
#8186=DIRECTION('ref_axis',(1.,0.,0.));
#8187=DIRECTION('center_axis',(0.,0.,1.));
#8188=DIRECTION('ref_axis',(1.,0.,0.));
#8189=DIRECTION('center_axis',(0.,0.,1.));
#8190=DIRECTION('ref_axis',(1.,0.,0.));
#8191=DIRECTION('center_axis',(0.,0.,1.));
#8192=DIRECTION('ref_axis',(1.,0.,0.));
#8193=DIRECTION('center_axis',(0.,0.,1.));
#8194=DIRECTION('ref_axis',(1.,0.,0.));
#8195=DIRECTION('center_axis',(0.,0.,-1.));
#8196=DIRECTION('ref_axis',(1.,0.,0.));
#8197=DIRECTION('center_axis',(0.,0.,-1.));
#8198=DIRECTION('ref_axis',(1.,0.,0.));
#8199=DIRECTION('center_axis',(0.,0.,-1.));
#8200=DIRECTION('ref_axis',(1.,1.77635683940025E-15,0.));
#8201=DIRECTION('center_axis',(0.,0.,-1.));
#8202=DIRECTION('ref_axis',(1.,-1.77635683940025E-15,0.));
#8203=DIRECTION('center_axis',(0.,0.,-1.));
#8204=DIRECTION('ref_axis',(1.,1.77635683940025E-15,0.));
#8205=DIRECTION('center_axis',(0.,0.,1.));
#8206=DIRECTION('ref_axis',(1.,0.,0.));
#8207=DIRECTION('center_axis',(0.,0.,1.));
#8208=DIRECTION('ref_axis',(1.,0.,0.));
#8209=DIRECTION('center_axis',(0.,0.,1.));
#8210=DIRECTION('ref_axis',(1.,0.,0.));
#8211=DIRECTION('center_axis',(0.,0.,1.));
#8212=DIRECTION('ref_axis',(1.,0.,0.));
#8213=DIRECTION('center_axis',(0.,0.,1.));
#8214=DIRECTION('ref_axis',(1.,0.,0.));
#8215=DIRECTION('center_axis',(0.,0.,1.));
#8216=DIRECTION('ref_axis',(1.,0.,0.));
#8217=DIRECTION('center_axis',(0.,0.,-1.));
#8218=DIRECTION('ref_axis',(-1.,0.,0.));
#8219=DIRECTION('center_axis',(0.,0.,-1.));
#8220=DIRECTION('ref_axis',(-1.,0.,0.));
#8221=DIRECTION('center_axis',(0.,0.,-1.));
#8222=DIRECTION('ref_axis',(-1.,0.,0.));
#8223=DIRECTION('center_axis',(0.,0.,-1.));
#8224=DIRECTION('ref_axis',(-1.,0.,0.));
#8225=DIRECTION('center_axis',(0.,0.,-1.));
#8226=DIRECTION('ref_axis',(-1.,0.,0.));
#8227=DIRECTION('center_axis',(0.,0.,-1.));
#8228=DIRECTION('ref_axis',(-1.,0.,0.));
#8229=DIRECTION('axis',(0.,0.,1.));
#8230=DIRECTION('refdir',(1.,0.,0.));
#8231=DIRECTION('center_axis',(-8.48851915644968E-18,0.,-1.));
#8232=DIRECTION('ref_axis',(-1.,0.,8.48851915644968E-18));
#8233=DIRECTION('center_axis',(-8.48851915644968E-18,0.,-1.));
#8234=DIRECTION('ref_axis',(-1.,0.,8.48851915644968E-18));
#8235=DIRECTION('',(8.48851915644968E-18,0.,1.));
#8236=DIRECTION('center_axis',(-8.48851915644968E-18,0.,-1.));
#8237=DIRECTION('ref_axis',(-1.,0.,8.48851915644968E-18));
#8238=DIRECTION('center_axis',(-6.12323399573677E-17,1.,0.));
#8239=DIRECTION('ref_axis',(-1.,0.,0.));
#8240=DIRECTION('center_axis',(-8.48851915644968E-18,0.,-1.));
#8241=DIRECTION('ref_axis',(-1.,0.,8.48851915644968E-18));
#8242=DIRECTION('center_axis',(-8.48851915644968E-18,0.,-1.));
#8243=DIRECTION('ref_axis',(-1.,0.,8.48851915644968E-18));
#8244=DIRECTION('center_axis',(-8.48851915644968E-18,0.,-1.));
#8245=DIRECTION('ref_axis',(-1.,0.,8.48851915644968E-18));
#8246=DIRECTION('axis',(0.,0.,1.));
#8247=DIRECTION('refdir',(1.,0.,0.));
#8248=DIRECTION('center_axis',(-1.,0.,0.));
#8249=DIRECTION('ref_axis',(0.,0.,1.));
#8250=DIRECTION('center_axis',(1.,1.22460635382238E-16,0.));
#8251=DIRECTION('ref_axis',(-1.22460635382238E-16,1.,0.));
#8252=DIRECTION('center_axis',(1.,1.22460635382238E-16,0.));
#8253=DIRECTION('ref_axis',(-1.22460635382238E-16,1.,0.));
#8254=DIRECTION('',(0.707106781186552,8.65956056235487E-17,0.707106781186543));
#8255=DIRECTION('center_axis',(-1.,0.,0.));
#8256=DIRECTION('ref_axis',(0.,0.,1.));
#8257=DIRECTION('center_axis',(-1.,-1.22460635382238E-16,0.));
#8258=DIRECTION('ref_axis',(1.22460635382238E-16,-1.,0.));
#8259=DIRECTION('center_axis',(-1.,-1.22460635382238E-16,0.));
#8260=DIRECTION('ref_axis',(1.22460635382238E-16,-1.,0.));
#8261=DIRECTION('center_axis',(-1.,-1.22460635382238E-16,0.));
#8262=DIRECTION('ref_axis',(1.22460635382238E-16,-1.,0.));
#8263=DIRECTION('',(0.57357643635105,-0.819152044288989,1.00317192905352E-16));
#8264=DIRECTION('center_axis',(-1.,-1.22460635382238E-16,0.));
#8265=DIRECTION('ref_axis',(1.22460635382238E-16,-1.,0.));
#8266=DIRECTION('center_axis',(-1.,-1.22460635382238E-16,0.));
#8267=DIRECTION('ref_axis',(1.22460635382238E-16,-1.,0.));
#8268=DIRECTION('center_axis',(1.,1.22460635382238E-16,0.));
#8269=DIRECTION('ref_axis',(-1.22460635382238E-16,1.,0.));
#8270=DIRECTION('',(-0.573576436351045,0.819152044288993,1.00317192905353E-16));
#8271=DIRECTION('center_axis',(-1.,0.,0.));
#8272=DIRECTION('ref_axis',(0.,0.,1.));
#8273=DIRECTION('center_axis',(-1.,-1.22460635382238E-16,0.));
#8274=DIRECTION('ref_axis',(1.22460635382238E-16,-1.,0.));
#8275=DIRECTION('center_axis',(-1.,-1.22460635382238E-16,0.));
#8276=DIRECTION('ref_axis',(1.22460635382238E-16,-1.,0.));
#8277=DIRECTION('',(1.,0.,0.));
#8278=DIRECTION('center_axis',(-1.,-1.22460635382238E-16,0.));
#8279=DIRECTION('ref_axis',(1.22460635382238E-16,-1.,0.));
#8280=DIRECTION('center_axis',(-1.,-1.22460635382238E-16,0.));
#8281=DIRECTION('ref_axis',(1.22460635382238E-16,-1.,0.));
#8282=DIRECTION('center_axis',(-1.,-1.22460635382238E-16,0.));
#8283=DIRECTION('ref_axis',(1.22460635382238E-16,-1.,0.));
#8284=DIRECTION('',(0.57357643635105,-0.819152044288989,1.00317192905352E-16));
#8285=DIRECTION('center_axis',(-1.,-1.22460635382238E-16,0.));
#8286=DIRECTION('ref_axis',(1.22460635382238E-16,-1.,0.));
#8287=DIRECTION('center_axis',(-1.,-1.22460635382238E-16,0.));
#8288=DIRECTION('ref_axis',(1.22460635382238E-16,-1.,0.));
#8289=DIRECTION('center_axis',(1.,1.22460635382238E-16,0.));
#8290=DIRECTION('ref_axis',(-1.22460635382238E-16,1.,0.));
#8291=DIRECTION('',(-0.573576436351045,0.819152044288993,1.00317192905353E-16));
#8292=DIRECTION('center_axis',(-1.,0.,0.));
#8293=DIRECTION('ref_axis',(0.,0.,1.));
#8294=DIRECTION('center_axis',(-1.,-1.22460635382238E-16,0.));
#8295=DIRECTION('ref_axis',(1.22460635382238E-16,-1.,0.));
#8296=DIRECTION('center_axis',(-1.,-1.22460635382238E-16,0.));
#8297=DIRECTION('ref_axis',(1.22460635382238E-16,-1.,0.));
#8298=DIRECTION('',(1.,0.,0.));
#8299=DIRECTION('center_axis',(-1.,-1.22460635382238E-16,0.));
#8300=DIRECTION('ref_axis',(1.22460635382238E-16,-1.,0.));
#8301=DIRECTION('center_axis',(-1.,-1.22460635382238E-16,0.));
#8302=DIRECTION('ref_axis',(1.22460635382238E-16,-1.,0.));
#8303=DIRECTION('center_axis',(-1.,-1.22460635382238E-16,0.));
#8304=DIRECTION('ref_axis',(1.22460635382238E-16,-1.,0.));
#8305=DIRECTION('',(0.57357643635105,-0.819152044288989,1.00317192905352E-16));
#8306=DIRECTION('center_axis',(-1.,-1.22460635382238E-16,0.));
#8307=DIRECTION('ref_axis',(1.22460635382238E-16,-1.,0.));
#8308=DIRECTION('center_axis',(-1.,-1.22460635382238E-16,0.));
#8309=DIRECTION('ref_axis',(1.22460635382238E-16,-1.,0.));
#8310=DIRECTION('center_axis',(1.,1.22460635382238E-16,0.));
#8311=DIRECTION('ref_axis',(-1.22460635382238E-16,1.,0.));
#8312=DIRECTION('',(-0.573576436351045,0.819152044288993,1.00317192905353E-16));
#8313=DIRECTION('center_axis',(-1.,0.,0.));
#8314=DIRECTION('ref_axis',(0.,0.,1.));
#8315=DIRECTION('center_axis',(-1.,-1.22460635382238E-16,0.));
#8316=DIRECTION('ref_axis',(1.22460635382238E-16,-1.,0.));
#8317=DIRECTION('center_axis',(-1.,-1.22460635382238E-16,0.));
#8318=DIRECTION('ref_axis',(1.22460635382238E-16,-1.,0.));
#8319=DIRECTION('',(1.,0.,0.));
#8320=DIRECTION('center_axis',(-1.,-1.22460635382238E-16,0.));
#8321=DIRECTION('ref_axis',(1.22460635382238E-16,-1.,0.));
#8322=DIRECTION('center_axis',(-1.,-1.22460635382238E-16,0.));
#8323=DIRECTION('ref_axis',(1.22460635382238E-16,-1.,0.));
#8324=DIRECTION('center_axis',(-1.,-1.22460635382238E-16,0.));
#8325=DIRECTION('ref_axis',(1.22460635382238E-16,-1.,0.));
#8326=DIRECTION('',(0.57357643635105,-0.819152044288989,1.00317192905352E-16));
#8327=DIRECTION('center_axis',(-1.,-1.22460635382238E-16,0.));
#8328=DIRECTION('ref_axis',(1.22460635382238E-16,-1.,0.));
#8329=DIRECTION('center_axis',(-1.,-1.22460635382238E-16,0.));
#8330=DIRECTION('ref_axis',(1.22460635382238E-16,-1.,0.));
#8331=DIRECTION('center_axis',(1.,1.22460635382238E-16,0.));
#8332=DIRECTION('ref_axis',(-1.22460635382238E-16,1.,0.));
#8333=DIRECTION('',(-0.573576436351045,0.819152044288993,1.00317192905353E-16));
#8334=DIRECTION('center_axis',(-1.,0.,0.));
#8335=DIRECTION('ref_axis',(0.,0.,1.));
#8336=DIRECTION('center_axis',(-1.,-1.22460635382238E-16,0.));
#8337=DIRECTION('ref_axis',(1.22460635382238E-16,-1.,0.));
#8338=DIRECTION('center_axis',(-1.,-1.22460635382238E-16,0.));
#8339=DIRECTION('ref_axis',(1.22460635382238E-16,-1.,0.));
#8340=DIRECTION('',(1.,0.,0.));
#8341=DIRECTION('center_axis',(-1.,-1.22460635382238E-16,0.));
#8342=DIRECTION('ref_axis',(1.22460635382238E-16,-1.,0.));
#8343=DIRECTION('center_axis',(-1.,-1.22460635382238E-16,0.));
#8344=DIRECTION('ref_axis',(1.22460635382238E-16,-1.,0.));
#8345=DIRECTION('center_axis',(-1.,-1.22460635382238E-16,0.));
#8346=DIRECTION('ref_axis',(1.22460635382238E-16,-1.,0.));
#8347=DIRECTION('',(0.57357643635105,-0.819152044288989,1.00317192905352E-16));
#8348=DIRECTION('center_axis',(-1.,-1.22460635382238E-16,0.));
#8349=DIRECTION('ref_axis',(1.22460635382238E-16,-1.,0.));
#8350=DIRECTION('center_axis',(-1.,-1.22460635382238E-16,0.));
#8351=DIRECTION('ref_axis',(1.22460635382238E-16,-1.,0.));
#8352=DIRECTION('center_axis',(1.,1.22460635382238E-16,0.));
#8353=DIRECTION('ref_axis',(-1.22460635382238E-16,1.,0.));
#8354=DIRECTION('',(-0.573576436351045,0.819152044288993,1.00317192905353E-16));
#8355=DIRECTION('center_axis',(-1.,0.,0.));
#8356=DIRECTION('ref_axis',(0.,0.,1.));
#8357=DIRECTION('center_axis',(-1.,-1.22460635382238E-16,0.));
#8358=DIRECTION('ref_axis',(1.22460635382238E-16,-1.,0.));
#8359=DIRECTION('center_axis',(-1.,-1.22460635382238E-16,0.));
#8360=DIRECTION('ref_axis',(1.22460635382238E-16,-1.,0.));
#8361=DIRECTION('',(1.,0.,0.));
#8362=DIRECTION('center_axis',(-1.,-1.22460635382238E-16,0.));
#8363=DIRECTION('ref_axis',(1.22460635382238E-16,-1.,0.));
#8364=DIRECTION('center_axis',(-1.,-1.22460635382238E-16,0.));
#8365=DIRECTION('ref_axis',(1.22460635382238E-16,-1.,0.));
#8366=DIRECTION('center_axis',(-1.,-1.22460635382238E-16,0.));
#8367=DIRECTION('ref_axis',(1.22460635382238E-16,-1.,0.));
#8368=DIRECTION('',(0.57357643635105,-0.819152044288989,1.00317192905352E-16));
#8369=DIRECTION('center_axis',(-1.,-1.22460635382238E-16,0.));
#8370=DIRECTION('ref_axis',(1.22460635382238E-16,-1.,0.));
#8371=DIRECTION('center_axis',(-1.,-1.22460635382238E-16,0.));
#8372=DIRECTION('ref_axis',(1.22460635382238E-16,-1.,0.));
#8373=DIRECTION('center_axis',(1.,1.22460635382238E-16,0.));
#8374=DIRECTION('ref_axis',(-1.22460635382238E-16,1.,0.));
#8375=DIRECTION('',(-0.573576436351045,0.819152044288993,1.00317192905353E-16));
#8376=DIRECTION('center_axis',(-1.,0.,0.));
#8377=DIRECTION('ref_axis',(0.,0.,1.));
#8378=DIRECTION('center_axis',(-1.,-1.22460635382238E-16,0.));
#8379=DIRECTION('ref_axis',(1.22460635382238E-16,-1.,0.));
#8380=DIRECTION('center_axis',(-1.,-1.22460635382238E-16,0.));
#8381=DIRECTION('ref_axis',(1.22460635382238E-16,-1.,0.));
#8382=DIRECTION('',(1.,0.,0.));
#8383=DIRECTION('center_axis',(-1.,-1.22460635382238E-16,0.));
#8384=DIRECTION('ref_axis',(1.22460635382238E-16,-1.,0.));
#8385=DIRECTION('center_axis',(-1.,-1.22460635382238E-16,0.));
#8386=DIRECTION('ref_axis',(1.22460635382238E-16,-1.,0.));
#8387=DIRECTION('center_axis',(-1.,-1.22460635382238E-16,0.));
#8388=DIRECTION('ref_axis',(1.22460635382238E-16,-1.,0.));
#8389=DIRECTION('',(0.57357643635105,-0.819152044288989,1.00317192905352E-16));
#8390=DIRECTION('center_axis',(-1.,-1.22460635382238E-16,0.));
#8391=DIRECTION('ref_axis',(1.22460635382238E-16,-1.,0.));
#8392=DIRECTION('center_axis',(-1.,-1.22460635382238E-16,0.));
#8393=DIRECTION('ref_axis',(1.22460635382238E-16,-1.,0.));
#8394=DIRECTION('center_axis',(1.,1.22460635382238E-16,0.));
#8395=DIRECTION('ref_axis',(-1.22460635382238E-16,1.,0.));
#8396=DIRECTION('',(-0.573576436351045,0.819152044288993,1.00317192905353E-16));
#8397=DIRECTION('center_axis',(-1.,0.,0.));
#8398=DIRECTION('ref_axis',(0.,0.,1.));
#8399=DIRECTION('center_axis',(-1.,-1.22460635382238E-16,0.));
#8400=DIRECTION('ref_axis',(1.22460635382238E-16,-1.,0.));
#8401=DIRECTION('center_axis',(-1.,-1.22460635382238E-16,0.));
#8402=DIRECTION('ref_axis',(1.22460635382238E-16,-1.,0.));
#8403=DIRECTION('',(1.,0.,0.));
#8404=DIRECTION('center_axis',(-1.,-1.22460635382238E-16,0.));
#8405=DIRECTION('ref_axis',(1.22460635382238E-16,-1.,0.));
#8406=DIRECTION('center_axis',(-1.,-1.22460635382238E-16,0.));
#8407=DIRECTION('ref_axis',(1.22460635382238E-16,-1.,0.));
#8408=DIRECTION('center_axis',(-1.,-1.22460635382238E-16,0.));
#8409=DIRECTION('ref_axis',(1.22460635382238E-16,-1.,0.));
#8410=DIRECTION('',(0.57357643635105,-0.819152044288989,1.00317192905352E-16));
#8411=DIRECTION('center_axis',(-1.,-1.22460635382238E-16,0.));
#8412=DIRECTION('ref_axis',(1.22460635382238E-16,-1.,0.));
#8413=DIRECTION('center_axis',(-1.,-1.22460635382238E-16,0.));
#8414=DIRECTION('ref_axis',(1.22460635382238E-16,-1.,0.));
#8415=DIRECTION('center_axis',(1.,1.22460635382238E-16,0.));
#8416=DIRECTION('ref_axis',(-1.22460635382238E-16,1.,0.));
#8417=DIRECTION('',(-0.573576436351045,0.819152044288993,1.00317192905353E-16));
#8418=DIRECTION('center_axis',(-1.,0.,0.));
#8419=DIRECTION('ref_axis',(0.,0.,1.));
#8420=DIRECTION('center_axis',(-1.,-1.22460635382238E-16,0.));
#8421=DIRECTION('ref_axis',(1.22460635382238E-16,-1.,0.));
#8422=DIRECTION('center_axis',(-1.,-1.22460635382238E-16,0.));
#8423=DIRECTION('ref_axis',(1.22460635382238E-16,-1.,0.));
#8424=DIRECTION('',(1.,0.,0.));
#8425=DIRECTION('center_axis',(-1.,-1.22460635382238E-16,0.));
#8426=DIRECTION('ref_axis',(1.22460635382238E-16,-1.,0.));
#8427=DIRECTION('center_axis',(-1.,-1.22460635382238E-16,0.));
#8428=DIRECTION('ref_axis',(1.22460635382238E-16,-1.,0.));
#8429=DIRECTION('center_axis',(-1.,-1.22460635382238E-16,0.));
#8430=DIRECTION('ref_axis',(1.22460635382238E-16,-1.,0.));
#8431=DIRECTION('',(0.57357643635105,-0.819152044288989,1.00317192905352E-16));
#8432=DIRECTION('center_axis',(-1.,-1.22460635382238E-16,0.));
#8433=DIRECTION('ref_axis',(1.22460635382238E-16,-1.,0.));
#8434=DIRECTION('center_axis',(-1.,-1.22460635382238E-16,0.));
#8435=DIRECTION('ref_axis',(1.22460635382238E-16,-1.,0.));
#8436=DIRECTION('center_axis',(1.,1.22460635382238E-16,0.));
#8437=DIRECTION('ref_axis',(-1.22460635382238E-16,1.,0.));
#8438=DIRECTION('',(-0.573576436351045,0.819152044288993,1.00317192905353E-16));
#8439=DIRECTION('center_axis',(-1.,0.,0.));
#8440=DIRECTION('ref_axis',(0.,0.,1.));
#8441=DIRECTION('center_axis',(-1.,-1.22460635382238E-16,0.));
#8442=DIRECTION('ref_axis',(1.22460635382238E-16,-1.,0.));
#8443=DIRECTION('center_axis',(-1.,-1.22460635382238E-16,0.));
#8444=DIRECTION('ref_axis',(1.22460635382238E-16,-1.,0.));
#8445=DIRECTION('',(1.,0.,0.));
#8446=DIRECTION('center_axis',(-1.,-1.22460635382238E-16,0.));
#8447=DIRECTION('ref_axis',(1.22460635382238E-16,-1.,0.));
#8448=DIRECTION('center_axis',(-1.,-1.22460635382238E-16,0.));
#8449=DIRECTION('ref_axis',(1.22460635382238E-16,-1.,0.));
#8450=DIRECTION('center_axis',(-1.,-1.22460635382238E-16,0.));
#8451=DIRECTION('ref_axis',(1.22460635382238E-16,-1.,0.));
#8452=DIRECTION('',(0.57357643635105,-0.819152044288989,1.00317192905352E-16));
#8453=DIRECTION('center_axis',(-1.,-1.22460635382238E-16,0.));
#8454=DIRECTION('ref_axis',(1.22460635382238E-16,-1.,0.));
#8455=DIRECTION('center_axis',(-1.,-1.22460635382238E-16,0.));
#8456=DIRECTION('ref_axis',(1.22460635382238E-16,-1.,0.));
#8457=DIRECTION('center_axis',(1.,1.22460635382238E-16,0.));
#8458=DIRECTION('ref_axis',(-1.22460635382238E-16,1.,0.));
#8459=DIRECTION('',(-0.573576436351045,0.819152044288993,1.00317192905353E-16));
#8460=DIRECTION('center_axis',(-1.,0.,0.));
#8461=DIRECTION('ref_axis',(0.,0.,1.));
#8462=DIRECTION('center_axis',(-1.,-1.22460635382238E-16,0.));
#8463=DIRECTION('ref_axis',(1.22460635382238E-16,-1.,0.));
#8464=DIRECTION('center_axis',(-1.,-1.22460635382238E-16,0.));
#8465=DIRECTION('ref_axis',(1.22460635382238E-16,-1.,0.));
#8466=DIRECTION('',(1.,0.,0.));
#8467=DIRECTION('center_axis',(-1.,-1.22460635382238E-16,0.));
#8468=DIRECTION('ref_axis',(1.22460635382238E-16,-1.,0.));
#8469=DIRECTION('center_axis',(-1.,-1.22460635382238E-16,0.));
#8470=DIRECTION('ref_axis',(1.22460635382238E-16,-1.,0.));
#8471=DIRECTION('center_axis',(-1.,-1.22460635382238E-16,0.));
#8472=DIRECTION('ref_axis',(1.22460635382238E-16,-1.,0.));
#8473=DIRECTION('',(0.57357643635105,-0.819152044288989,1.00317192905352E-16));
#8474=DIRECTION('center_axis',(-1.,-1.22460635382238E-16,0.));
#8475=DIRECTION('ref_axis',(1.22460635382238E-16,-1.,0.));
#8476=DIRECTION('center_axis',(-1.,-1.22460635382238E-16,0.));
#8477=DIRECTION('ref_axis',(1.22460635382238E-16,-1.,0.));
#8478=DIRECTION('center_axis',(1.,1.22460635382238E-16,0.));
#8479=DIRECTION('ref_axis',(-1.22460635382238E-16,1.,0.));
#8480=DIRECTION('',(-0.573576436351045,0.819152044288993,1.00317192905353E-16));
#8481=DIRECTION('center_axis',(-1.,0.,0.));
#8482=DIRECTION('ref_axis',(0.,0.,1.));
#8483=DIRECTION('center_axis',(-1.,-1.22460635382238E-16,0.));
#8484=DIRECTION('ref_axis',(1.22460635382238E-16,-1.,0.));
#8485=DIRECTION('center_axis',(-1.,-1.22460635382238E-16,0.));
#8486=DIRECTION('ref_axis',(1.22460635382238E-16,-1.,0.));
#8487=DIRECTION('',(1.,0.,0.));
#8488=DIRECTION('center_axis',(-1.,-1.22460635382238E-16,0.));
#8489=DIRECTION('ref_axis',(1.22460635382238E-16,-1.,0.));
#8490=DIRECTION('center_axis',(-1.,-1.22460635382238E-16,0.));
#8491=DIRECTION('ref_axis',(1.22460635382238E-16,-1.,0.));
#8492=DIRECTION('center_axis',(-1.,-1.22460635382238E-16,0.));
#8493=DIRECTION('ref_axis',(1.22460635382238E-16,-1.,0.));
#8494=DIRECTION('',(0.57357643635105,-0.819152044288989,1.00317192905352E-16));
#8495=DIRECTION('center_axis',(-1.,-1.22460635382238E-16,0.));
#8496=DIRECTION('ref_axis',(1.22460635382238E-16,-1.,0.));
#8497=DIRECTION('center_axis',(-1.,-1.22460635382238E-16,0.));
#8498=DIRECTION('ref_axis',(1.22460635382238E-16,-1.,0.));
#8499=DIRECTION('center_axis',(1.,1.22460635382238E-16,0.));
#8500=DIRECTION('ref_axis',(-1.22460635382238E-16,1.,0.));
#8501=DIRECTION('',(-0.573576436351045,0.819152044288993,1.00317192905353E-16));
#8502=DIRECTION('center_axis',(-1.,0.,0.));
#8503=DIRECTION('ref_axis',(0.,0.,1.));
#8504=DIRECTION('center_axis',(-1.,-1.22460635382238E-16,0.));
#8505=DIRECTION('ref_axis',(1.22460635382238E-16,-1.,0.));
#8506=DIRECTION('center_axis',(-1.,-1.22460635382238E-16,0.));
#8507=DIRECTION('ref_axis',(1.22460635382238E-16,-1.,0.));
#8508=DIRECTION('',(1.,0.,0.));
#8509=DIRECTION('center_axis',(-1.,-1.22460635382238E-16,0.));
#8510=DIRECTION('ref_axis',(1.22460635382238E-16,-1.,0.));
#8511=DIRECTION('center_axis',(-1.,-1.22460635382238E-16,0.));
#8512=DIRECTION('ref_axis',(1.22460635382238E-16,-1.,0.));
#8513=DIRECTION('center_axis',(-1.,-1.22460635382238E-16,0.));
#8514=DIRECTION('ref_axis',(1.22460635382238E-16,-1.,0.));
#8515=DIRECTION('',(0.57357643635105,-0.819152044288989,1.00317192905352E-16));
#8516=DIRECTION('center_axis',(-1.,-1.22460635382238E-16,0.));
#8517=DIRECTION('ref_axis',(1.22460635382238E-16,-1.,0.));
#8518=DIRECTION('center_axis',(-1.,-1.22460635382238E-16,0.));
#8519=DIRECTION('ref_axis',(1.22460635382238E-16,-1.,0.));
#8520=DIRECTION('center_axis',(1.,1.22460635382238E-16,0.));
#8521=DIRECTION('ref_axis',(-1.22460635382238E-16,1.,0.));
#8522=DIRECTION('',(-0.573576436351045,0.819152044288993,1.00317192905353E-16));
#8523=DIRECTION('center_axis',(-1.,0.,0.));
#8524=DIRECTION('ref_axis',(0.,0.,1.));
#8525=DIRECTION('center_axis',(-1.,-1.22460635382238E-16,0.));
#8526=DIRECTION('ref_axis',(1.22460635382238E-16,-1.,0.));
#8527=DIRECTION('center_axis',(-1.,-1.22460635382238E-16,0.));
#8528=DIRECTION('ref_axis',(1.22460635382238E-16,-1.,0.));
#8529=DIRECTION('',(1.,0.,0.));
#8530=DIRECTION('center_axis',(-1.,-1.22460635382238E-16,0.));
#8531=DIRECTION('ref_axis',(1.22460635382238E-16,-1.,0.));
#8532=DIRECTION('center_axis',(-1.,-1.22460635382238E-16,0.));
#8533=DIRECTION('ref_axis',(1.22460635382238E-16,-1.,0.));
#8534=DIRECTION('center_axis',(-1.,-1.22460635382238E-16,0.));
#8535=DIRECTION('ref_axis',(1.22460635382238E-16,-1.,0.));
#8536=DIRECTION('',(0.57357643635105,-0.819152044288989,1.00317192905352E-16));
#8537=DIRECTION('center_axis',(-1.,-1.22460635382238E-16,0.));
#8538=DIRECTION('ref_axis',(1.22460635382238E-16,-1.,0.));
#8539=DIRECTION('center_axis',(-1.,-1.22460635382238E-16,0.));
#8540=DIRECTION('ref_axis',(1.22460635382238E-16,-1.,0.));
#8541=DIRECTION('center_axis',(1.,1.22460635382238E-16,0.));
#8542=DIRECTION('ref_axis',(-1.22460635382238E-16,1.,0.));
#8543=DIRECTION('',(-0.573576436351045,0.819152044288993,1.00317192905353E-16));
#8544=DIRECTION('center_axis',(-1.,0.,0.));
#8545=DIRECTION('ref_axis',(0.,0.,1.));
#8546=DIRECTION('center_axis',(-1.,-1.22460635382238E-16,0.));
#8547=DIRECTION('ref_axis',(1.22460635382238E-16,-1.,0.));
#8548=DIRECTION('center_axis',(-1.,-1.22460635382238E-16,0.));
#8549=DIRECTION('ref_axis',(1.22460635382238E-16,-1.,0.));
#8550=DIRECTION('',(1.,0.,0.));
#8551=DIRECTION('center_axis',(-1.,-1.22460635382238E-16,0.));
#8552=DIRECTION('ref_axis',(1.22460635382238E-16,-1.,0.));
#8553=DIRECTION('center_axis',(-1.,-1.22460635382238E-16,0.));
#8554=DIRECTION('ref_axis',(1.22460635382238E-16,-1.,0.));
#8555=DIRECTION('center_axis',(-1.,-1.22460635382238E-16,0.));
#8556=DIRECTION('ref_axis',(1.22460635382238E-16,-1.,0.));
#8557=DIRECTION('',(0.57357643635105,-0.819152044288989,1.00317192905352E-16));
#8558=DIRECTION('center_axis',(-1.,-1.22460635382238E-16,0.));
#8559=DIRECTION('ref_axis',(1.22460635382238E-16,-1.,0.));
#8560=DIRECTION('center_axis',(-1.,-1.22460635382238E-16,0.));
#8561=DIRECTION('ref_axis',(1.22460635382238E-16,-1.,0.));
#8562=DIRECTION('center_axis',(1.,1.22460635382238E-16,0.));
#8563=DIRECTION('ref_axis',(-1.22460635382238E-16,1.,0.));
#8564=DIRECTION('',(-0.573576436351045,0.819152044288993,1.00317192905353E-16));
#8565=DIRECTION('center_axis',(1.,0.,0.));
#8566=DIRECTION('ref_axis',(0.,0.,-1.));
#8567=DIRECTION('center_axis',(1.,0.,0.));
#8568=DIRECTION('ref_axis',(0.,0.,-1.));
#8569=DIRECTION('center_axis',(1.,0.,0.));
#8570=DIRECTION('ref_axis',(0.,0.,-1.));
#8571=DIRECTION('center_axis',(0.,1.,1.22464679914735E-16));
#8572=DIRECTION('ref_axis',(0.,-1.22464679914735E-16,1.));
#8573=DIRECTION('center_axis',(-1.,0.,0.));
#8574=DIRECTION('ref_axis',(0.,0.,-1.));
#8575=DIRECTION('center_axis',(-1.,0.,0.));
#8576=DIRECTION('ref_axis',(0.,0.,1.));
#8577=DIRECTION('center_axis',(-1.,0.,0.));
#8578=DIRECTION('ref_axis',(0.,0.,1.));
#8579=DIRECTION('center_axis',(-1.,0.,0.));
#8580=DIRECTION('ref_axis',(0.,0.,1.));
#8581=DIRECTION('center_axis',(-1.,0.,0.));
#8582=DIRECTION('ref_axis',(0.,0.,1.));
#8583=DIRECTION('',(1.,0.,0.));
#8584=DIRECTION('center_axis',(1.,0.,0.));
#8585=DIRECTION('ref_axis',(0.,0.,-1.));
#8586=DIRECTION('center_axis',(-1.,0.,0.));
#8587=DIRECTION('ref_axis',(0.,0.,1.));
#8588=DIRECTION('center_axis',(-1.,0.,0.));
#8589=DIRECTION('ref_axis',(0.,0.,1.));
#8590=DIRECTION('center_axis',(-1.,0.,0.));
#8591=DIRECTION('ref_axis',(0.,0.,1.));
#8592=DIRECTION('center_axis',(-1.,0.,0.));
#8593=DIRECTION('ref_axis',(0.,0.,1.));
#8594=DIRECTION('',(1.,0.,0.));
#8595=DIRECTION('center_axis',(1.,0.,0.));
#8596=DIRECTION('ref_axis',(0.,0.,-1.));
#8597=DIRECTION('center_axis',(1.,0.,0.));
#8598=DIRECTION('ref_axis',(0.,0.,-1.));
#8599=DIRECTION('',(0.,0.500000000000001,0.866025403784438));
#8600=DIRECTION('',(0.,1.,1.35037086860206E-16));
#8601=DIRECTION('center_axis',(1.,0.,0.));
#8602=DIRECTION('ref_axis',(0.,0.,-1.));
#8603=DIRECTION('',(0.,0.500000000000001,0.866025403784438));
#8604=DIRECTION('',(0.,-0.500000000000001,0.866025403784438));
#8605=DIRECTION('center_axis',(1.,0.,0.));
#8606=DIRECTION('ref_axis',(0.,0.,-1.));
#8607=DIRECTION('',(0.,-0.500000000000001,0.866025403784438));
#8608=DIRECTION('',(0.,-1.,1.35037086860206E-16));
#8609=DIRECTION('center_axis',(1.,0.,0.));
#8610=DIRECTION('ref_axis',(0.,0.,-1.));
#8611=DIRECTION('',(0.,-1.,1.35037086860206E-16));
#8612=DIRECTION('',(0.,-0.500000000000002,-0.866025403784437));
#8613=DIRECTION('center_axis',(1.,0.,0.));
#8614=DIRECTION('ref_axis',(0.,0.,-1.));
#8615=DIRECTION('',(0.,-0.500000000000002,-0.866025403784437));
#8616=DIRECTION('',(0.,0.499999999999999,-0.866025403784439));
#8617=DIRECTION('center_axis',(1.,0.,0.));
#8618=DIRECTION('ref_axis',(0.,0.,-1.));
#8619=DIRECTION('',(0.,0.499999999999999,-0.866025403784439));
#8620=DIRECTION('',(0.,1.,1.35037086860206E-16));
#8621=DIRECTION('center_axis',(1.,0.,0.));
#8622=DIRECTION('ref_axis',(0.,0.,-1.));
#8623=DIRECTION('center_axis',(1.,0.,0.));
#8624=DIRECTION('ref_axis',(0.,0.,-1.));
#8625=DIRECTION('center_axis',(1.,0.,0.));
#8626=DIRECTION('ref_axis',(0.,0.,-1.));
#8627=DIRECTION('center_axis',(1.,0.,0.));
#8628=DIRECTION('ref_axis',(0.,0.,-1.));
#8629=DIRECTION('center_axis',(1.,0.,0.));
#8630=DIRECTION('ref_axis',(0.,0.,-1.));
#8631=DIRECTION('center_axis',(-1.,0.,0.));
#8632=DIRECTION('ref_axis',(0.,0.,1.));
#8633=DIRECTION('center_axis',(1.,0.,0.));
#8634=DIRECTION('ref_axis',(0.,0.,-1.));
#8635=DIRECTION('center_axis',(1.,0.,0.));
#8636=DIRECTION('ref_axis',(0.,0.,-1.));
#8637=DIRECTION('center_axis',(1.,0.,0.));
#8638=DIRECTION('ref_axis',(0.,0.,-1.));
#8639=DIRECTION('center_axis',(1.,0.,0.));
#8640=DIRECTION('ref_axis',(0.,0.,-1.));
#8641=DIRECTION('center_axis',(1.,0.,0.));
#8642=DIRECTION('ref_axis',(0.,0.,-1.));
#8643=DIRECTION('center_axis',(1.,0.,0.));
#8644=DIRECTION('ref_axis',(0.,0.,-1.));
#8645=DIRECTION('center_axis',(1.,0.,0.));
#8646=DIRECTION('ref_axis',(0.,0.,-1.));
#8647=DIRECTION('center_axis',(0.,-1.35037086860206E-16,1.));
#8648=DIRECTION('ref_axis',(0.,-1.,-1.35037086860206E-16));
#8649=DIRECTION('',(-1.,0.,0.));
#8650=DIRECTION('',(-1.,0.,0.));
#8651=DIRECTION('center_axis',(0.,0.866025403784439,0.499999999999999));
#8652=DIRECTION('ref_axis',(0.,-0.499999999999999,0.866025403784439));
#8653=DIRECTION('',(-1.,0.,0.));
#8654=DIRECTION('center_axis',(0.,0.866025403784438,-0.500000000000002));
#8655=DIRECTION('ref_axis',(0.,0.500000000000002,0.866025403784437));
#8656=DIRECTION('',(-1.,0.,0.));
#8657=DIRECTION('center_axis',(0.,-1.35037086860206E-16,-1.));
#8658=DIRECTION('ref_axis',(0.,1.,-1.35037086860206E-16));
#8659=DIRECTION('',(-1.,0.,0.));
#8660=DIRECTION('center_axis',(0.,-0.866025403784438,-0.500000000000001));
#8661=DIRECTION('ref_axis',(0.,0.500000000000001,-0.866025403784438));
#8662=DIRECTION('',(-1.,0.,0.));
#8663=DIRECTION('center_axis',(0.,-0.866025403784438,0.500000000000001));
#8664=DIRECTION('ref_axis',(0.,-0.500000000000001,-0.866025403784438));
#8665=DIRECTION('center_axis',(-1.,0.,0.));
#8666=DIRECTION('ref_axis',(0.,0.,1.));
#8667=DIRECTION('axis',(0.,0.,1.));
#8668=DIRECTION('refdir',(1.,0.,0.));
#8669=DIRECTION('center_axis',(1.,0.,0.));
#8670=DIRECTION('ref_axis',(0.,0.,-1.));
#8671=DIRECTION('center_axis',(1.,0.,0.));
#8672=DIRECTION('ref_axis',(0.,0.,-1.));
#8673=DIRECTION('',(1.,0.,0.));
#8674=DIRECTION('center_axis',(1.,0.,0.));
#8675=DIRECTION('ref_axis',(0.,0.,-1.));
#8676=DIRECTION('center_axis',(1.,0.,0.));
#8677=DIRECTION('ref_axis',(0.,0.,-1.));
#8678=DIRECTION('center_axis',(1.,0.,0.));
#8679=DIRECTION('ref_axis',(0.,0.,-1.));
#8680=DIRECTION('',(1.,0.,0.));
#8681=DIRECTION('center_axis',(1.,0.,0.));
#8682=DIRECTION('ref_axis',(0.,0.,-1.));
#8683=DIRECTION('',(1.,0.,0.));
#8684=DIRECTION('center_axis',(1.,0.,0.));
#8685=DIRECTION('ref_axis',(0.,0.,-1.));
#8686=DIRECTION('center_axis',(1.,0.,0.));
#8687=DIRECTION('ref_axis',(0.,0.,-1.));
#8688=DIRECTION('',(1.,0.,0.));
#8689=DIRECTION('center_axis',(1.,0.,0.));
#8690=DIRECTION('ref_axis',(0.,0.,-1.));
#8691=DIRECTION('center_axis',(0.866025403784438,0.,0.500000000000001));
#8692=DIRECTION('ref_axis',(0.500000000000001,0.,-0.866025403784438));
#8693=DIRECTION('',(0.500000000000001,1.82123199577618E-16,-0.866025403784438));
#8694=DIRECTION('',(0.,1.,0.));
#8695=DIRECTION('',(-0.500000000000001,-1.82123199577618E-16,0.866025403784438));
#8696=DIRECTION('',(0.,1.,0.));
#8697=DIRECTION('center_axis',(9.10615997888089E-17,-1.,-1.5772331745272E-16));
#8698=DIRECTION('ref_axis',(0.500000000000001,1.82123199577618E-16,-0.866025403784438));
#8699=DIRECTION('',(0.500000000000001,1.82123199577618E-16,-0.866025403784438));
#8700=DIRECTION('',(0.866025403784438,1.11518296706602E-32,0.500000000000001));
#8701=DIRECTION('',(0.866025403784438,1.11518296706602E-32,0.500000000000001));
#8702=DIRECTION('center_axis',(-9.10615997888089E-17,1.,1.5772331745272E-16));
#8703=DIRECTION('ref_axis',(-0.500000000000001,-1.82123199577618E-16,0.866025403784438));
#8704=DIRECTION('',(-0.866025403784438,-1.11518296706602E-32,-0.500000000000001));
#8705=DIRECTION('',(-0.500000000000001,-1.82123199577618E-16,0.866025403784438));
#8706=DIRECTION('',(-0.866025403784438,-1.11518296706602E-32,-0.500000000000001));
#8707=DIRECTION('center_axis',(0.866025403784438,0.,0.500000000000001));
#8708=DIRECTION('ref_axis',(0.500000000000001,0.,-0.866025403784438));
#8709=DIRECTION('',(0.,1.,0.));
#8710=DIRECTION('',(0.,1.,0.));
#8711=DIRECTION('center_axis',(1.,0.,0.));
#8712=DIRECTION('ref_axis',(0.,1.22464679914735E-16,1.));
#8713=DIRECTION('center_axis',(1.,0.,0.));
#8714=DIRECTION('ref_axis',(0.,0.,-1.));
#8715=DIRECTION('',(1.,0.,0.));
#8716=DIRECTION('center_axis',(1.,0.,0.));
#8717=DIRECTION('ref_axis',(0.,0.,-1.));
#8718=DIRECTION('',(1.,0.,0.));
#8719=DIRECTION('center_axis',(1.,0.,0.));
#8720=DIRECTION('ref_axis',(0.,0.,-1.));
#8721=DIRECTION('',(0.,1.,0.));
#8722=DIRECTION('',(0.,1.82123199577618E-16,-1.));
#8723=DIRECTION('',(0.,-1.82123199577618E-16,1.));
#8724=DIRECTION('center_axis',(0.,-1.,-1.82123199577617E-16));
#8725=DIRECTION('ref_axis',(0.,1.82123199577618E-16,-1.));
#8726=DIRECTION('',(1.,1.11518296706602E-32,-6.12323399573677E-17));
#8727=DIRECTION('',(0.,1.82123199577618E-16,-1.));
#8728=DIRECTION('center_axis',(1.,0.,0.));
#8729=DIRECTION('ref_axis',(0.,0.,-1.));
#8730=DIRECTION('',(0.,1.,0.));
#8731=DIRECTION('',(0.,-1.82123199577618E-16,1.));
#8732=DIRECTION('center_axis',(0.,1.,1.82123199577617E-16));
#8733=DIRECTION('ref_axis',(0.,-1.82123199577618E-16,1.));
#8734=DIRECTION('',(-1.,-1.11518296706602E-32,6.12323399573677E-17));
#8735=DIRECTION('center_axis',(0.,-1.,0.));
#8736=DIRECTION('ref_axis',(0.,0.,-1.));
#8737=DIRECTION('center_axis',(0.,1.,0.));
#8738=DIRECTION('ref_axis',(0.,0.,-1.));
#8739=DIRECTION('center_axis',(0.,1.,0.));
#8740=DIRECTION('ref_axis',(0.,0.,-1.));
#8741=DIRECTION('center_axis',(0.,1.,0.));
#8742=DIRECTION('ref_axis',(0.,0.,1.));
#8743=DIRECTION('center_axis',(0.,-1.,0.));
#8744=DIRECTION('ref_axis',(0.,0.,-1.));
#8745=DIRECTION('center_axis',(0.,-1.,0.));
#8746=DIRECTION('ref_axis',(0.,0.,1.));
#8747=DIRECTION('center_axis',(0.,-1.,0.));
#8748=DIRECTION('ref_axis',(0.,0.,-1.));
#8749=DIRECTION('center_axis',(0.,-1.,0.));
#8750=DIRECTION('ref_axis',(0.,0.,-1.));
#8751=DIRECTION('center_axis',(0.,1.,0.));
#8752=DIRECTION('ref_axis',(0.,0.,1.));
#8753=DIRECTION('',(1.,1.11518296706602E-32,0.));
#8754=DIRECTION('center_axis',(0.,-1.,0.));
#8755=DIRECTION('ref_axis',(0.,0.,-1.));
#8756=DIRECTION('center_axis',(0.,-1.,0.));
#8757=DIRECTION('ref_axis',(0.,0.,1.));
#8758=DIRECTION('center_axis',(0.,-1.,0.));
#8759=DIRECTION('ref_axis',(0.,0.,-1.));
#8760=DIRECTION('center_axis',(0.,1.,0.));
#8761=DIRECTION('ref_axis',(-3.54944407778959E-15,0.,-1.));
#8762=DIRECTION('',(-1.,-1.11518296706602E-32,0.));
#8763=DIRECTION('center_axis',(0.,1.,0.));
#8764=DIRECTION('ref_axis',(0.,0.,-1.));
#8765=DIRECTION('center_axis',(0.,-1.,0.));
#8766=DIRECTION('ref_axis',(0.,0.,-1.));
#8767=DIRECTION('',(0.,1.,0.));
#8768=DIRECTION('center_axis',(0.,-1.,0.));
#8769=DIRECTION('ref_axis',(0.,0.,-1.));
#8770=DIRECTION('',(0.,1.,0.));
#8771=DIRECTION('center_axis',(1.,0.,0.));
#8772=DIRECTION('ref_axis',(0.,0.,-1.));
#8773=DIRECTION('',(0.,1.82123199577618E-16,-1.));
#8774=DIRECTION('',(0.,-1.82123199577618E-16,1.));
#8775=DIRECTION('center_axis',(0.,1.,1.82123199577617E-16));
#8776=DIRECTION('ref_axis',(0.,-1.82123199577618E-16,1.));
#8777=DIRECTION('',(0.,-1.82123199577618E-16,1.));
#8778=DIRECTION('center_axis',(1.,0.,0.));
#8779=DIRECTION('ref_axis',(0.,0.,-1.));
#8780=DIRECTION('',(0.,1.82123199577618E-16,-1.));
#8781=DIRECTION('center_axis',(0.,-1.,-1.82123199577617E-16));
#8782=DIRECTION('ref_axis',(0.,1.82123199577618E-16,-1.));
#8783=DIRECTION('axis',(0.,0.,1.));
#8784=DIRECTION('refdir',(1.,0.,0.));
#8785=DIRECTION('center_axis',(0.,0.,1.));
#8786=DIRECTION('ref_axis',(1.,0.,0.));
#8787=DIRECTION('center_axis',(0.,0.,-1.));
#8788=DIRECTION('ref_axis',(1.,0.,0.));
#8789=DIRECTION('center_axis',(0.,0.,1.));
#8790=DIRECTION('ref_axis',(1.,0.,0.));
#8791=DIRECTION('center_axis',(1.,0.,0.));
#8792=DIRECTION('ref_axis',(0.,0.,-1.));
#8793=DIRECTION('center_axis',(0.,0.,1.));
#8794=DIRECTION('ref_axis',(1.,0.,0.));
#8795=DIRECTION('center_axis',(0.,0.,-1.));
#8796=DIRECTION('ref_axis',(1.,0.,0.));
#8797=DIRECTION('center_axis',(0.406935888454085,-0.913456721847338,0.));
#8798=DIRECTION('ref_axis',(0.913456721847338,0.406935888454085,0.));
#8799=DIRECTION('center_axis',(0.,0.,1.));
#8800=DIRECTION('ref_axis',(1.,0.,0.));
#8801=DIRECTION('center_axis',(-1.,0.,0.));
#8802=DIRECTION('ref_axis',(0.,0.,1.));
#8803=DIRECTION('center_axis',(0.,0.,1.));
#8804=DIRECTION('ref_axis',(1.,0.,0.));
#8805=DIRECTION('center_axis',(0.,0.,-1.));
#8806=DIRECTION('ref_axis',(1.,0.,0.));
#8807=DIRECTION('center_axis',(0.,0.,1.));
#8808=DIRECTION('ref_axis',(1.,0.,0.));
#8809=DIRECTION('center_axis',(1.,0.,0.));
#8810=DIRECTION('ref_axis',(0.,0.,-1.));
#8811=DIRECTION('center_axis',(0.,0.,1.));
#8812=DIRECTION('ref_axis',(1.,0.,0.));
#8813=DIRECTION('center_axis',(0.,0.,-1.));
#8814=DIRECTION('ref_axis',(1.,0.,0.));
#8815=DIRECTION('center_axis',(0.406935888454085,-0.913456721847338,0.));
#8816=DIRECTION('ref_axis',(0.913456721847338,0.406935888454085,0.));
#8817=DIRECTION('center_axis',(0.,0.,1.));
#8818=DIRECTION('ref_axis',(1.,0.,0.));
#8819=DIRECTION('center_axis',(-1.,0.,0.));
#8820=DIRECTION('ref_axis',(0.,0.,1.));
#8821=DIRECTION('center_axis',(0.,0.,1.));
#8822=DIRECTION('ref_axis',(1.,0.,0.));
#8823=DIRECTION('center_axis',(0.,0.,1.));
#8824=DIRECTION('ref_axis',(1.,0.,0.));
#8825=DIRECTION('center_axis',(0.,0.,1.));
#8826=DIRECTION('ref_axis',(1.,0.,0.));
#8827=DIRECTION('',(-0.707106781186539,-8.65956056235483E-17,0.707106781186556));
#8828=DIRECTION('center_axis',(0.,0.,-1.));
#8829=DIRECTION('ref_axis',(1.,0.,0.));
#8830=DIRECTION('center_axis',(0.,0.,-1.));
#8831=DIRECTION('ref_axis',(-1.,0.,0.));
#8832=DIRECTION('center_axis',(0.,0.,-1.));
#8833=DIRECTION('ref_axis',(1.,0.,0.));
#8834=DIRECTION('',(0.707106781186516,-8.65956056235455E-17,-0.707106781186578));
#8835=DIRECTION('center_axis',(0.,0.,1.));
#8836=DIRECTION('ref_axis',(1.,0.,0.));
#8837=DIRECTION('center_axis',(0.,0.,1.));
#8838=DIRECTION('ref_axis',(1.,0.,0.));
#8839=DIRECTION('center_axis',(0.,0.,1.));
#8840=DIRECTION('ref_axis',(1.,0.,0.));
#8841=DIRECTION('center_axis',(0.,0.,1.));
#8842=DIRECTION('ref_axis',(1.,0.,0.));
#8843=DIRECTION('',(-0.707106781186539,-8.65956056235482E-17,0.707106781186556));
#8844=DIRECTION('center_axis',(0.,0.,-1.));
#8845=DIRECTION('ref_axis',(1.,0.,0.));
#8846=DIRECTION('center_axis',(0.,0.,-1.));
#8847=DIRECTION('ref_axis',(-1.,0.,0.));
#8848=DIRECTION('center_axis',(0.,0.,-1.));
#8849=DIRECTION('ref_axis',(1.,0.,0.));
#8850=DIRECTION('',(0.707106781186533,-8.65956056235476E-17,-0.707106781186561));
#8851=DIRECTION('center_axis',(0.,0.,1.));
#8852=DIRECTION('ref_axis',(1.,0.,0.));
#8853=DIRECTION('center_axis',(0.,0.,1.));
#8854=DIRECTION('ref_axis',(1.,0.,0.));
#8855=DIRECTION('center_axis',(0.,0.,1.));
#8856=DIRECTION('ref_axis',(1.,0.,0.));
#8857=DIRECTION('center_axis',(0.,0.,1.));
#8858=DIRECTION('ref_axis',(1.,0.,0.));
#8859=DIRECTION('',(-0.707106781186539,-8.65956056235482E-17,0.707106781186556));
#8860=DIRECTION('center_axis',(0.,0.,-1.));
#8861=DIRECTION('ref_axis',(1.,0.,0.));
#8862=DIRECTION('center_axis',(0.,0.,-1.));
#8863=DIRECTION('ref_axis',(-1.,0.,0.));
#8864=DIRECTION('center_axis',(0.,0.,-1.));
#8865=DIRECTION('ref_axis',(1.,0.,0.));
#8866=DIRECTION('',(0.707106781186539,-8.65956056235483E-17,-0.707106781186556));
#8867=DIRECTION('center_axis',(0.,0.,1.));
#8868=DIRECTION('ref_axis',(1.,0.,0.));
#8869=DIRECTION('center_axis',(0.,0.,1.));
#8870=DIRECTION('ref_axis',(1.,0.,0.));
#8871=DIRECTION('center_axis',(0.,0.,1.));
#8872=DIRECTION('ref_axis',(1.,0.,0.));
#8873=DIRECTION('center_axis',(0.,0.,1.));
#8874=DIRECTION('ref_axis',(1.,0.,0.));
#8875=DIRECTION('',(-0.707106781186538,-8.65956056235482E-17,0.707106781186557));
#8876=DIRECTION('center_axis',(0.,0.,-1.));
#8877=DIRECTION('ref_axis',(1.,0.,0.));
#8878=DIRECTION('center_axis',(0.,0.,-1.));
#8879=DIRECTION('ref_axis',(-1.,0.,0.));
#8880=DIRECTION('center_axis',(0.,0.,-1.));
#8881=DIRECTION('ref_axis',(1.,0.,0.));
#8882=DIRECTION('',(0.707106781186538,-8.65956056235482E-17,-0.707106781186557));
#8883=DIRECTION('center_axis',(0.,0.,1.));
#8884=DIRECTION('ref_axis',(1.,0.,0.));
#8885=DIRECTION('center_axis',(0.,0.,1.));
#8886=DIRECTION('ref_axis',(1.,0.,0.));
#8887=DIRECTION('center_axis',(0.,0.,1.));
#8888=DIRECTION('ref_axis',(1.,0.,0.));
#8889=DIRECTION('center_axis',(0.,0.,1.));
#8890=DIRECTION('ref_axis',(1.,0.,0.));
#8891=DIRECTION('',(-0.707106781186538,-8.65956056235482E-17,0.707106781186557));
#8892=DIRECTION('center_axis',(0.,0.,-1.));
#8893=DIRECTION('ref_axis',(1.,0.,0.));
#8894=DIRECTION('center_axis',(0.,0.,-1.));
#8895=DIRECTION('ref_axis',(-1.,0.,0.));
#8896=DIRECTION('center_axis',(0.,0.,-1.));
#8897=DIRECTION('ref_axis',(1.,0.,0.));
#8898=DIRECTION('',(0.707106781186558,-8.65956056235506E-17,-0.707106781186537));
#8899=DIRECTION('center_axis',(0.,0.,1.));
#8900=DIRECTION('ref_axis',(1.,0.,0.));
#8901=DIRECTION('center_axis',(0.,0.,-1.));
#8902=DIRECTION('ref_axis',(-1.,0.,0.));
#8903=DIRECTION('',(0.,0.,-1.));
#8904=DIRECTION('center_axis',(0.,0.,-1.));
#8905=DIRECTION('ref_axis',(-1.,0.,0.));
#8906=DIRECTION('',(0.,0.,-1.));
#8907=DIRECTION('center_axis',(0.,0.,-1.));
#8908=DIRECTION('ref_axis',(-1.,0.,0.));
#8909=DIRECTION('',(0.,0.,-1.));
#8910=DIRECTION('center_axis',(0.,0.,-1.));
#8911=DIRECTION('ref_axis',(-1.,0.,0.));
#8912=DIRECTION('',(0.,0.,-1.));
#8913=DIRECTION('center_axis',(0.,0.,-1.));
#8914=DIRECTION('ref_axis',(-1.,0.,0.));
#8915=DIRECTION('',(0.,0.,-1.));
#8916=DIRECTION('center_axis',(0.,0.,-1.));
#8917=DIRECTION('ref_axis',(-1.,0.,0.));
#8918=DIRECTION('center_axis',(0.,0.,-1.));
#8919=DIRECTION('ref_axis',(1.,1.04083408558608E-14,0.));
#8920=DIRECTION('',(0.,0.,-1.));
#8921=DIRECTION('center_axis',(0.,0.,1.));
#8922=DIRECTION('ref_axis',(1.,0.,0.));
#8923=DIRECTION('',(0.,0.,-1.));
#8924=DIRECTION('center_axis',(0.,0.,-1.));
#8925=DIRECTION('ref_axis',(-1.,0.,0.));
#8926=DIRECTION('center_axis',(0.,0.,-1.));
#8927=DIRECTION('ref_axis',(1.,0.,0.));
#8928=DIRECTION('',(0.,0.,-1.));
#8929=DIRECTION('center_axis',(0.,0.,1.));
#8930=DIRECTION('ref_axis',(1.,0.,0.));
#8931=DIRECTION('',(0.,0.,-1.));
#8932=DIRECTION('center_axis',(0.,0.,1.));
#8933=DIRECTION('ref_axis',(1.,0.,0.));
#8934=DIRECTION('',(0.370256409888397,-0.928929594176305,0.));
#8935=DIRECTION('',(-1.,-1.28820497806328E-16,0.));
#8936=DIRECTION('center_axis',(0.,0.,1.));
#8937=DIRECTION('ref_axis',(1.,0.,0.));
#8938=DIRECTION('',(1.,-8.88417226250542E-18,0.));
#8939=DIRECTION('center_axis',(0.,0.,1.));
#8940=DIRECTION('ref_axis',(1.,0.,0.));
#8941=DIRECTION('',(-0.866025403784438,-0.500000000000001,0.));
#8942=DIRECTION('center_axis',(0.,0.,1.));
#8943=DIRECTION('ref_axis',(1.,0.,0.));
#8944=DIRECTION('center_axis',(0.,0.,1.));
#8945=DIRECTION('ref_axis',(1.,0.,0.));
#8946=DIRECTION('',(1.,1.28820497806328E-16,0.));
#8947=DIRECTION('',(-0.370256409888397,0.928929594176305,0.));
#8948=DIRECTION('center_axis',(0.,0.,-1.));
#8949=DIRECTION('ref_axis',(1.,4.16333634234433E-15,0.));
#8950=DIRECTION('',(0.866025403784438,0.500000000000001,0.));
#8951=DIRECTION('center_axis',(0.,0.,-1.));
#8952=DIRECTION('ref_axis',(1.,0.,0.));
#8953=DIRECTION('',(-1.,8.88417226250542E-18,0.));
#8954=DIRECTION('center_axis',(0.,0.,-1.));
#8955=DIRECTION('ref_axis',(1.,0.,0.));
#8956=DIRECTION('center_axis',(8.88417226250541E-18,1.,0.));
#8957=DIRECTION('ref_axis',(-1.,8.88417226250541E-18,0.));
#8958=DIRECTION('',(0.,0.,-1.));
#8959=DIRECTION('',(-1.,8.88417226250542E-18,0.));
#8960=DIRECTION('',(1.,-8.88417226250542E-18,0.));
#8961=DIRECTION('center_axis',(0.,0.,-1.));
#8962=DIRECTION('ref_axis',(0.838729959061342,-0.544547569798048,0.));
#8963=DIRECTION('',(0.,0.,-1.));
#8964=DIRECTION('center_axis',(0.,0.,-1.));
#8965=DIRECTION('ref_axis',(-1.,0.,0.));
#8966=DIRECTION('center_axis',(0.,0.,1.));
#8967=DIRECTION('ref_axis',(1.,0.,0.));
#8968=DIRECTION('',(0.,0.,-1.));
#8969=DIRECTION('center_axis',(0.,0.,-1.));
#8970=DIRECTION('ref_axis',(1.,-2.31296463463574E-15,0.));
#8971=DIRECTION('center_axis',(0.500000000000001,-0.866025403784438,0.));
#8972=DIRECTION('ref_axis',(0.866025403784438,0.500000000000001,0.));
#8973=DIRECTION('',(-0.866025403784438,-0.500000000000001,0.));
#8974=DIRECTION('',(0.866025403784438,0.500000000000001,0.));
#8975=DIRECTION('center_axis',(0.928929594176305,0.370256409888397,0.));
#8976=DIRECTION('ref_axis',(-0.370256409888397,0.928929594176305,0.));
#8977=DIRECTION('',(0.370256409888397,-0.928929594176305,0.));
#8978=DIRECTION('',(0.,0.,-1.));
#8979=DIRECTION('',(-0.370256409888397,0.928929594176305,0.));
#8980=DIRECTION('center_axis',(0.,0.,-1.));
#8981=DIRECTION('ref_axis',(0.712771275806866,-0.701396541468984,0.));
#8982=DIRECTION('',(0.,0.,-1.));
#8983=DIRECTION('center_axis',(1.28820497806328E-16,-1.,0.));
#8984=DIRECTION('ref_axis',(1.,1.28820497806328E-16,0.));
#8985=DIRECTION('',(-1.,-1.28820497806328E-16,0.));
#8986=DIRECTION('',(1.,1.28820497806328E-16,0.));
#8987=DIRECTION('center_axis',(0.,0.,1.));
#8988=DIRECTION('ref_axis',(1.,0.,0.));
#8989=DIRECTION('center_axis',(-0.866025403784439,-0.499999999999999,0.));
#8990=DIRECTION('ref_axis',(0.499999999999999,-0.86602540378444,0.));
#8991=DIRECTION('center_axis',(-0.866025403784438,-0.500000000000001,0.));
#8992=DIRECTION('ref_axis',(0.500000000000001,-0.866025403784438,0.));
#8993=DIRECTION('center_axis',(-0.866025403784439,-0.499999999999999,0.));
#8994=DIRECTION('ref_axis',(0.499999999999999,-0.86602540378444,0.));
#8995=DIRECTION('center_axis',(1.,-8.88417226250541E-18,0.));
#8996=DIRECTION('ref_axis',(8.88417226250541E-18,1.,0.));
#8997=DIRECTION('center_axis',(-1.,0.,0.));
#8998=DIRECTION('ref_axis',(0.,0.,1.));
#8999=DIRECTION('center_axis',(0.,0.,1.));
#9000=DIRECTION('ref_axis',(-0.944752944945269,0.327783271411525,0.));
#9001=DIRECTION('center_axis',(0.370256409888406,-0.928929594176302,0.));
#9002=DIRECTION('ref_axis',(0.928929594176302,0.370256409888406,0.));
#9003=DIRECTION('center_axis',(0.,0.,1.));
#9004=DIRECTION('ref_axis',(-1.,-1.18852590797403E-16,0.));
#9005=DIRECTION('center_axis',(1.,0.,0.));
#9006=DIRECTION('ref_axis',(0.,0.,-1.));
#9007=DIRECTION('center_axis',(0.370256409888397,-0.928929594176305,0.));
#9008=DIRECTION('ref_axis',(0.928929594176305,0.370256409888397,0.));
#9009=DIRECTION('center_axis',(-1.,-1.28820497806328E-16,0.));
#9010=DIRECTION('ref_axis',(1.28820497806329E-16,-1.,0.));
#9011=DIRECTION('center_axis',(0.,0.,1.));
#9012=DIRECTION('ref_axis',(1.,0.,0.));
#9013=DIRECTION('center_axis',(-0.866025403784439,-0.499999999999999,0.));
#9014=DIRECTION('ref_axis',(0.499999999999999,-0.86602540378444,0.));
#9015=DIRECTION('center_axis',(0.866025403784438,0.500000000000001,0.));
#9016=DIRECTION('ref_axis',(-0.500000000000001,0.866025403784438,0.));
#9017=DIRECTION('center_axis',(-0.866025403784443,-0.499999999999993,0.));
#9018=DIRECTION('ref_axis',(0.499999999999993,-0.866025403784443,0.));
#9019=DIRECTION('center_axis',(-1.,8.88417226250541E-18,0.));
#9020=DIRECTION('ref_axis',(-8.88417226250541E-18,-1.,0.));
#9021=DIRECTION('center_axis',(-1.,0.,0.));
#9022=DIRECTION('ref_axis',(0.,0.,1.));
#9023=DIRECTION('center_axis',(0.,0.,1.));
#9024=DIRECTION('ref_axis',(-0.944752944945269,0.327783271411525,0.));
#9025=DIRECTION('center_axis',(0.3702564098884,-0.928929594176304,0.));
#9026=DIRECTION('ref_axis',(0.928929594176304,0.3702564098884,0.));
#9027=DIRECTION('center_axis',(0.,0.,1.));
#9028=DIRECTION('ref_axis',(-1.,-1.18852590797403E-16,0.));
#9029=DIRECTION('center_axis',(1.,0.,0.));
#9030=DIRECTION('ref_axis',(0.,0.,-1.));
#9031=DIRECTION('center_axis',(-0.370256409888397,0.928929594176305,0.));
#9032=DIRECTION('ref_axis',(-0.928929594176305,-0.370256409888397,0.));
#9033=DIRECTION('center_axis',(1.,1.28820497806328E-16,0.));
#9034=DIRECTION('ref_axis',(-1.28820497806328E-16,1.,0.));
#9035=DIRECTION('',(-0.288863932057661,0.293145135121242,-0.911385515855357));
#9036=DIRECTION('',(0.94596773123939,-0.0590907808125063,-0.318831195269174));
#9037=DIRECTION('',(0.945967731239389,-0.0590907808125063,-0.318831195269176));
#9038=DIRECTION('',(-0.110972873933173,-0.982877794415124,-0.147092700351421));
#9039=DIRECTION('',(-0.196103813305551,0.0346370212714953,0.979971209354877));
#9040=DIRECTION('',(0.979088859150446,-0.0482344628624278,0.197632088689693));
#9041=DIRECTION('',(0.173660521921563,-0.0335248278525656,-0.984234783495984));
#9042=DIRECTION('',(-0.983317712050094,0.0490140037912104,-0.175168218010358));
#9043=DIRECTION('',(0.945967731239389,-0.0590907808125067,-0.318831195269175));
#9044=DIRECTION('',(0.0996380178535381,0.988655868265101,0.112391456718019));
#9045=DIRECTION('',(-0.173660521921563,0.0335248278525656,0.984234783495984));
#9046=DIRECTION('',(0.984801205419384,0.0029340978953859,0.173660521921563));
#9047=DIRECTION('',(0.316395818115763,-0.0470402576329403,0.947460236865212));
#9048=DIRECTION('',(0.945967731239389,-0.0590907808125065,-0.318831195269175));
#9049=DIRECTION('',(0.945967731239389,-0.0590907808125064,-0.318831195269175));
#9050=DIRECTION('',(-0.189819322531999,0.696262423980742,-0.692233531220465));
#9051=DIRECTION('',(-0.288863932057666,0.293145135121222,-0.911385515855362));
#9052=DIRECTION('',(-0.945967731239389,0.0590907808125066,0.318831195269177));
#9053=DIRECTION('',(-0.945967731239389,0.0590907808125067,0.318831195269175));
#9054=DIRECTION('',(-0.321109902237676,-0.0339718444538309,-0.94643242995436));
#9055=DIRECTION('',(0.950407030315111,0.252731356840593,0.181254897856928));
#9056=DIRECTION('',(0.196103813305564,-0.0346370212714964,-0.979971209354874));
#9057=DIRECTION('',(-0.612957084999054,0.350388394409024,0.708174826587989));
#9058=DIRECTION('',(0.749863917933823,-0.0244537595410115,0.661140014085705));
#9059=DIRECTION('',(-0.196103813305565,0.0346370212714964,0.979971209354874));
#9060=DIRECTION('',(-0.0875956400643035,0.9947617319281,-0.0526887135270094));
#9061=DIRECTION('',(-0.749863917933823,0.0244537595410113,-0.661140014085707));
#9062=DIRECTION('',(0.148603214629521,0.980007344130335,-0.13229773260483));
#9063=DIRECTION('',(-0.196103813305565,0.0346370212714967,0.979971209354874));
#9064=DIRECTION('',(0.73555501658121,0.666085106426314,0.123650509822088));
#9065=DIRECTION('',(-0.749863917933822,0.0244537595410116,-0.661140014085706));
#9066=DIRECTION('',(-0.431822481098737,0.739006460467091,0.51710617498308));
#9067=DIRECTION('',(0.196103813305565,-0.0346370212714964,-0.979971209354874));
#9068=DIRECTION('',(0.977178000281899,-0.0763102200229555,0.198242039146891));
#9069=DIRECTION('',(0.749863917933823,-0.0244537595410113,0.661140014085707));
#9070=DIRECTION('',(-0.660637118261209,0.0259974708054006,0.750255109604224));
#9071=DIRECTION('',(-0.980580802095762,-0.00474464419903071,-0.196058100859559));
#9072=DIRECTION('',(-0.196103813305566,0.0346370212714966,0.979971209354874));
#9073=DIRECTION('',(0.655580108636711,-0.106949003351338,-0.747513633214828));
#9074=DIRECTION('',(-0.749863917933822,0.0244537595410114,-0.661140014085707));
#9075=DIRECTION('',(0.950407030315105,0.252731356840614,0.181254897856928));
#9076=DIRECTION('',(-0.196103813305566,0.0346370212714969,0.979971209354873));
#9077=DIRECTION('',(-0.61295708499905,0.350388394409044,0.708174826587983));
#9078=DIRECTION('',(-0.749863917933822,0.0244537595410117,-0.661140014085707));
#9079=DIRECTION('',(-0.196103813305564,0.0346370212714968,0.979971209354874));
#9080=DIRECTION('',(0.123627102033092,-0.990528317747962,0.059749404869769));
#9081=DIRECTION('',(-0.749863917933823,0.0244537595410118,-0.661140014085706));
#9082=DIRECTION('',(-0.172325272399209,-0.972041369080477,0.159497891173177));
#9083=CARTESIAN_POINT('',(0.,0.,0.));
#9084=CARTESIAN_POINT('',(0.,0.,0.));
#9085=CARTESIAN_POINT('Origin',(0.,-25.4,0.));
#9086=CARTESIAN_POINT('',(-8.53327934765894E-14,19.7627746953453,-8.326));
#9087=CARTESIAN_POINT('',(1.31190385833674E-13,20.1637230794129,-8.326));
#9088=CARTESIAN_POINT('',(-1.01964092497009E-15,-25.4,-8.326));
#9089=CARTESIAN_POINT('',(1.15457232288591,22.22,-8.24555872886889));
#9090=CARTESIAN_POINT('Ctrl Pts',(2.9393154576951E-13,20.1637230794129,
-8.326));
#9091=CARTESIAN_POINT('Ctrl Pts',(-0.708200717931855,20.1895051998125,-8.326));
#9092=CARTESIAN_POINT('Ctrl Pts',(-1.41494612036022,20.2171332728378,-8.23565416784787));
#9093=CARTESIAN_POINT('Ctrl Pts',(-3.16729826485032,20.2905430311874,-7.77819055474686));
#9094=CARTESIAN_POINT('Ctrl Pts',(-4.16596846789998,20.3371138773749,-7.29223028439277));
#9095=CARTESIAN_POINT('Ctrl Pts',(-5.88380050089614,20.4271213329289,-5.98530507331128));
#9096=CARTESIAN_POINT('Ctrl Pts',(-6.59647033054524,20.4697946579353,-5.1894105472544));
#9097=CARTESIAN_POINT('Ctrl Pts',(-7.70794823763998,20.5492238742483,-3.33553158228336));
#9098=CARTESIAN_POINT('Ctrl Pts',(-8.08157861678374,20.5926134393248,-2.28631103821033));
#9099=CARTESIAN_POINT('Ctrl Pts',(-8.39575024460199,20.6837076506364,-0.119309885693965));
#9100=CARTESIAN_POINT('Ctrl Pts',(-8.33966207607041,20.7297596899249,0.976202340350647));
#9101=CARTESIAN_POINT('Ctrl Pts',(-7.81768239149004,20.8170405939904,3.05249036106223));
#9102=CARTESIAN_POINT('Ctrl Pts',(-7.36879696098183,20.8548878518499,4.01677584313272));
#9103=CARTESIAN_POINT('Ctrl Pts',(-6.10637108416454,20.9376219601132,5.76644257170316));
#9104=CARTESIAN_POINT('Ctrl Pts',(-5.28937860377834,20.9832860564796,6.52393732253735));
#9105=CARTESIAN_POINT('Ctrl Pts',(-3.43256215082987,21.0747868850767,7.66118487941332));
#9106=CARTESIAN_POINT('Ctrl Pts',(-2.41646683206916,21.1197342681174,8.03972422596952));
#9107=CARTESIAN_POINT('Ctrl Pts',(-0.30103886964946,21.2040887303464,8.38903981540581));
#9108=CARTESIAN_POINT('Ctrl Pts',(0.77805047538717,21.2413690487989,8.35830671932943));
#9109=CARTESIAN_POINT('Ctrl Pts',(2.89883696890837,21.3285727435666,7.88271403447874));
#9110=CARTESIAN_POINT('Ctrl Pts',(3.91705889205637,21.3751678727251,7.42946302233154));
#9111=CARTESIAN_POINT('Ctrl Pts',(5.68342520927749,21.4658085523941,6.17647466325817));
#9112=CARTESIAN_POINT('Ctrl Pts',(6.42420250024152,21.5090577158337,5.40186694088489));
#9113=CARTESIAN_POINT('Ctrl Pts',(7.59864239252401,21.5901331939427,3.57871690055576));
#9114=CARTESIAN_POINT('Ctrl Pts',(8.00651613636646,21.6320216270508,2.53827512105294));
#9115=CARTESIAN_POINT('Ctrl Pts',(8.38863518496435,21.722950323466,0.375211331472238));
#9116=CARTESIAN_POINT('Ctrl Pts',(8.36567998459492,21.7691937855692,-0.724854569873513));
#9117=CARTESIAN_POINT('Ctrl Pts',(7.90507099774516,21.8571908196599,-2.81817830084023));
#9118=CARTESIAN_POINT('Ctrl Pts',(7.48545823607019,21.8959733497179,-3.79471255741776));
#9119=CARTESIAN_POINT('Ctrl Pts',(6.27658819709621,21.9775203773607,-5.58066281390651));
#9120=CARTESIAN_POINT('Ctrl Pts',(5.48278798673984,22.0228461833929,-6.36223286723487));
#9121=CARTESIAN_POINT('Ctrl Pts',(4.04328783254457,22.0950557765146,-7.30447159027245));
#9122=CARTESIAN_POINT('Ctrl Pts',(3.49067741606164,22.1210511178399,-7.58410633998801));
#9123=CARTESIAN_POINT('Ctrl Pts',(2.34434684189784,22.1717792313269,-8.01210224550795));
#9124=CARTESIAN_POINT('Ctrl Pts',(1.75496663665873,22.1963755718445,-8.16148939163003));
#9125=CARTESIAN_POINT('Ctrl Pts',(1.15457232288581,22.22,-8.2455587288689));
#9126=CARTESIAN_POINT('',(-7.30706743901566,22.22,-3.99112032412919));
#9127=CARTESIAN_POINT('Origin',(0.,22.22,0.));
#9128=CARTESIAN_POINT('',(2.02140576001126E-13,21.8627746953453,-8.326));
#9129=CARTESIAN_POINT('Ctrl Pts',(-7.30706743901566,22.22,-3.99112032412919));
#9130=CARTESIAN_POINT('Ctrl Pts',(-6.80957791613765,22.1817118950886,-4.90193964267893));
#9131=CARTESIAN_POINT('Ctrl Pts',(-6.14607950438177,22.141467826149,-5.71189907139109));
#9132=CARTESIAN_POINT('Ctrl Pts',(-4.52911708821652,22.0540951363203,-7.06818095845697));
#9133=CARTESIAN_POINT('Ctrl Pts',(-3.58212247816543,22.0086069804025,-7.59213467174586));
#9134=CARTESIAN_POINT('Ctrl Pts',(-1.73288189728967,21.9287159657206,-8.19014224877633));
#9135=CARTESIAN_POINT('Ctrl Pts',(-0.868435929643723,21.8943901952037,-8.32600000000001));
#9136=CARTESIAN_POINT('Ctrl Pts',(3.16691117774326E-13,21.8627746953453,
-8.326));
#9137=CARTESIAN_POINT('',(-1.01964092497009E-15,24.9,-8.326));
#9138=CARTESIAN_POINT('',(-1.01964092497009E-15,-25.4,-8.326));
#9139=CARTESIAN_POINT('Origin',(0.,24.9,0.));
#9140=CARTESIAN_POINT('Ctrl Pts',(2.73392419813945E-13,21.8627746953453,
-8.326));
#9141=CARTESIAN_POINT('Ctrl Pts',(0.222420275737213,21.8546774621977,-8.326));
#9142=CARTESIAN_POINT('Ctrl Pts',(0.445088669140307,21.8463838731545,-8.31708769992091));
#9143=CARTESIAN_POINT('Ctrl Pts',(1.72956012537363,21.7974512311123,-8.21378222217217));
#9144=CARTESIAN_POINT('Ctrl Pts',(2.76535295574494,21.7536792163472,-7.92528063087028));
#9145=CARTESIAN_POINT('Ctrl Pts',(4.70935917599653,21.6625113677188,-6.9548924164029));
#9146=CARTESIAN_POINT('Ctrl Pts',(5.59165784984499,21.6159442735309,-6.26754925433765));
#9147=CARTESIAN_POINT('Ctrl Pts',(7.00684017904237,21.529824526478,-4.62138544212288));
#9148=CARTESIAN_POINT('Ctrl Pts',(7.53914569966282,21.4928809496688,-3.68975621000039));
#9149=CARTESIAN_POINT('Ctrl Pts',(8.2291331827155,21.4076770804388,-1.66287788083303));
#9150=CARTESIAN_POINT('Ctrl Pts',(8.37505267279169,21.3623615337414,-0.584885761396712));
#9151=CARTESIAN_POINT('Ctrl Pts',(8.24648416511102,21.2708521782396,1.59199107833957));
#9152=CARTESIAN_POINT('Ctrl Pts',(7.96327969214975,21.2255626695136,2.66936379163521));
#9153=CARTESIAN_POINT('Ctrl Pts',(7.0152084419188,21.144136245221,4.60638210209414));
#9154=CARTESIAN_POINT('Ctrl Pts',(6.37675301190161,21.1052415183809,5.45612438337728));
#9155=CARTESIAN_POINT('Ctrl Pts',(4.78959810321677,21.0171730787018,6.89713617786851));
#9156=CARTESIAN_POINT('Ctrl Pts',(3.84635314660346,20.9709125093812,7.46433370424951));
#9157=CARTESIAN_POINT('Ctrl Pts',(1.78044218858592,20.8800677193668,8.20820651339556));
#9158=CARTESIAN_POINT('Ctrl Pts',(0.676127188089457,20.8383517093461,8.37179460683603));
#9159=CARTESIAN_POINT('Ctrl Pts',(-1.48885324123266,20.7571943549324,8.26041566296981));
#9160=CARTESIAN_POINT('Ctrl Pts',(-2.52964769301862,20.7138984210511,8.00322770229722));
#9161=CARTESIAN_POINT('Ctrl Pts',(-4.49594281807084,20.6232085649402,7.09418652168197));
#9162=CARTESIAN_POINT('Ctrl Pts',(-5.39595620582177,20.5766138261025,6.43621089068518));
#9163=CARTESIAN_POINT('Ctrl Pts',(-6.86332004775605,20.4895022029757,4.83323748008094));
#9164=CARTESIAN_POINT('Ctrl Pts',(-7.4265465602687,20.4522662415181,3.9130188955332));
#9165=CARTESIAN_POINT('Ctrl Pts',(-8.17616169136161,20.3678381340514,1.9045948304856));
#9166=CARTESIAN_POINT('Ctrl Pts',(-8.35346386919154,20.3228574715675,0.834569128080672));
#9167=CARTESIAN_POINT('Ctrl Pts',(-8.29082102121212,20.2313519706046,-1.3422160176817));
#9168=CARTESIAN_POINT('Ctrl Pts',(-8.04024058237028,20.1857179501071,-2.42778417386124));
#9169=CARTESIAN_POINT('Ctrl Pts',(-7.15070000077872,20.1030946136455,-4.39327531494625));
#9170=CARTESIAN_POINT('Ctrl Pts',(-6.53768510268979,20.0651732446934,-5.26234377960467));
#9171=CARTESIAN_POINT('Ctrl Pts',(-4.99629403922793,19.9778244858738,-6.7483805201122));
#9172=CARTESIAN_POINT('Ctrl Pts',(-4.07364773146887,19.9317528080013,-7.34226903746486));
#9173=CARTESIAN_POINT('Ctrl Pts',(-2.0873033090925,19.8429221520908,-8.12812838292694));
#9174=CARTESIAN_POINT('Ctrl Pts',(-1.04801299029565,19.8009277166739,-8.32599999999998));
#9175=CARTESIAN_POINT('Ctrl Pts',(-1.4432899320127E-13,19.7627746953453,
-8.326));
#9176=CARTESIAN_POINT('Origin',(0.,-25.4,0.));
#9177=CARTESIAN_POINT('',(-5.25515247417893E-14,17.6627746953453,-8.326));
#9178=CARTESIAN_POINT('',(2.16625517025532E-13,18.0637230794129,-8.326));
#9179=CARTESIAN_POINT('',(-1.01964092497009E-15,-25.4,-8.326));
#9180=CARTESIAN_POINT('Ctrl Pts',(2.52020626589911E-13,18.0637230794129,
-8.326));
#9181=CARTESIAN_POINT('Ctrl Pts',(-0.890419891838311,18.0961389076892,-8.326));
#9182=CARTESIAN_POINT('Ctrl Pts',(-1.77639189334566,18.1313947631273,-8.1831756499706));
#9183=CARTESIAN_POINT('Ctrl Pts',(-3.66112836545653,18.2131638963057,-7.55729324801004));
#9184=CARTESIAN_POINT('Ctrl Pts',(-4.62037689809789,18.2595459254736,-7.01203601590485));
#9185=CARTESIAN_POINT('Ctrl Pts',(-6.24408054969564,18.3481770243168,-5.60755878566216));
#9186=CARTESIAN_POINT('Ctrl Pts',(-6.90299349539498,18.3880811030606,-4.77298598603335));
#9187=CARTESIAN_POINT('Ctrl Pts',(-7.89718765749648,18.46854217343,-2.85893206632874));
#9188=CARTESIAN_POINT('Ctrl Pts',(-8.20603261947695,18.5135288767537,-1.78876266097571));
#9189=CARTESIAN_POINT('Ctrl Pts',(-8.38685799405134,18.604981436681,0.386763093180027));
#9190=CARTESIAN_POINT('Ctrl Pts',(-8.26601443080375,18.6505352226678,1.47042258496924));
#9191=CARTESIAN_POINT('Ctrl Pts',(-7.62326100457352,18.7363397578568,3.51158989920655));
#9192=CARTESIAN_POINT('Ctrl Pts',(-7.11494212544351,18.7732834184323,4.45229486945681));
#9193=CARTESIAN_POINT('Ctrl Pts',(-5.7408036723115,18.8586081423939,6.13172383316992));
#9194=CARTESIAN_POINT('Ctrl Pts',(-4.87297955135116,18.9051237215524,6.84168671833937));
#9195=CARTESIAN_POINT('Ctrl Pts',(-2.94767213755927,18.9966100831954,7.85961615483011));
#9196=CARTESIAN_POINT('Ctrl Pts',(-1.91643098526058,19.0407291195881,8.17251178137013));
#9197=CARTESIAN_POINT('Ctrl Pts',(0.226566935638505,19.1233906949082,8.39353207965677));
#9198=CARTESIAN_POINT('Ctrl Pts',(1.31869908885409,19.1624366089017,8.29240327023542));
#9199=CARTESIAN_POINT('Ctrl Pts',(3.41208572998068,19.2516557666824,7.67346267722576));
#9200=CARTESIAN_POINT('Ctrl Pts',(4.39178998104064,19.2981569649045,7.15796606561161));
#9201=CARTESIAN_POINT('Ctrl Pts',(6.06368536035962,19.387512273397,5.80250353034279));
#9202=CARTESIAN_POINT('Ctrl Pts',(6.74982179139679,19.4290584529639,4.98762194233357));
#9203=CARTESIAN_POINT('Ctrl Pts',(7.8040409043102,19.5082348491522,3.10412858614996));
#9204=CARTESIAN_POINT('Ctrl Pts',(8.14610250630801,19.5527862684777,2.04431396528135));
#9205=CARTESIAN_POINT('Ctrl Pts',(8.39522393183261,19.6440847731824,-0.127547035208562));
#9206=CARTESIAN_POINT('Ctrl Pts',(8.30742204212602,19.6899135850502,-1.21774899981201));
#9207=CARTESIAN_POINT('Ctrl Pts',(7.72647180284449,19.7764844822775,-3.27714697213884));
#9208=CARTESIAN_POINT('Ctrl Pts',(7.24888972111259,19.8137313904644,-4.22984071149828));
#9209=CARTESIAN_POINT('Ctrl Pts',(5.92803207045448,19.898005531026,-5.9515709756581));
#9210=CARTESIAN_POINT('Ctrl Pts',(5.079672161943,19.9444159902647,-6.69024556027974));
#9211=CARTESIAN_POINT('Ctrl Pts',(3.1801110567652,20.0362414234368,-7.7689009659777));
#9212=CARTESIAN_POINT('Ctrl Pts',(2.15556595890407,20.0807750999972,-8.11312189350259));
#9213=CARTESIAN_POINT('Ctrl Pts',(0.730483570767718,20.1366251233243,-8.30199133068642));
#9214=CARTESIAN_POINT('Ctrl Pts',(0.365066982180118,20.1504327781605,-8.326));
#9215=CARTESIAN_POINT('Ctrl Pts',(2.43693953905222E-13,20.1637230794129,
-8.326));
#9216=CARTESIAN_POINT('Ctrl Pts',(-1.69645946028209E-13,19.7627746953453,
-8.326));
#9217=CARTESIAN_POINT('Ctrl Pts',(0.0537760328361958,19.7608169733068,-8.32600000000001));
#9218=CARTESIAN_POINT('Ctrl Pts',(0.107574246419283,19.7588474932951,-8.32547900742368));
#9219=CARTESIAN_POINT('Ctrl Pts',(1.22032386865729,19.717884294939,-8.30390594916758));
#9220=CARTESIAN_POINT('Ctrl Pts',(2.26557642210438,19.675157325493,-8.08150934929497));
#9221=CARTESIAN_POINT('Ctrl Pts',(4.25439689276674,19.5850888690087,-7.24104763054406));
#9222=CARTESIAN_POINT('Ctrl Pts',(5.17296265458766,19.5385136547805,-6.61613457917031));
#9223=CARTESIAN_POINT('Ctrl Pts',(6.69769916516932,19.4503382758645,-5.06192308448468));
#9224=CARTESIAN_POINT('Ctrl Pts',(7.29556680177744,19.4124020752022,-4.15413589911575));
#9225=CARTESIAN_POINT('Ctrl Pts',(8.11027653410421,19.3288434821876,-2.16639634071711));
#9226=CARTESIAN_POINT('Ctrl Pts',(8.32142803602603,19.2842710064197,-1.10608081716402));
#9227=CARTESIAN_POINT('Ctrl Pts',(8.33060510978089,19.1924165715265,1.07900496832259));
#9228=CARTESIAN_POINT('Ctrl Pts',(8.11166964648995,19.1460188118018,2.18274138966102));
#9229=CARTESIAN_POINT('Ctrl Pts',(7.27482662402643,19.0618495981043,4.18500674179216));
#9230=CARTESIAN_POINT('Ctrl Pts',(6.68601371437469,19.0245541532904,5.07293964281488));
#9231=CARTESIAN_POINT('Ctrl Pts',(5.18838404047147,18.9379083407741,6.60132915675086));
#9232=CARTESIAN_POINT('Ctrl Pts',(4.28597903871517,18.8920544918981,7.21991296322557));
#9233=CARTESIAN_POINT('Ctrl Pts',(2.27756009335754,18.8007762125735,8.08398904216306));
#9234=CARTESIAN_POINT('Ctrl Pts',(1.18800422662706,18.7562704237527,8.3142811960007));
#9235=CARTESIAN_POINT('Ctrl Pts',(-0.970574421465393,18.6772229603539,8.33636576399424));
#9236=CARTESIAN_POINT('Ctrl Pts',(-2.01903107640799,18.6354936260255,8.14625193122687));
#9237=CARTESIAN_POINT('Ctrl Pts',(-4.02696397192928,18.5460671966126,7.36943971707767));
#9238=CARTESIAN_POINT('Ctrl Pts',(-4.96163230319053,18.4995567041815,6.77549641229619));
#9239=CARTESIAN_POINT('Ctrl Pts',(-6.53890596645596,18.4104340420465,5.26721290630533));
#9240=CARTESIAN_POINT('Ctrl Pts',(-7.16916082099009,18.3715093575615,4.37078513603769));
#9241=CARTESIAN_POINT('Ctrl Pts',(-8.04313227967416,18.2887628323817,2.40236351133255));
#9242=CARTESIAN_POINT('Ctrl Pts',(-8.28466633463081,18.2445995564128,1.35178226642655));
#9243=CARTESIAN_POINT('Ctrl Pts',(-8.35906795948745,18.1530746958544,-0.825463416455813));
#9244=CARTESIAN_POINT('Ctrl Pts',(-8.17458512402766,18.1065678943966,-1.93179378485013));
#9245=CARTESIAN_POINT('Ctrl Pts',(-7.40071930074816,18.0213496277566,-3.95901460783598));
#9246=CARTESIAN_POINT('Ctrl Pts',(-6.83757202508643,17.9843906714201,-4.86745290900539));
#9247=CARTESIAN_POINT('Ctrl Pts',(-5.38647179191651,17.898507096619,-6.44016868567395));
#9248=CARTESIAN_POINT('Ctrl Pts',(-4.50612444658721,17.8529234024623,-7.0841042841063));
#9249=CARTESIAN_POINT('Ctrl Pts',(-2.52840988388469,17.7614823987188,-8.00910387674011));
#9250=CARTESIAN_POINT('Ctrl Pts',(-1.44636514008738,17.7165379978424,-8.27327358554525));
#9251=CARTESIAN_POINT('Ctrl Pts',(-0.229460356638047,17.6711780304915,-8.32363031929139));
#9252=CARTESIAN_POINT('Ctrl Pts',(-0.114688347109808,17.6669499364864,-8.326));
#9253=CARTESIAN_POINT('Ctrl Pts',(-9.72832925327793E-14,17.6627746953453,
-8.326));
#9254=CARTESIAN_POINT('Origin',(0.,-25.4,0.));
#9255=CARTESIAN_POINT('',(-1.73496445486892E-13,15.5627746953453,-8.326));
#9256=CARTESIAN_POINT('',(-8.53327934765894E-14,15.9637230794129,-8.326));
#9257=CARTESIAN_POINT('',(-1.01964092497009E-15,-25.4,-8.326));
#9258=CARTESIAN_POINT('Ctrl Pts',(-1.01030295240889E-13,15.9637230794129,
-8.326));
#9259=CARTESIAN_POINT('Ctrl Pts',(-1.06766019611996,16.0025913593021,-8.32599999999998));
#9260=CARTESIAN_POINT('Ctrl Pts',(-2.12593713442031,16.0454344607786,-8.12063706622244));
#9261=CARTESIAN_POINT('Ctrl Pts',(-4.12404446198688,16.1351306644149,-7.31397138239622));
#9262=CARTESIAN_POINT('Ctrl Pts',(-5.04197560981409,16.1811543292689,-6.7142002907157));
#9263=CARTESIAN_POINT('Ctrl Pts',(-6.57307250804579,16.268338992533,-5.21814073069542));
#9264=CARTESIAN_POINT('Ctrl Pts',(-7.18038549971979,16.3060862262824,-4.34466982618623));
#9265=CARTESIAN_POINT('Ctrl Pts',(-8.05663598620786,16.3889768494034,-2.37282031731172));
#9266=CARTESIAN_POINT('Ctrl Pts',(-8.29980195235844,16.4346829044047,-1.28553856319385));
#9267=CARTESIAN_POINT('Ctrl Pts',(-8.34754816142187,16.5261758537262,0.89094799695044));
#9268=CARTESIAN_POINT('Ctrl Pts',(-8.16319350057409,16.5710755391503,1.95904737078116));
#9269=CARTESIAN_POINT('Ctrl Pts',(-7.40008811787804,16.6553253882446,3.96323092380682));
#9270=CARTESIAN_POINT('Ctrl Pts',(-6.82976049081476,16.6926735547414,4.88087307410312));
#9271=CARTESIAN_POINT('Ctrl Pts',(-5.35053928533847,16.7800074091779,6.47388205937465));
#9272=CARTESIAN_POINT('Ctrl Pts',(-4.4466108738051,16.8266024358327,7.12509036378162));
#9273=CARTESIAN_POINT('Ctrl Pts',(-2.47548792401173,16.9171721477538,8.02005338937477));
#9274=CARTESIAN_POINT('Ctrl Pts',(-1.43368173786436,16.9603544152598,8.27008105335408));
#9275=CARTESIAN_POINT('Ctrl Pts',(0.734035591731605,17.0413133397641,8.36727881874682));
#9276=CARTESIAN_POINT('Ctrl Pts',(1.83997710111426,17.0834518014106,8.19544045616635));
#9277=CARTESIAN_POINT('Ctrl Pts',(3.90203516139383,17.1744991125026,7.43525885814066));
#9278=CARTESIAN_POINT('Ctrl Pts',(4.84033335378641,17.220717531209,6.86149869059172));
#9279=CARTESIAN_POINT('Ctrl Pts',(6.41637397647712,17.3086126976293,5.40948023465566));
#9280=CARTESIAN_POINT('Ctrl Pts',(7.0486350625867,17.3472412213165,4.55507985860513));
#9281=CARTESIAN_POINT('Ctrl Pts',(7.98257278257802,17.428959582952,2.6111167758123));
#9282=CARTESIAN_POINT('Ctrl Pts',(8.25790602060779,17.4743363547778,1.5316681980353));
#9283=CARTESIAN_POINT('Ctrl Pts',(8.37051137781878,17.5658525086914,-0.645370366206906));
#9284=CARTESIAN_POINT('Ctrl Pts',(8.21696717253769,17.6110904807199,-1.7215170950898));
#9285=CARTESIAN_POINT('Ctrl Pts',(7.51254948138263,17.6961083691393,-3.74397120645815));
#9286=CARTESIAN_POINT('Ctrl Pts',(6.97282744523094,17.7330925721754,-4.67283653177338));
#9287=CARTESIAN_POINT('Ctrl Pts',(5.54505326333423,17.8194536431009,-6.3086721157136));
#9288=CARTESIAN_POINT('Ctrl Pts',(4.65840815242837,17.8660313162708,-6.98899034570502));
#9289=CARTESIAN_POINT('Ctrl Pts',(2.70886925636158,17.95709134306,-7.94466582950618));
#9290=CARTESIAN_POINT('Ctrl Pts',(1.67178820401725,18.000752057619,-8.22564080909474));
#9291=CARTESIAN_POINT('Ctrl Pts',(0.40662470803591,18.0487635135138,-8.31856125006016));
#9292=CARTESIAN_POINT('Ctrl Pts',(0.203202195754393,18.0563254824552,-8.326));
#9293=CARTESIAN_POINT('Ctrl Pts',(2.88657986402541E-13,18.0637230794129,
-8.326));
#9294=CARTESIAN_POINT('Ctrl Pts',(-1.62647673107585E-13,17.6627746953453,
-8.32600000000001));
#9295=CARTESIAN_POINT('Ctrl Pts',(0.937428171083856,17.6286475258,-8.32600000000003));
#9296=CARTESIAN_POINT('Ctrl Pts',(1.86902802054237,17.5914051457875,-8.16769223739126));
#9297=CARTESIAN_POINT('Ctrl Pts',(3.78693416571463,17.5074465822747,-7.49509455465147));
#9298=CARTESIAN_POINT('Ctrl Pts',(4.7372426102813,17.4610503279071,-6.93367584142013));
#9299=CARTESIAN_POINT('Ctrl Pts',(6.36854294282441,17.3709826643249,-5.47400880272639));
#9300=CARTESIAN_POINT('Ctrl Pts',(7.03283715715672,17.3306964041795,-4.58933185072455));
#9301=CARTESIAN_POINT('Ctrl Pts',(7.96749087277855,17.2488016572187,-2.64117281302412));
#9302=CARTESIAN_POINT('Ctrl Pts',(8.23964999089758,17.2050932528527,-1.60141231373512));
#9303=CARTESIAN_POINT('Ctrl Pts',(8.38017383007285,17.1139867134581,0.565882106262566));
#9304=CARTESIAN_POINT('Ctrl Pts',(8.23080475600197,17.067413244654,1.67379839558519));
#9305=CARTESIAN_POINT('Ctrl Pts',(7.52151860508346,16.9811548538322,3.72576228696615));
#9306=CARTESIAN_POINT('Ctrl Pts',(6.98435774174966,16.9441902237068,4.65545852901487));
#9307=CARTESIAN_POINT('Ctrl Pts',(5.58036455598891,16.8590930472698,6.27235151787872));
#9308=CARTESIAN_POINT('Ctrl Pts',(4.72285823283805,16.8138217755528,6.94098476017238));
#9309=CARTESIAN_POINT('Ctrl Pts',(2.77783410889142,16.7223079121988,7.92607230575084));
#9310=CARTESIAN_POINT('Ctrl Pts',(1.70442017914298,16.6769679903503,8.22400878079362));
#9311=CARTESIAN_POINT('Ctrl Pts',(-0.446522969877771,16.5953737458763,8.38048698816194));
#9312=CARTESIAN_POINT('Ctrl Pts',(-1.50218431899096,16.5566342895529,8.25685945638442));
#9313=CARTESIAN_POINT('Ctrl Pts',(-3.54600325216184,16.4686652785713,7.61154348763457));
#9314=CARTESIAN_POINT('Ctrl Pts',(-4.51068510061488,16.4224286312543,7.08261388765972));
#9315=CARTESIAN_POINT('Ctrl Pts',(-6.19486653546212,16.3314671777391,5.67201563359183));
#9316=CARTESIAN_POINT('Ctrl Pts',(-6.89326576259661,16.2895104354326,4.79900506276053));
#9317=CARTESIAN_POINT('Ctrl Pts',(-7.88714772594216,16.2084670496717,2.87109869177676));
#9318=CARTESIAN_POINT('Ctrl Pts',(-8.18867382432303,16.1652362687781,1.84270017257802));
#9319=CARTESIAN_POINT('Ctrl Pts',(-8.39297278532252,16.0746150173042,-0.313049941056341));
#9320=CARTESIAN_POINT('Ctrl Pts',(-8.27765322129032,16.0280198395401,-1.42148265552545));
#9321=CARTESIAN_POINT('Ctrl Pts',(-7.631489900257,15.9407801999068,-3.49678905434423));
#9322=CARTESIAN_POINT('Ctrl Pts',(-7.11949600278651,15.9034817484166,-4.44746066470012));
#9323=CARTESIAN_POINT('Ctrl Pts',(-5.76095076674326,15.8191561169798,-6.10636390487672));
#9324=CARTESIAN_POINT('Ctrl Pts',(-4.92591855586582,15.774221829667,-6.79789069632792));
#9325=CARTESIAN_POINT('Ctrl Pts',(-3.01387150876772,15.6827230275315,-7.83937964475539));
#9326=CARTESIAN_POINT('Ctrl Pts',(-1.9497251141762,15.6370472783281,-8.16934566758503));
#9327=CARTESIAN_POINT('Ctrl Pts',(-0.568555311775885,15.5837786856521,-8.31145683949874));
#9328=CARTESIAN_POINT('Ctrl Pts',(-0.284127003756134,15.57311836831,-8.326));
#9329=CARTESIAN_POINT('Ctrl Pts',(-1.89154247820511E-13,15.5627746953453,
-8.326));
#9330=CARTESIAN_POINT('Origin',(0.,-25.4,0.));
#9331=CARTESIAN_POINT('',(-1.11957170745022E-14,13.4627746953453,-8.326));
#9332=CARTESIAN_POINT('',(-5.82414177429932E-14,13.863723079413,-8.32600000000001));
#9333=CARTESIAN_POINT('',(-1.01964092497009E-15,-25.4,-8.326));
#9334=CARTESIAN_POINT('Ctrl Pts',(-1.4582085539061E-13,13.863723079413,
-8.326));
#9335=CARTESIAN_POINT('Ctrl Pts',(-0.135836828135204,13.8686682331935,-8.326));
#9336=CARTESIAN_POINT('Ctrl Pts',(-0.271785053719794,13.8736873117228,-8.32267581772396));
#9337=CARTESIAN_POINT('Ctrl Pts',(-1.50950589218815,13.9200221532606,-8.26199182042639));
#9338=CARTESIAN_POINT('Ctrl Pts',(-2.58954375088037,13.9650672888594,-7.98955341437777));
#9339=CARTESIAN_POINT('Ctrl Pts',(-4.55944747076069,14.0565344481263,-7.0497806400479));
#9340=CARTESIAN_POINT('Ctrl Pts',(-5.43428128731425,14.1020456522445,-6.39974419856835));
#9341=CARTESIAN_POINT('Ctrl Pts',(-6.87391755623469,14.1877391807443,-4.81621411339271));
#9342=CARTESIAN_POINT('Ctrl Pts',(-7.43074385164979,14.2246674325236,-3.90264947429375));
#9343=CARTESIAN_POINT('Ctrl Pts',(-8.1889707434789,14.3101409425543,-1.8693567756763));
#9344=CARTESIAN_POINT('Ctrl Pts',(-8.36492764659033,14.3566680587784,-0.762543148013781));
#9345=CARTESIAN_POINT('Ctrl Pts',(-8.27443805711982,14.4480989999331,1.41246832642682));
#9346=CARTESIAN_POINT('Ctrl Pts',(-8.02543631461458,14.4921553401998,2.46050572374258));
#9347=CARTESIAN_POINT('Ctrl Pts',(-7.1367614153721,14.5746973638872,4.42406255008773));
#9348=CARTESIAN_POINT('Ctrl Pts',(-6.49834127821936,14.6139194508751,5.31765719475317));
#9349=CARTESIAN_POINT('Ctrl Pts',(-4.90799537658902,14.7032735693802,6.81431095251126));
#9350=CARTESIAN_POINT('Ctrl Pts',(-3.96945604358268,14.7497608912359,7.40044709581961));
#9351=CARTESIAN_POINT('Ctrl Pts',(-1.95701469491134,14.8390158062621,8.16129027556823));
#9352=CARTESIAN_POINT('Ctrl Pts',(-0.907781491932131,14.8803102780559,8.34336195724052));
#9353=CARTESIAN_POINT('Ctrl Pts',(1.25002532406152,14.959667796113,8.30518902206611));
#9354=CARTESIAN_POINT('Ctrl Pts',(2.33788033733056,15.0042827301164,8.06675808767319));
#9355=CARTESIAN_POINT('Ctrl Pts',(4.33911191421371,15.0956082046261,7.18798770930206));
#9356=CARTESIAN_POINT('Ctrl Pts',(5.23629522702819,15.141401066234,6.56326127224253));
#9357=CARTESIAN_POINT('Ctrl Pts',(6.72280797819924,15.2278661186725,5.02421673135485));
#9358=CARTESIAN_POINT('Ctrl Pts',(7.30548506957144,15.2650502817789,4.13142775172451));
#9359=CARTESIAN_POINT('Ctrl Pts',(8.12735299824442,15.3494719846849,2.12315604202303));
#9360=CARTESIAN_POINT('Ctrl Pts',(8.33808083599502,15.3958996429541,1.01870837702462));
#9361=CARTESIAN_POINT('Ctrl Pts',(8.31333421448786,15.4876828292901,-1.16468250707291));
#9362=CARTESIAN_POINT('Ctrl Pts',(8.09491472867419,15.5321611558964,-2.22275835656821));
#9363=CARTESIAN_POINT('Ctrl Pts',(7.26610606428713,15.6155283161931,-4.20594400408292));
#9364=CARTESIAN_POINT('Ctrl Pts',(6.66060813053494,15.6536692230037,-5.11103507158764));
#9365=CARTESIAN_POINT('Ctrl Pts',(5.12339638574204,15.7420719450369,-6.6544551627523));
#9366=CARTESIAN_POINT('Ctrl Pts',(4.2009289386824,15.7886358811958,-7.27207371873985));
#9367=CARTESIAN_POINT('Ctrl Pts',(2.20749238849329,15.8785557742899,-8.09747193158456));
#9368=CARTESIAN_POINT('Ctrl Pts',(1.16141776831797,15.9211526735467,-8.31225630215715));
#9369=CARTESIAN_POINT('Ctrl Pts',(0.0687215117795646,15.9612167961274,-8.32578735205743));
#9370=CARTESIAN_POINT('Ctrl Pts',(0.0343560586356681,15.9624723435442,-8.326));
#9371=CARTESIAN_POINT('Ctrl Pts',(-1.69645946028209E-13,15.9637230794129,
-8.326));
#9372=CARTESIAN_POINT('Ctrl Pts',(-1.55153667691366E-13,15.5627746953453,
-8.326));
#9373=CARTESIAN_POINT('Ctrl Pts',(0.766473007452974,15.5348711662173,-8.32600000000002));
#9374=CARTESIAN_POINT('Ctrl Pts',(1.53059056240928,15.5048290963712,-8.22017457936218));
#9375=CARTESIAN_POINT('Ctrl Pts',(3.315932973231,15.4291964951735,-7.71409527197532));
#9376=CARTESIAN_POINT('Ctrl Pts',(4.29316118863751,15.3831522201064,-7.21604913902925));
#9377=CARTESIAN_POINT('Ctrl Pts',(6.01417786317076,15.2920486182911,-5.86248838162399));
#9378=CARTESIAN_POINT('Ctrl Pts',(6.73696230357398,15.2485957082345,-5.01513072376378));
#9379=CARTESIAN_POINT('Ctrl Pts',(7.78880263202565,15.169221526306,-3.12693232737676));
#9380=CARTESIAN_POINT('Ctrl Pts',(8.12286538336693,15.1265692379339,-2.11229531884364));
#9381=CARTESIAN_POINT('Ctrl Pts',(8.39826316592157,15.036585808248,0.0282819256256184));
#9382=CARTESIAN_POINT('Ctrl Pts',(8.3211193271742,14.9900167842913,1.13609247837785));
#9383=CARTESIAN_POINT('Ctrl Pts',(7.74647417120216,14.9017102095279,3.23677973975202));
#9384=CARTESIAN_POINT('Ctrl Pts',(7.2627833257141,14.8636583216416,4.21146930995301));
#9385=CARTESIAN_POINT('Ctrl Pts',(5.9550395739323,14.7802099460948,5.91662597317146));
#9386=CARTESIAN_POINT('Ctrl Pts',(5.14556445242495,14.7356914964966,6.6326345715706));
#9387=CARTESIAN_POINT('Ctrl Pts',(3.26313744592203,14.643877584444,7.74041896476706));
#9388=CARTESIAN_POINT('Ctrl Pts',(2.19981065428884,14.5974622874687,8.10699015155958));
#9389=CARTESIAN_POINT('Ctrl Pts',(0.0486893857144464,14.5131473062414,8.39260472799874));
#9390=CARTESIAN_POINT('Ctrl Pts',(-1.01534262136813,14.4759184106797,8.33110828659527));
#9391=CARTESIAN_POINT('Ctrl Pts',(-3.08990218717426,14.3893767506368,7.80694593494561));
#9392=CARTESIAN_POINT('Ctrl Pts',(-4.07838391792978,14.3435578020054,7.33911185036683));
#9393=CARTESIAN_POINT('Ctrl Pts',(-5.83618716670347,14.2522516602417,6.0396310365248));
#9394=CARTESIAN_POINT('Ctrl Pts',(-6.58398529979185,14.2076825850543,5.21438613963775));
#9395=CARTESIAN_POINT('Ctrl Pts',(-7.69022007882209,14.1284560366258,3.36106816935293));
#9396=CARTESIAN_POINT('Ctrl Pts',(-8.05404936263119,14.0869802088156,2.35995744330347));
#9397=CARTESIAN_POINT('Ctrl Pts',(-8.39456826427114,13.9976526424611,0.234982250540276));
#9398=CARTESIAN_POINT('Ctrl Pts',(-8.35255602044774,13.9511551906314,-0.871125703558243));
#9399=CARTESIAN_POINT('Ctrl Pts',(-7.84456729604378,13.8618985928561,-2.9944126552092));
#9400=CARTESIAN_POINT('Ctrl Pts',(-7.38713856607453,13.8228045832374,-3.99170590989937));
#9401=CARTESIAN_POINT('Ctrl Pts',(-6.12610103946332,13.7401760861308,-5.73875265446514));
#9402=CARTESIAN_POINT('Ctrl Pts',(-5.34046520368155,13.6960743460471,-6.47622625885644));
#9403=CARTESIAN_POINT('Ctrl Pts',(-3.49787283183606,13.6046031740294,-7.63669967157466));
#9404=CARTESIAN_POINT('Ctrl Pts',(-2.44973670994727,13.5580843076334,-8.03450940729452));
#9405=CARTESIAN_POINT('Ctrl Pts',(-0.905737253757057,13.4965243087677,-8.28907276263488));
#9406=CARTESIAN_POINT('Ctrl Pts',(-0.452759042309395,13.4792574351185,-8.32599999999999));
#9407=CARTESIAN_POINT('Ctrl Pts',(-1.12271303365219E-13,13.4627746953453,
-8.326));
#9408=CARTESIAN_POINT('Origin',(0.,-25.4,0.));
#9409=CARTESIAN_POINT('',(1.23965221987824E-14,11.3627746953453,-8.326));
#9410=CARTESIAN_POINT('',(-1.7738222607308E-13,11.763723079413,-8.32600000000001));
#9411=CARTESIAN_POINT('',(-1.01964092497009E-15,-25.4,-8.326));
#9412=CARTESIAN_POINT('Ctrl Pts',(-2.02754479872169E-13,11.763723079413,
-8.326));
#9413=CARTESIAN_POINT('Ctrl Pts',(-0.303252472074516,11.7747630170303,-8.326));
#9414=CARTESIAN_POINT('Ctrl Pts',(-0.606820499119774,11.7861626527411,-8.30943314966895));
#9415=CARTESIAN_POINT('Ctrl Pts',(-2.006123196559,11.8403360153408,-8.15568270533984));
#9416=CARTESIAN_POINT('Ctrl Pts',(-3.0679903265585,11.8860833591555,-7.81836261337937));
#9417=CARTESIAN_POINT('Ctrl Pts',(-4.97219018423794,11.9775669309886,-6.76400654845765));
#9418=CARTESIAN_POINT('Ctrl Pts',(-5.80194903063939,12.0224181649271,-6.06729746404484));
#9419=CARTESIAN_POINT('Ctrl Pts',(-7.14994139612737,12.1065628343985,-4.39872576918177));
#9420=CARTESIAN_POINT('Ctrl Pts',(-7.65607384812685,12.1439849020982,-3.44311446949431));
#9421=CARTESIAN_POINT('Ctrl Pts',(-8.28746475539839,12.2314488778649,-1.36247143454109));
#9422=CARTESIAN_POINT('Ctrl Pts',(-8.39486154416642,12.2780430273218,-0.254063182030855));
#9423=CARTESIAN_POINT('Ctrl Pts',(-8.17577182323232,12.3685400772549,1.89873235437619));
#9424=CARTESIAN_POINT('Ctrl Pts',(-7.86745931090753,12.4116545474063,2.92436400717674));
#9425=CARTESIAN_POINT('Ctrl Pts',(-6.85972962789788,12.4924959910119,4.84746646277679));
#9426=CARTESIAN_POINT('Ctrl Pts',(-6.1532288151958,12.5348918593769,5.71771214982715));
#9427=CARTESIAN_POINT('Ctrl Pts',(-4.45667115926648,12.6260577404462,7.11660023911833));
#9428=CARTESIAN_POINT('Ctrl Pts',(-3.48876230026754,12.6722501006202,7.63783343714226));
#9429=CARTESIAN_POINT('Ctrl Pts',(-1.44092546537248,12.7600423327032,8.26777956105381));
#9430=CARTESIAN_POINT('Ctrl Pts',(-0.384296819897299,12.7985224076212,8.38358291612028));
#9431=CARTESIAN_POINT('Ctrl Pts',(1.76555131698124,12.8804130475961,8.21110644099873));
#9432=CARTESIAN_POINT('Ctrl Pts',(2.83675341664969,12.9258403501148,7.90518164125101));
#9433=CARTESIAN_POINT('Ctrl Pts',(4.77373411316413,13.0173582017968,6.90597271744218));
#9434=CARTESIAN_POINT('Ctrl Pts',(5.62570972681814,13.0625491659331,6.23158081053345));
#9435=CARTESIAN_POINT('Ctrl Pts',(7.01844275423167,13.1474563783671,4.60422259982182));
#9436=CARTESIAN_POINT('Ctrl Pts',(7.54937778889659,13.1844736122372,3.66937446773204));
#9437=CARTESIAN_POINT('Ctrl Pts',(8.24309946706272,13.2709773220947,1.61157478694954));
#9438=CARTESIAN_POINT('Ctrl Pts',(8.38404516506843,13.3175601021255,0.503436996845469));
#9439=CARTESIAN_POINT('Ctrl Pts',(8.22771272001427,13.408553899823,-1.66117545923843));
#9440=CARTESIAN_POINT('Ctrl Pts',(7.94825830436621,13.4521475008907,-2.69820495206495));
#9441=CARTESIAN_POINT('Ctrl Pts',(6.9989919870918,13.5338340516951,-4.6414113006288));
#9442=CARTESIAN_POINT('Ctrl Pts',(6.32636525605991,13.5745011148047,-5.52323132314027));
#9443=CARTESIAN_POINT('Ctrl Pts',(4.68202887376216,13.6647920808336,-6.97094335373384));
#9444=CARTESIAN_POINT('Ctrl Pts',(3.728089952798,13.7111534209451,-7.52441277683913));
#9445=CARTESIAN_POINT('Ctrl Pts',(1.82619866592454,13.7940649276322,-8.17493303565393));
#9446=CARTESIAN_POINT('Ctrl Pts',(0.915744931208586,13.8303852904585,-8.32600000000003));
#9447=CARTESIAN_POINT('Ctrl Pts',(-1.52655665885959E-13,13.863723079413,
-8.32600000000001));
#9448=CARTESIAN_POINT('Ctrl Pts',(-1.28785870856518E-13,13.4627746953453,
-8.326));
#9449=CARTESIAN_POINT('Ctrl Pts',(0.602475208085855,13.4408415230689,-8.32600000000002));
#9450=CARTESIAN_POINT('Ctrl Pts',(1.20446106602682,13.4175518737411,-8.26061511824214));
#9451=CARTESIAN_POINT('Ctrl Pts',(2.85005435699202,13.3500058164016,-7.89721788731316));
#9452=CARTESIAN_POINT('Ctrl Pts',(3.84936152349472,13.3044637551861,-7.46130751960217));
#9453=CARTESIAN_POINT('Ctrl Pts',(5.64444722471778,13.2130069623409,-6.21923425961092));
#9454=CARTESIAN_POINT('Ctrl Pts',(6.41781466084013,13.1680039634893,-5.41763184652892));
#9455=CARTESIAN_POINT('Ctrl Pts',(7.58056217918825,13.087492624649,-3.60107015505294));
#9456=CARTESIAN_POINT('Ctrl Pts',(7.97507616633824,13.0476459325469,-2.61367977412177));
#9457=CARTESIAN_POINT('Ctrl Pts',(8.38213775996806,12.9590437430625,-0.505960260844928));
#9458=CARTESIAN_POINT('Ctrl Pts',(8.37612732733517,12.9126673606885,0.597267623858461));
#9459=CARTESIAN_POINT('Ctrl Pts',(7.93743142281672,12.8224701255431,2.74293099477509));
#9460=CARTESIAN_POINT('Ctrl Pts',(7.50726802011452,12.7819657713616,3.76391307165841));
#9461=CARTESIAN_POINT('Ctrl Pts',(6.2941538258584,12.700191484644,5.55332457302669));
#9462=CARTESIAN_POINT('Ctrl Pts',(5.53325443955575,12.6565493400172,6.31177672600054));
#9463=CARTESIAN_POINT('Ctrl Pts',(3.7325000233972,12.56550754908,7.52428687864775));
#9464=CARTESIAN_POINT('Ctrl Pts',(2.70065483388178,12.5189283691453,7.95318288278388));
#9465=CARTESIAN_POINT('Ctrl Pts',(0.570533848588451,12.4325276141087,8.37440617533124));
#9466=CARTESIAN_POINT('Ctrl Pts',(-0.503966248242079,12.3955349082409,8.37867533336922));
#9467=CARTESIAN_POINT('Ctrl Pts',(-2.6082270937139,12.3105477467568,7.97991570715822));
#9468=CARTESIAN_POINT('Ctrl Pts',(-3.61732900654454,12.2653227648794,7.57605606670174));
#9469=CARTESIAN_POINT('Ctrl Pts',(-5.44772472808909,12.1738059650236,6.39228659380338));
#9470=CARTESIAN_POINT('Ctrl Pts',(-6.24582818079019,12.1284150581469,5.61507266269158));
#9471=CARTESIAN_POINT('Ctrl Pts',(-7.4645333267061,12.0466487516106,3.83572464787945));
#9472=CARTESIAN_POINT('Ctrl Pts',(-7.88950950913947,12.0080621878062,2.86146760637413));
#9473=CARTESIAN_POINT('Ctrl Pts',(-8.36145215618212,11.9201956169881,0.771247410285937));
#9474=CARTESIAN_POINT('Ctrl Pts',(-8.39053311634181,11.8739843619691,-0.328052330537919));
#9475=CARTESIAN_POINT('Ctrl Pts',(-8.02048208966464,11.7829039823986,-2.49472444569266));
#9476=CARTESIAN_POINT('Ctrl Pts',(-7.61737029272528,11.7406944885028,-3.53932837946436));
#9477=CARTESIAN_POINT('Ctrl Pts',(-6.45112885884589,11.6597682299118,-5.36957912797074));
#9478=CARTESIAN_POINT('Ctrl Pts',(-5.71463194672094,11.6166047768032,-6.14752283130325));
#9479=CARTESIAN_POINT('Ctrl Pts',(-3.95561993247836,11.5260551556824,-7.40891691123526));
#9480=CARTESIAN_POINT('Ctrl Pts',(-2.94033701199002,11.4794602953578,-7.86724563496573));
#9481=CARTESIAN_POINT('Ctrl Pts',(-1.25207829660374,11.409842157908,-8.25532783449594));
#9482=CARTESIAN_POINT('Ctrl Pts',(-0.626361873301063,11.38557746414,-8.326));
#9483=CARTESIAN_POINT('Ctrl Pts',(2.84772205816353E-13,11.3627746953453,
-8.326));
#9484=CARTESIAN_POINT('Origin',(0.,-25.4,0.));
#9485=CARTESIAN_POINT('',(1.94473098237308E-13,9.26277469534531,-8.326));
#9486=CARTESIAN_POINT('',(1.71062558676527E-15,9.66372307941294,-8.326));
#9487=CARTESIAN_POINT('',(-1.01964092497009E-15,-25.4,-8.326));
#9488=CARTESIAN_POINT('Ctrl Pts',(-1.72223346694977E-13,9.66372307941295,
-8.326));
#9489=CARTESIAN_POINT('Ctrl Pts',(-0.474199948109406,9.68098637757983,-8.326));
#9490=CARTESIAN_POINT('Ctrl Pts',(-0.948564287601614,9.69910706346753,-8.28549267616555));
#9491=CARTESIAN_POINT('Ctrl Pts',(-2.51093903145465,9.76166088539588,-8.01547299083435));
#9492=CARTESIAN_POINT('Ctrl Pts',(-3.55519873590362,9.80819853902353,-7.61005526035746));
#9493=CARTESIAN_POINT('Ctrl Pts',(-5.3877587457154,9.8995729445105,-6.43680916193083));
#9494=CARTESIAN_POINT('Ctrl Pts',(-6.16743606182152,9.94356643510009,-5.6941653003555));
#9495=CARTESIAN_POINT('Ctrl Pts',(-7.41688487727091,10.0259895644163,-3.93681713196663));
#9496=CARTESIAN_POINT('Ctrl Pts',(-7.86775284239254,10.0653932510665,-2.93384043089224));
#9497=CARTESIAN_POINT('Ctrl Pts',(-8.35906861457206,10.1548806124347,-0.805063943029334));
#9498=CARTESIAN_POINT('Ctrl Pts',(-8.39236780364888,10.2013532156509,0.300452898050963));
#9499=CARTESIAN_POINT('Ctrl Pts',(-8.03573869924169,10.2905079433405,2.42131650589003));
#9500=CARTESIAN_POINT('Ctrl Pts',(-7.66452791394732,10.331559107744,3.41908188803614));
#9501=CARTESIAN_POINT('Ctrl Pts',(-6.54469345955934,10.4110963696274,5.26362738806832));
#9502=CARTESIAN_POINT('Ctrl Pts',(-5.79069118709908,10.4557736515338,6.0832745668736));
#9503=CARTESIAN_POINT('Ctrl Pts',(-4.02377198376237,10.5471242117649,7.36907938802327));
#9504=CARTESIAN_POINT('Ctrl Pts',(-3.03260117434181,10.5928804912406,7.82927423235415));
#9505=CARTESIAN_POINT('Ctrl Pts',(-0.954371183257477,10.6792397998651,8.33840346145337));
#9506=CARTESIAN_POINT('Ctrl Pts',(0.110819689456831,10.7163680467929,8.39210534172936));
#9507=CARTESIAN_POINT('Ctrl Pts',(2.25961469410576,10.8009363753522,8.09040801577519));
#9508=CARTESIAN_POINT('Ctrl Pts',(3.31939921095577,10.8473803507535,7.71633699151253));
#9509=CARTESIAN_POINT('Ctrl Pts',(5.19245858238359,10.9391198505578,6.5958677005875));
#9510=CARTESIAN_POINT('Ctrl Pts',(5.99630069783449,10.983542260661,5.87467173427252));
#9511=CARTESIAN_POINT('Ctrl Pts',(7.2929547143924,11.0667971103334,4.15951449438082));
#9512=CARTESIAN_POINT('Ctrl Pts',(7.77043385499936,11.1050663529639,3.17950258404369));
#9513=CARTESIAN_POINT('Ctrl Pts',(8.32933089730255,11.1936012981371,1.07338271686461));
#9514=CARTESIAN_POINT('Ctrl Pts',(8.39813326278913,11.2401574660181,-0.0341220082125714));
#9515=CARTESIAN_POINT('Ctrl Pts',(8.10725762469965,11.3299882681282,-2.17106846069599));
#9516=CARTESIAN_POINT('Ctrl Pts',(7.76614069422855,11.3725080725837,-3.18255386611217));
#9517=CARTESIAN_POINT('Ctrl Pts',(6.70139780907636,11.4515366532656,-5.06253090256127));
#9518=CARTESIAN_POINT('Ctrl Pts',(5.97271674059568,11.4953938433415,-5.90471045661073));
#9519=CARTESIAN_POINT('Ctrl Pts',(4.24285960338634,11.5865535444329,-7.24562812676891));
#9520=CARTESIAN_POINT('Ctrl Pts',(3.2628970493093,11.6325481260211,-7.73657397246758));
#9521=CARTESIAN_POINT('Ctrl Pts',(1.49306607867275,11.7072519314285,-8.22533043235189));
#9522=CARTESIAN_POINT('Ctrl Pts',(0.747569406382801,11.7365077378375,-8.32600000000001));
#9523=CARTESIAN_POINT('Ctrl Pts',(-1.68060010352633E-13,11.763723079413,
-8.326));
#9524=CARTESIAN_POINT('Ctrl Pts',(3.17246229286638E-13,11.3627746953453,
-8.326));
#9525=CARTESIAN_POINT('Ctrl Pts',(0.43974300939449,11.3467658055969,-8.326));
#9526=CARTESIAN_POINT('Ctrl Pts',(0.879750206370908,11.330015125447,-8.29116531842167));
#9527=CARTESIAN_POINT('Ctrl Pts',(2.37622328087344,11.270501412391,-8.05164028759308));
#9528=CARTESIAN_POINT('Ctrl Pts',(3.39370126759801,11.2256151617867,-7.67840429886385));
#9529=CARTESIAN_POINT('Ctrl Pts',(5.25588865827407,11.1341246763999,-6.55095157941137));
#9530=CARTESIAN_POINT('Ctrl Pts',(6.07676516332524,11.0884070404113,-5.79763689437981));
#9531=CARTESIAN_POINT('Ctrl Pts',(7.34829876630346,11.0054727971358,-4.05422335819444));
#9532=CARTESIAN_POINT('Ctrl Pts',(7.8021809619017,10.9677524572588,-3.09198527340771));
#9533=CARTESIAN_POINT('Ctrl Pts',(8.33451523277333,10.88059469251,-1.01862656112783));
#9534=CARTESIAN_POINT('Ctrl Pts',(8.39618247397769,10.834579066331,0.0760194490623026));
#9535=CARTESIAN_POINT('Ctrl Pts',(8.09341281379174,10.7434423052017,2.24403280095633));
#9536=CARTESIAN_POINT('Ctrl Pts',(7.72529352344289,10.6997560888879,3.2951318423501));
#9537=CARTESIAN_POINT('Ctrl Pts',(6.62387520353467,10.6205825087671,5.15427208379822));
#9538=CARTESIAN_POINT('Ctrl Pts',(5.91584121845181,10.5780070403487,5.95354039130136));
#9539=CARTESIAN_POINT('Ctrl Pts',(4.20606760973629,10.4881118368888,7.2690825687462));
#9540=CARTESIAN_POINT('Ctrl Pts',(3.21067803326855,10.4415499806909,7.76029733300199));
#9541=CARTESIAN_POINT('Ctrl Pts',(1.10594381595948,10.3531103177683,8.32249720930198));
#9542=CARTESIAN_POINT('Ctrl Pts',(0.0191197917106355,10.3149342484212,8.39562891452947));
#9543=CARTESIAN_POINT('Ctrl Pts',(-2.1132777072148,10.2315983927577,8.12416781458325));
#9544=CARTESIAN_POINT('Ctrl Pts',(-3.13907909322553,10.1871356018457,7.7854953785785));
#9545=CARTESIAN_POINT('Ctrl Pts',(-5.04334369665254,10.0953644533491,6.71756938058307));
#9546=CARTESIAN_POINT('Ctrl Pts',(-5.89522363595378,10.0489321566374,5.9839527035621));
#9547=CARTESIAN_POINT('Ctrl Pts',(-7.22556881879485,9.96446947296532,4.26968498468107));
#9548=CARTESIAN_POINT('Ctrl Pts',(-7.70859384852291,9.92730158568948,3.31914539716159));
#9549=CARTESIAN_POINT('Ctrl Pts',(-8.30059192471654,9.84086603030577,1.26296701394893));
#9550=CARTESIAN_POINT('Ctrl Pts',(-8.39431687163808,9.79508330663404,0.173861421689487));
#9551=CARTESIAN_POINT('Ctrl Pts',(-8.15739166509317,9.70375064862286,-1.99881203717135));
#9552=CARTESIAN_POINT('Ctrl Pts',(-7.82123735923041,9.65911821207469,-3.06055394202927));
#9553=CARTESIAN_POINT('Ctrl Pts',(-6.77772150535337,9.57971043425691,-4.94955153663381));
#9554=CARTESIAN_POINT('Ctrl Pts',(-6.0964918257955,9.53848464817047,-5.76794177750132));
#9555=CARTESIAN_POINT('Ctrl Pts',(-4.43324056799386,9.44925769153702,-7.13226975569284));
#9556=CARTESIAN_POINT('Ctrl Pts',(-3.45714963380328,9.40277439015981,-7.65317333496234));
#9557=CARTESIAN_POINT('Ctrl Pts',(-1.62582185353653,9.32447410626235,-8.20652436697391));
#9558=CARTESIAN_POINT('Ctrl Pts',(-0.814402088748981,9.29242308763611,-8.32600000000001));
#9559=CARTESIAN_POINT('Ctrl Pts',(2.66453525910038E-13,9.26277469534532,
-8.32600000000001));
#9560=CARTESIAN_POINT('Origin',(0.,-25.4,0.));
#9561=CARTESIAN_POINT('',(1.6837414297283E-14,7.16277469534533,-8.326));
#9562=CARTESIAN_POINT('',(5.38911077441476E-14,7.56372307941295,-8.326));
#9563=CARTESIAN_POINT('',(-1.01964092497009E-15,-25.4,-8.326));
#9564=CARTESIAN_POINT('Ctrl Pts',(2.52159404467989E-13,7.56372307941294,
-8.326));
#9565=CARTESIAN_POINT('Ctrl Pts',(-0.646166079188242,7.58724682237162,-8.326));
#9566=CARTESIAN_POINT('Ctrl Pts',(-1.29151752362468,7.61232174378504,-8.25078837229487));
#9567=CARTESIAN_POINT('Ctrl Pts',(-2.99553195348629,7.68285860964985,-7.84628539769874));
#9568=CARTESIAN_POINT('Ctrl Pts',(-4.00685913034017,7.7294511525345,-7.38121538218405));
#9569=CARTESIAN_POINT('Ctrl Pts',(-5.7560065685614,7.81987582713428,-6.10867995386882));
#9570=CARTESIAN_POINT('Ctrl Pts',(-6.48677428614185,7.86292342757756,-5.32632493330393));
#9571=CARTESIAN_POINT('Ctrl Pts',(-7.64205544266831,7.94364960845092,-3.48660955371491));
#9572=CARTESIAN_POINT('Ctrl Pts',(-8.03877974932396,7.98630322303686,-2.43642206911082));
#9573=CARTESIAN_POINT('Ctrl Pts',(-8.39265713520717,8.07758446765967,-0.264971661311598));
#9574=CARTESIAN_POINT('Ctrl Pts',(-8.35539629462834,8.12375047093282,0.833251605123153));
#9575=CARTESIAN_POINT('Ctrl Pts',(-7.86831170863093,8.21144146718116,2.91929513301856));
#9576=CARTESIAN_POINT('Ctrl Pts',(-7.43614052398183,8.24978250879786,3.89052068008099));
#9577=CARTESIAN_POINT('Ctrl Pts',(-6.20425617670594,8.33184176118451,5.66097917510394));
#9578=CARTESIAN_POINT('Ctrl Pts',(-5.40041701443523,8.37731781705428,6.43230971163402));
#9579=CARTESIAN_POINT('Ctrl Pts',(-3.56194700431721,8.46883564977609,7.60214324730046));
#9580=CARTESIAN_POINT('Ctrl Pts',(-2.55067534908799,8.51397971436136,7.99839497011445));
#9581=CARTESIAN_POINT('Ctrl Pts',(-0.443025731472404,8.59877788690376,8.38229351692315));
#9582=CARTESIAN_POINT('Ctrl Pts',(0.632825873132995,8.63583414320664,8.37010532378516));
#9583=CARTESIAN_POINT('Ctrl Pts',(2.76020839296628,8.72247757178746,7.93259315604519));
#9584=CARTESIAN_POINT('Ctrl Pts',(3.78803083251719,8.76906451810793,7.49636004213978));
#9585=CARTESIAN_POINT('Ctrl Pts',(5.57857788868775,8.85999159475243,6.27162800167303));
#9586=CARTESIAN_POINT('Ctrl Pts',(6.33348554769889,8.90351846461245,5.50828231665004));
#9587=CARTESIAN_POINT('Ctrl Pts',(7.53505857253065,8.98508509467007,3.70876063403948));
#9588=CARTESIAN_POINT('Ctrl Pts',(7.95859913789034,9.02597976931485,2.68200228536735));
#9589=CARTESIAN_POINT('Ctrl Pts',(8.38047241067967,9.11639797448044,0.531082353341697));
#9590=CARTESIAN_POINT('Ctrl Pts',(8.37782841188649,9.16273798161244,-0.571280216318487));
#9591=CARTESIAN_POINT('Ctrl Pts',(7.95477284015797,9.25116138123764,-2.67474657425873));
#9592=CARTESIAN_POINT('Ctrl Pts',(7.55280247544499,9.29066662359165,-3.65887733459845));
#9593=CARTESIAN_POINT('Ctrl Pts',(6.37633864427922,9.37148720986523,-5.46639478469158));
#9594=CARTESIAN_POINT('Ctrl Pts',(5.59685221872653,9.41658919703079,-6.26210837834233));
#9595=CARTESIAN_POINT('Ctrl Pts',(3.79296005377837,9.50806897776786,-7.49002209394443));
#9596=CARTESIAN_POINT('Ctrl Pts',(2.79116570028853,9.5535372772894,-7.91811515677167));
#9597=CARTESIAN_POINT('Ctrl Pts',(1.1637569824839,9.62007369357247,-8.26497315555356));
#9598=CARTESIAN_POINT('Ctrl Pts',(0.582049594485062,9.64253350371268,-8.32600000000002));
#9599=CARTESIAN_POINT('Ctrl Pts',(-2.13024042849952E-13,9.66372307941295,
-8.326));
#9600=CARTESIAN_POINT('Ctrl Pts',(2.65829025458686E-13,9.26277469534532,
-8.326));
#9601=CARTESIAN_POINT('Ctrl Pts',(0.270011332909717,9.25294490483806,-8.326));
#9602=CARTESIAN_POINT('Ctrl Pts',(0.540330328713359,9.24282785542697,-8.31286592986294));
#9603=CARTESIAN_POINT('Ctrl Pts',(1.8722686141496,9.19160195337279,-8.18266865276879));
#9604=CARTESIAN_POINT('Ctrl Pts',(2.90463882928701,9.14756312398022,-7.8755446403364));
#9605=CARTESIAN_POINT('Ctrl Pts',(4.83447661738027,9.05614783747807,-6.86884359444069));
#9606=CARTESIAN_POINT('Ctrl Pts',(5.70577910102292,9.00961768353316,-6.16421198346843));
#9607=CARTESIAN_POINT('Ctrl Pts',(7.08966225860657,8.92410304413962,-4.49262570933537));
#9608=CARTESIAN_POINT('Ctrl Pts',(7.60365014163406,8.88717781687242,-3.55408682810106));
#9609=CARTESIAN_POINT('Ctrl Pts',(8.25764608625664,8.80151508631727,-1.51629284352452));
#9610=CARTESIAN_POINT('Ctrl Pts',(8.38447345847686,8.75601581466154,-0.43393016979451));
#9611=CARTESIAN_POINT('Ctrl Pts',(8.21608442769125,8.66454493988926,1.74203126836012));
#9612=CARTESIAN_POINT('Ctrl Pts',(7.91332388916238,8.61948379405422,2.8139715547111));
#9613=CARTESIAN_POINT('Ctrl Pts',(6.93008815760916,8.53879162550238,4.73352297003514));
#9614=CARTESIAN_POINT('Ctrl Pts',(6.27607052332773,8.49914701973004,5.5716960307008));
#9615=CARTESIAN_POINT('Ctrl Pts',(4.66108897497509,8.41064917972435,6.98494031216529));
#9616=CARTESIAN_POINT('Ctrl Pts',(3.70562210090701,8.36429372470061,7.53548324720289));
#9617=CARTESIAN_POINT('Ctrl Pts',(1.63032274656187,8.27396701813399,8.23844594669925));
#9618=CARTESIAN_POINT('Ctrl Pts',(0.530057311503819,8.23323680801519,8.38144266320653));
#9619=CARTESIAN_POINT('Ctrl Pts',(-1.62792472637798,8.15158384599891,8.23436255608475));
#9620=CARTESIAN_POINT('Ctrl Pts',(-2.66594668201158,8.10800889182977,7.95909750311635));
#9621=CARTESIAN_POINT('Ctrl Pts',(-4.61960871021218,8.01703365213557,7.01459742138488));
#9622=CARTESIAN_POINT('Ctrl Pts',(-5.50951373087223,7.97044961766743,6.33962286832511));
#9623=CARTESIAN_POINT('Ctrl Pts',(-6.94681990713011,7.88390665710639,4.7116433937412));
#9624=CARTESIAN_POINT('Ctrl Pts',(-7.49217320594941,7.84687913003538,3.78486720922831));
#9625=CARTESIAN_POINT('Ctrl Pts',(-8.20749596222921,7.76200248643653,1.76577311036096));
#9626=CARTESIAN_POINT('Ctrl Pts',(-8.36678981857217,7.716824612001,0.691056017360496));
#9627=CARTESIAN_POINT('Ctrl Pts',(-8.26624484813637,7.62530659708561,-1.48602681745564));
#9628=CARTESIAN_POINT('Ctrl Pts',(-7.99687043893497,7.57986552404543,-2.56700502926336));
#9629=CARTESIAN_POINT('Ctrl Pts',(-7.07362642223966,7.497927502703,-4.51619350268564));
#9630=CARTESIAN_POINT('Ctrl Pts',(-6.44602993909129,7.45948712400998,-5.37412175554442));
#9631=CARTESIAN_POINT('Ctrl Pts',(-4.87837176501689,7.3717232907501,-6.83441058184061));
#9632=CARTESIAN_POINT('Ctrl Pts',(-3.94382848183897,7.3255382517794,-7.4130863304762));
#9633=CARTESIAN_POINT('Ctrl Pts',(-1.98841059853127,7.2389325423352,-8.14665541703044));
#9634=CARTESIAN_POINT('Ctrl Pts',(-0.997760808690797,7.19909828080406,-8.32600000000001));
#9635=CARTESIAN_POINT('Ctrl Pts',(2.78110867668602E-13,7.16277469534532,
-8.32600000000001));
#9636=CARTESIAN_POINT('Origin',(0.,-25.4,0.));
#9637=CARTESIAN_POINT('',(-1.48126560903206E-15,5.06277469534534,-8.32600000000001));
#9638=CARTESIAN_POINT('',(2.12097888753232E-13,5.46372307941294,-8.326));
#9639=CARTESIAN_POINT('',(-1.01964092497009E-15,-25.4,-8.326));
#9640=CARTESIAN_POINT('Ctrl Pts',(2.66869859544272E-13,5.46372307941295,
-8.32600000000001));
#9641=CARTESIAN_POINT('Ctrl Pts',(-0.836238710997287,5.49416643619563,-8.32600000000001));
#9642=CARTESIAN_POINT('Ctrl Pts',(-1.6691076352286,5.52713480092555,-8.20003069430066));
#9643=CARTESIAN_POINT('Ctrl Pts',(-3.51605227828332,5.60643469280897,-7.6261703701439));
#9644=CARTESIAN_POINT('Ctrl Pts',(-4.48736206739596,5.65289217823176,-7.09821385403226));
#9645=CARTESIAN_POINT('Ctrl Pts',(-6.13926504489025,5.74194958478934,-5.72229678595137));
#9646=CARTESIAN_POINT('Ctrl Pts',(-6.81406939673126,5.78277185299237,-4.89928546051299));
#9647=CARTESIAN_POINT('Ctrl Pts',(-7.8434923195373,5.86248277281707,-3.0030765506242));
#9648=CARTESIAN_POINT('Ctrl Pts',(-8.1718573836664,5.90721963796853,-1.93885043847795));
#9649=CARTESIAN_POINT('Ctrl Pts',(-8.39273444303584,5.99859283259092,0.234787328453905));
#9650=CARTESIAN_POINT('Ctrl Pts',(-8.29123071882295,6.0443129058275,1.32240255636142));
#9651=CARTESIAN_POINT('Ctrl Pts',(-7.68470419092934,6.13056937921356,3.37432083468098));
#9652=CARTESIAN_POINT('Ctrl Pts',(-7.19448788927728,6.16764968623736,4.3220352924857));
#9653=CARTESIAN_POINT('Ctrl Pts',(-5.8516413287853,6.25235984893773,6.02642433519535));
#9654=CARTESIAN_POINT('Ctrl Pts',(-4.99515856122614,6.29881886716971,6.75334001340205));
#9655=CARTESIAN_POINT('Ctrl Pts',(-3.08477432069922,6.39051447046153,7.80707226401682));
#9656=CARTESIAN_POINT('Ctrl Pts',(-2.05735958893951,6.43488191143801,8.13841382570729));
#9657=CARTESIAN_POINT('Ctrl Pts',(0.0780813666116063,6.51802730695115,8.39554195436847));
#9658=CARTESIAN_POINT('Ctrl Pts',(1.16639161912466,6.55642742029657,8.31449901901567));
#9659=CARTESIAN_POINT('Ctrl Pts',(3.26797984233654,6.64509040181786,7.73622526022656));
#9660=CARTESIAN_POINT('Ctrl Pts',(4.25898323384728,6.69163818482159,7.23808296314459));
#9661=CARTESIAN_POINT('Ctrl Pts',(5.95801836496231,6.7813807989042,5.91120096349971));
#9662=CARTESIAN_POINT('Ctrl Pts',(6.65988782344491,6.82382491694228,5.10750465853079));
#9663=CARTESIAN_POINT('Ctrl Pts',(7.74794429048108,6.90265681557172,3.2414772381525));
#9664=CARTESIAN_POINT('Ctrl Pts',(8.10874982004316,6.94674901219425,2.18793166761265));
#9665=CARTESIAN_POINT('Ctrl Pts',(8.39641154396656,7.03793848012301,0.0186644962552045));
#9666=CARTESIAN_POINT('Ctrl Pts',(8.32736417643051,7.08390407115339,-1.07479124922758));
#9667=CARTESIAN_POINT('Ctrl Pts',(7.78132089306779,7.17089779552674,-3.14424767531945));
#9668=CARTESIAN_POINT('Ctrl Pts',(7.32079618340722,7.20846408878987,-4.10378319334718));
#9669=CARTESIAN_POINT('Ctrl Pts',(6.03717307551937,7.2916631814244,-5.83885786857691));
#9670=CARTESIAN_POINT('Ctrl Pts',(5.21116882224519,7.33745006928877,-6.58658583954571));
#9671=CARTESIAN_POINT('Ctrl Pts',(3.34192411406301,7.42892306594443,-7.70098286265292));
#9672=CARTESIAN_POINT('Ctrl Pts',(2.32265069959541,7.47372640841552,-8.06716454721469));
#9673=CARTESIAN_POINT('Ctrl Pts',(0.843407827322808,7.53234586696614,-8.29398708937408));
#9674=CARTESIAN_POINT('Ctrl Pts',(0.421555332686322,7.54837631391661,-8.326));
#9675=CARTESIAN_POINT('Ctrl Pts',(3.47361028829596E-13,7.56372307941294,
-8.326));
#9676=CARTESIAN_POINT('Ctrl Pts',(3.17176840347599E-13,7.16277469534532,
-8.326));
#9677=CARTESIAN_POINT('Ctrl Pts',(0.110531407005316,7.15875078803883,-8.326));
#9678=CARTESIAN_POINT('Ctrl Pts',(0.221146764566538,7.15467756251844,-8.32379898692281));
#9679=CARTESIAN_POINT('Ctrl Pts',(1.39221484264702,7.11106308580878,-8.27709620822705));
#9680=CARTESIAN_POINT('Ctrl Pts',(2.43474869707119,7.0679673551769,-8.03244607989538));
#9681=CARTESIAN_POINT('Ctrl Pts',(4.40943191700961,6.97749051763201,-7.14806832054697));
#9682=CARTESIAN_POINT('Ctrl Pts',(5.31626753571269,6.9308967450319,-6.50195511100492));
#9683=CARTESIAN_POINT('Ctrl Pts',(6.80437648512559,6.84339711469949,-4.91645300631127));
#9684=CARTESIAN_POINT('Ctrl Pts',(7.38004618128376,6.80595372948799,-4.00073896649165));
#9685=CARTESIAN_POINT('Ctrl Pts',(8.15325004613083,6.72183798589981,-1.99974559187804));
#9686=CARTESIAN_POINT('Ctrl Pts',(8.34287163849979,6.67700016300087,-0.933117839145429));
#9687=CARTESIAN_POINT('Ctrl Pts',(8.30627021956783,6.58551942388972,1.24307825753891));
#9688=CARTESIAN_POINT('Ctrl Pts',(8.06866161818484,6.5397608817083,2.33160860668945));
#9689=CARTESIAN_POINT('Ctrl Pts',(7.20237143688086,6.45667104581957,4.30819710271847));
#9690=CARTESIAN_POINT('Ctrl Pts',(6.59931472806746,6.41904313295165,5.18497119551834));
#9691=CARTESIAN_POINT('Ctrl Pts',(5.07590919889841,6.33198158776267,6.68849499128344));
#9692=CARTESIAN_POINT('Ctrl Pts',(4.16151989849957,6.28599510059205,7.29263193471018));
#9693=CARTESIAN_POINT('Ctrl Pts',(2.1363687615072,6.19482687975152,8.12249073939595));
#9694=CARTESIAN_POINT('Ctrl Pts',(1.04292815878845,6.15090401440863,8.33367950045313));
#9695=CARTESIAN_POINT('Ctrl Pts',(-1.11743517016165,6.07193069835686,8.31821380931037));
#9696=CARTESIAN_POINT('Ctrl Pts',(-2.16408733753655,6.02943213951944,8.10910853602593));
#9697=CARTESIAN_POINT('Ctrl Pts',(-4.16089487781268,5.93962602065705,7.2949621021605));
#9698=CARTESIAN_POINT('Ctrl Pts',(-5.08623646770629,5.89307213146327,6.68279971348423));
#9699=CARTESIAN_POINT('Ctrl Pts',(-6.63273819124001,5.80450107051947,5.14746125310297));
#9700=CARTESIAN_POINT('Ctrl Pts',(-7.24394210984032,5.76619557337075,4.24437780125603));
#9701=CARTESIAN_POINT('Ctrl Pts',(-8.08323842736825,5.68297152755918,2.26459664289444));
#9702=CARTESIAN_POINT('Ctrl Pts',(-8.30704860044801,5.63856454044485,1.208217857998));
#9703=CARTESIAN_POINT('Ctrl Pts',(-8.3433565962951,5.54683726336699,-0.97384302471674));
#9704=CARTESIAN_POINT('Ctrl Pts',(-8.13873009131252,5.50038896906575,-2.07878159143743));
#9705=CARTESIAN_POINT('Ctrl Pts',(-7.32800466069326,5.41578061817603,-4.09149339003265));
#9706=CARTESIAN_POINT('Ctrl Pts',(-6.74987920718193,5.37866651333336,-4.98790357997048));
#9707=CARTESIAN_POINT('Ctrl Pts',(-5.27161683067499,5.29233616772912,-6.53482922266064));
#9708=CARTESIAN_POINT('Ctrl Pts',(-4.37832878617842,5.24659002303265,-7.16407980518596));
#9709=CARTESIAN_POINT('Ctrl Pts',(-2.38249229096588,5.15523291310326,-8.05369986200487));
#9710=CARTESIAN_POINT('Ctrl Pts',(-1.29593786950077,5.11053874562274,-8.29815318994175));
#9711=CARTESIAN_POINT('Ctrl Pts',(-0.128827677076796,5.06748038441164,-8.32525284116874));
#9712=CARTESIAN_POINT('Ctrl Pts',(-0.0643990695313742,5.06511915013371,
-8.326));
#9713=CARTESIAN_POINT('Ctrl Pts',(2.80624040585213E-13,5.06277469534533,
-8.326));
#9714=CARTESIAN_POINT('Origin',(0.,-25.4,0.));
#9715=CARTESIAN_POINT('',(-1.87582400111824E-13,2.96277469534536,-8.326));
#9716=CARTESIAN_POINT('',(-8.53327934765894E-14,3.36372307941297,-8.326));
#9717=CARTESIAN_POINT('',(-1.01964092497009E-15,-25.4,-8.326));
#9718=CARTESIAN_POINT('Ctrl Pts',(-1.18793863634892E-13,3.36372307941297,
-8.32599999999999));
#9719=CARTESIAN_POINT('Ctrl Pts',(-1.01836376702856,3.40079671770132,-8.32599999999997));
#9720=CARTESIAN_POINT('Ctrl Pts',(-2.02901965751839,3.44151663238114,-8.13917015344795));
#9721=CARTESIAN_POINT('Ctrl Pts',(-3.99734367168246,3.52904090918155,-7.38425233093585));
#9722=CARTESIAN_POINT('Ctrl Pts',(-4.92702575069337,3.57518100252677,-6.79929511414191));
#9723=CARTESIAN_POINT('Ctrl Pts',(-6.48389859140411,3.66277504659142,-5.3284036272797));
#9724=CARTESIAN_POINT('Ctrl Pts',(-7.10550172745547,3.70098935641988,-4.46591707897539));
#9725=CARTESIAN_POINT('Ctrl Pts',(-8.01494287944838,3.78320932991601,-2.51002136660578));
#9726=CARTESIAN_POINT('Ctrl Pts',(-8.27662251212905,3.82873120460592,-1.42712099898192));
#9727=CARTESIAN_POINT('Ctrl Pts',(-8.36162443406572,3.92024745868604,0.749919948078396));
#9728=CARTESIAN_POINT('Ctrl Pts',(-8.19493445769682,3.96534599110138,1.82274960776392));
#9729=CARTESIAN_POINT('Ctrl Pts',(-7.46555349515448,4.05003955738955,3.83748855894897));
#9730=CARTESIAN_POINT('Ctrl Pts',(-6.91290358877263,4.08713924640636,4.76157456578563));
#9731=CARTESIAN_POINT('Ctrl Pts',(-5.46329019484257,4.17391595682806,6.37935846457562));
#9732=CARTESIAN_POINT('Ctrl Pts',(-4.56921462651943,4.22050609686749,7.04739990282447));
#9733=CARTESIAN_POINT('Ctrl Pts',(-2.61031192483623,4.311367800571,7.97742115377031));
#9734=CARTESIAN_POINT('Ctrl Pts',(-1.57111891415557,4.35483008732094,8.24529748599969));
#9735=CARTESIAN_POINT('Ctrl Pts',(0.589739027879327,4.43628138737034,8.37780188080297));
#9736=CARTESIAN_POINT('Ctrl Pts',(1.69164942547461,4.47740058732764,8.22642886267737));
#9737=CARTESIAN_POINT('Ctrl Pts',(3.76316894793577,4.56794020341399,7.50678967567851));
#9738=CARTESIAN_POINT('Ctrl Pts',(4.71368626587519,4.61425885797127,6.94942471900162));
#9739=CARTESIAN_POINT('Ctrl Pts',(6.31733377238988,4.70258257366624,5.52483363842384));
#9740=CARTESIAN_POINT('Ctrl Pts',(6.96500296712227,4.74190739602998,4.6819639424229));
#9741=CARTESIAN_POINT('Ctrl Pts',(7.93395357776352,4.82289919832966,2.75528466828652));
#9742=CARTESIAN_POINT('Ctrl Pts',(8.22877510544623,4.86805504852651,1.68109150046035));
#9743=CARTESIAN_POINT('Ctrl Pts',(8.38097082524413,4.95954527861263,-0.49533037295973));
#9744=CARTESIAN_POINT('Ctrl Pts',(8.2463670677231,5.00497152327706,-1.57595583889112));
#9745=CARTESIAN_POINT('Ctrl Pts',(7.57773447837673,5.090448545739,-3.60933209322709));
#9746=CARTESIAN_POINT('Ctrl Pts',(7.05632880145078,5.12736695766995,-4.54505674397575));
#9747=CARTESIAN_POINT('Ctrl Pts',(5.6597358437157,5.21312822444436,-6.20636282462398));
#9748=CARTESIAN_POINT('Ctrl Pts',(4.78393547707342,5.25967520081863,-6.90400423683939));
#9749=CARTESIAN_POINT('Ctrl Pts',(2.84827344830574,5.35099353959103,-7.89600490598302));
#9750=CARTESIAN_POINT('Ctrl Pts',(1.81447574080089,5.39492571590364,-8.19558218028575));
#9751=CARTESIAN_POINT('Ctrl Pts',(0.501719643319216,5.44521990738753,-8.31467585461312));
#9752=CARTESIAN_POINT('Ctrl Pts',(0.250717041383125,5.45459569958473,-8.326));
#9753=CARTESIAN_POINT('Ctrl Pts',(2.86368151414251E-13,5.46372307941295,
-8.326));
#9754=CARTESIAN_POINT('Ctrl Pts',(2.80886425230165E-13,5.06277469534533,
-8.326));
#9755=CARTESIAN_POINT('Ctrl Pts',(0.98938994559301,5.02675585202358,-8.326));
#9756=CARTESIAN_POINT('Ctrl Pts',(1.97154206318376,4.98729387796089,-8.14964939102314));
#9757=CARTESIAN_POINT('Ctrl Pts',(3.92683794662508,4.90083922264985,-7.42305571857651));
#9758=CARTESIAN_POINT('Ctrl Pts',(4.86819512279073,4.85437079776511,-6.84269928667721));
#9759=CARTESIAN_POINT('Ctrl Pts',(6.46817564592858,4.76484721600004,-5.35467060515037));
#9760=CARTESIAN_POINT('Ctrl Pts',(7.112642278346,4.72539283222041,-4.46316745034782));
#9761=CARTESIAN_POINT('Ctrl Pts',(8.01214487047178,4.6430021741349,-2.50321139543531));
#9762=CARTESIAN_POINT('Ctrl Pts',(8.26662695749645,4.59902593358394,-1.45707945592931));
#9763=CARTESIAN_POINT('Ctrl Pts',(8.3689375242085,4.50766721207635,0.716214016276809));
#9764=CARTESIAN_POINT('Ctrl Pts',(8.19925236532742,4.46112684145986,1.82334294699955));
#9765=CARTESIAN_POINT('Ctrl Pts',(7.45254564987965,4.37546667437354,3.86107595031696));
#9766=CARTESIAN_POINT('Ctrl Pts',(6.90036360677415,4.33854782460159,4.77842564798735));
#9767=CARTESIAN_POINT('Ctrl Pts',(5.46914904938857,4.25299445984832,6.3698739748369));
#9768=CARTESIAN_POINT('Ctrl Pts',(4.5983844945359,4.20753797265641,7.02435530931477));
#9769=CARTESIAN_POINT('Ctrl Pts',(2.63427890012778,4.11605506929538,7.97491979056402));
#9770=CARTESIAN_POINT('Ctrl Pts',(1.55575398765627,4.07093777131744,8.25341197616064));
#9771=CARTESIAN_POINT('Ctrl Pts',(-0.597677104968653,3.9900687341678,8.37107764632682));
#9772=CARTESIAN_POINT('Ctrl Pts',(-1.65108899359419,3.95061517335544,8.22839756708033));
#9773=CARTESIAN_POINT('Ctrl Pts',(-3.68494463374718,3.86221993194998,7.54554584284826));
#9774=CARTESIAN_POINT('Ctrl Pts',(-4.64149569507564,3.81588587958301,6.9978990524894));
#9775=CARTESIAN_POINT('Ctrl Pts',(-6.29534005757804,3.72543324975436,5.55896382499089));
#9776=CARTESIAN_POINT('Ctrl Pts',(-6.9740746221251,3.68447564688011,4.67923463565191));
#9777=CARTESIAN_POINT('Ctrl Pts',(-7.933993206594,3.60294162668782,2.73965677245104));
#9778=CARTESIAN_POINT('Ctrl Pts',(-8.21874543774091,3.55943297781633,1.7046481710116));
#9779=CARTESIAN_POINT('Ctrl Pts',(-8.38657213518008,3.46852426640382,-0.457940203903986));
#9780=CARTESIAN_POINT('Ctrl Pts',(-8.25175791078302,3.42193633662906,-1.56620049906026));
#9781=CARTESIAN_POINT('Ctrl Pts',(-7.56938605684569,3.33525511430828,-3.62822294775514));
#9782=CARTESIAN_POINT('Ctrl Pts',(-7.0429821529524,3.29818716034735,-4.5668361622465));
#9783=CARTESIAN_POINT('Ctrl Pts',(-5.65843785820305,3.21341859132525,-6.20178141656848));
#9784=CARTESIAN_POINT('Ctrl Pts',(-4.81050026118659,3.16828735903497,-6.88032550288151));
#9785=CARTESIAN_POINT('Ctrl Pts',(-2.87942229464534,3.07676981877775,-7.8897434382078));
#9786=CARTESIAN_POINT('Ctrl Pts',(-1.8098638956802,3.03128070198162,-8.20145615779368));
#9787=CARTESIAN_POINT('Ctrl Pts',(-0.473919123104029,2.98024015797251,-8.31589518941546));
#9788=CARTESIAN_POINT('Ctrl Pts',(-0.236834098017002,2.97139666518413,-8.326));
#9789=CARTESIAN_POINT('Ctrl Pts',(-1.73680514414798E-13,2.96277469534536,
-8.326));
#9790=CARTESIAN_POINT('Origin',(0.,-25.4,0.));
#9791=CARTESIAN_POINT('',(-1.6746832197628E-14,0.862774695345363,-8.32600000000001));
#9792=CARTESIAN_POINT('',(-5.1302523839086E-14,1.26372307941298,-8.326));
#9793=CARTESIAN_POINT('',(-1.01964092497009E-15,-25.4,-8.326));
#9794=CARTESIAN_POINT('Ctrl Pts',(-1.69645946028209E-13,1.26372307941299,
-8.326));
#9795=CARTESIAN_POINT('Ctrl Pts',(-0.0837768214034725,1.26677298326288,
-8.326));
#9796=CARTESIAN_POINT('Ctrl Pts',(-0.167601579300017,1.26985120902554,-8.32473555275498));
#9797=CARTESIAN_POINT('Ctrl Pts',(-1.3539457410103,1.31379357929034,-8.28889148852802));
#9798=CARTESIAN_POINT('Ctrl Pts',(-2.43880631725384,1.35858594554283,-8.03683231760474));
#9799=CARTESIAN_POINT('Ctrl Pts',(-4.42773562785666,1.44997899855494,-7.13353859692295));
#9800=CARTESIAN_POINT('Ctrl Pts',(-5.31606588894694,1.49566420549788,-6.49860012585041));
#9801=CARTESIAN_POINT('Ctrl Pts',(-6.78387820388031,1.58182325722266,-4.94172411894643));
#9802=CARTESIAN_POINT('Ctrl Pts',(-7.35624026525427,1.61886395956457,-4.04070580530918));
#9803=CARTESIAN_POINT('Ctrl Pts',(-8.15281686088358,1.70370780369458,-2.02239195894645));
#9804=CARTESIAN_POINT('Ctrl Pts',(-8.34970350508474,1.75018032569696,-0.916877049826637));
#9805=CARTESIAN_POINT('Ctrl Pts',(-8.29874479024791,1.84183306570532,1.26341070248638));
#9806=CARTESIAN_POINT('Ctrl Pts',(-8.06811115217157,1.88614789682518,2.31759722792569));
#9807=CARTESIAN_POINT('Ctrl Pts',(-7.21550118058259,1.96918938584951,4.29303562111409));
#9808=CARTESIAN_POINT('Ctrl Pts',(-6.59701641921928,2.00771898813145,5.19356725068109));
#9809=CARTESIAN_POINT('Ctrl Pts',(-5.03870961518502,2.09650276267898,6.71857901736009));
#9810=CARTESIAN_POINT('Ctrl Pts',(-4.10975467197251,2.14304184596436,7.32377847168283));
#9811=CARTESIAN_POINT('Ctrl Pts',(-2.10874593485223,2.23269950506558,8.12358492789594));
#9812=CARTESIAN_POINT('Ctrl Pts',(-1.0614027300489,2.27507127258183,8.32546092044366));
#9813=CARTESIAN_POINT('Ctrl Pts',(1.09821997672844,2.35371566105738,8.32655997253554));
#9814=CARTESIAN_POINT('Ctrl Pts',(2.19016207354498,2.39803518065504,8.1081431028105));
#9815=CARTESIAN_POINT('Ctrl Pts',(4.20907432661105,2.48925161014868,7.26518460420603));
#9816=CARTESIAN_POINT('Ctrl Pts',(5.11892502241012,2.53518909188473,6.65551810557873));
#9817=CARTESIAN_POINT('Ctrl Pts',(6.63252465185689,2.62209304366012,5.14250783763209));
#9818=CARTESIAN_POINT('Ctrl Pts',(7.23015926129918,2.65958222891784,4.26150491778023));
#9819=CARTESIAN_POINT('Ctrl Pts',(8.08371261568657,2.74292541938276,2.27888947831906));
#9820=CARTESIAN_POINT('Ctrl Pts',(8.31421456842586,2.7887492107285,1.18880694476285));
#9821=CARTESIAN_POINT('Ctrl Pts',(8.33658991899218,2.88021085400004,-0.986934889176645));
#9822=CARTESIAN_POINT('Ctrl Pts',(8.14025679028578,2.92496811769043,-2.05164625342269));
#9823=CARTESIAN_POINT('Ctrl Pts',(7.35415411630031,3.00891174121332,-4.04854513756839));
#9824=CARTESIAN_POINT('Ctrl Pts',(6.77162781890511,3.04649077030201,-4.96179654281381));
#9825=CARTESIAN_POINT('Ctrl Pts',(5.27215257541828,3.13420139337505,-6.53765008044056));
#9826=CARTESIAN_POINT('Ctrl Pts',(4.36163341616348,3.18079171921284,-7.17721922349229));
#9827=CARTESIAN_POINT('Ctrl Pts',(2.3824705566221,3.27114625086254,-8.04801905440062));
#9828=CARTESIAN_POINT('Ctrl Pts',(1.33904462603134,3.3141296388214,-8.285779118084));
#9829=CARTESIAN_POINT('Ctrl Pts',(0.185981993360484,3.35691966319102,-8.32444315628126));
#9830=CARTESIAN_POINT('Ctrl Pts',(0.0929600549114514,3.36033885899719,-8.326));
#9831=CARTESIAN_POINT('Ctrl Pts',(-1.69645946028209E-13,3.36372307941297,
-8.326));
#9832=CARTESIAN_POINT('Ctrl Pts',(-1.82076576038526E-13,2.96277469534536,
-8.326));
#9833=CARTESIAN_POINT('Ctrl Pts',(0.813556815714888,2.93315707530678,-8.32600000000002));
#9834=CARTESIAN_POINT('Ctrl Pts',(1.62397012934317,2.90114791058247,-8.20677243150924));
#9835=CARTESIAN_POINT('Ctrl Pts',(3.44723056130226,2.82320780122122,-7.65658441771259));
#9836=CARTESIAN_POINT('Ctrl Pts',(4.41743669168115,2.77704906892423,-7.14093012874506));
#9837=CARTESIAN_POINT('Ctrl Pts',(6.12293048574269,2.685736751059,-5.75055284036092));
#9838=CARTESIAN_POINT('Ctrl Pts',(6.83531027266515,2.643012464414,-4.88231332932904));
#9839=CARTESIAN_POINT('Ctrl Pts',(7.85303680208091,2.56231749481875,-2.96269528118814));
#9840=CARTESIAN_POINT('Ctrl Pts',(8.1662290676751,2.51928806067112,-1.9390865134368));
#9841=CARTESIAN_POINT('Ctrl Pts',(8.3959665744779,2.42888316692028,0.211516759046871));
#9842=CARTESIAN_POINT('Ctrl Pts',(8.29427947588552,2.38229118501643,1.31987344856551));
#9843=CARTESIAN_POINT('Ctrl Pts',(7.67355633196759,2.29466647743399,3.404340063799));
#9844=CARTESIAN_POINT('Ctrl Pts',(7.17165113038443,2.2571446505772,4.36352557621024));
#9845=CARTESIAN_POINT('Ctrl Pts',(5.83126000942862,2.17313074369003,6.03904170265549));
#9846=CARTESIAN_POINT('Ctrl Pts',(5.00531155999211,2.12834042858072,6.73945224437031));
#9847=CARTESIAN_POINT('Ctrl Pts',(3.10680679284471,2.03687052649224,7.80302212805181));
#9848=CARTESIAN_POINT('Ctrl Pts',(2.04661048153777,1.99107309342936,8.14561926619544));
#9849=CARTESIAN_POINT('Ctrl Pts',(-0.0976340101182796,1.90783304287678,
8.39200263937633));
#9850=CARTESIAN_POINT('Ctrl Pts',(-1.15903231784563,1.87028914896897,8.31216195281203));
#9851=CARTESIAN_POINT('Ctrl Pts',(-3.22479127438158,1.78332090368117,7.75246079163234));
#9852=CARTESIAN_POINT('Ctrl Pts',(-4.2066826292331,1.73736323871729,7.2666121143808));
#9853=CARTESIAN_POINT('Ctrl Pts',(-5.94282182088796,1.64616598469532,5.93478862055471));
#9854=CARTESIAN_POINT('Ctrl Pts',(-6.67570707028367,1.60200963702447,5.09634321262818));
#9855=CARTESIAN_POINT('Ctrl Pts',(-7.74965742290837,1.5232309206312,3.22231009065765));
#9856=CARTESIAN_POINT('Ctrl Pts',(-8.09581206121049,1.48080730375074,2.21311285023932));
#9857=CARTESIAN_POINT('Ctrl Pts',(-8.39775521983311,1.39108869823119,0.0788353943661968));
#9858=CARTESIAN_POINT('Ctrl Pts',(-8.33492431754466,1.34454331319512,-1.02841282223466));
#9859=CARTESIAN_POINT('Ctrl Pts',(-7.78733004158013,1.25584594677796,-3.13839645877649));
#9860=CARTESIAN_POINT('Ctrl Pts',(-7.31430595671989,1.21740957143647,-4.12223537722999));
#9861=CARTESIAN_POINT('Ctrl Pts',(-6.02559014343174,1.13429368963372,-5.84453029432095));
#9862=CARTESIAN_POINT('Ctrl Pts',(-5.22579107191315,1.08994115003569,-6.56940477934618));
#9863=CARTESIAN_POINT('Ctrl Pts',(-3.39229921268728,0.999870221400379,-7.67902116285679));
#9864=CARTESIAN_POINT('Ctrl Pts',(-2.37477190565768,0.954986193959591,-8.05206595434195));
#9865=CARTESIAN_POINT('Ctrl Pts',(-0.878764722238898,0.895496747091505,
-8.29124341631015));
#9866=CARTESIAN_POINT('Ctrl Pts',(-0.43924976329083,0.878765628418327,-8.32599999999999));
#9867=CARTESIAN_POINT('Ctrl Pts',(-2.1163626406917E-13,0.862774695345371,
-8.326));
#9868=CARTESIAN_POINT('Origin',(0.,-25.4,0.));
#9869=CARTESIAN_POINT('',(1.71843589924784E-14,-1.23722530465463,-8.326));
#9870=CARTESIAN_POINT('',(-1.91468180698012E-13,-0.836276920586999,-8.326));
#9871=CARTESIAN_POINT('',(-1.01964092497009E-15,-25.4,-8.326));
#9872=CARTESIAN_POINT('Ctrl Pts',(-2.39808173319034E-13,-0.836276920587004,
-8.326));
#9873=CARTESIAN_POINT('Ctrl Pts',(-0.255368949442104,-0.826980187564671,
-8.326));
#9874=CARTESIAN_POINT('Ctrl Pts',(-0.511010728906746,-0.817426591330658,
-8.31425173774534));
#9875=CARTESIAN_POINT('Ctrl Pts',(-1.86474347872633,-0.765514493499206,
-8.1891563457596));
#9876=CARTESIAN_POINT('Ctrl Pts',(-2.93221896013381,-0.719950607316501,
-7.87027859334921));
#9877=CARTESIAN_POINT('Ctrl Pts',(-4.85590214026335,-0.628437197390175,
-6.84824902158977));
#9878=CARTESIAN_POINT('Ctrl Pts',(-5.69880496181663,-0.583381716280099,
-6.16458847309249));
#9879=CARTESIAN_POINT('Ctrl Pts',(-7.07317588236123,-0.498785972970789,
-4.52024497139059));
#9880=CARTESIAN_POINT('Ctrl Pts',(-7.59394586307286,-0.46164039435956,-3.57693223608604));
#9881=CARTESIAN_POINT('Ctrl Pts',(-8.26218083383954,-0.37473971366601,-1.50968918621494));
#9882=CARTESIAN_POINT('Ctrl Pts',(-8.38937147905276,-0.328147295434776,
-0.401322117091165));
#9883=CARTESIAN_POINT('Ctrl Pts',(-8.20726869881849,-0.237347928498029,
1.75866510895241));
#9884=CARTESIAN_POINT('Ctrl Pts',(-7.91594414736932,-0.193946534618926,
2.79112226734456));
#9885=CARTESIAN_POINT('Ctrl Pts',(-6.94276165816964,-0.112603341226765,
4.72616063358038));
#9886=CARTESIAN_POINT('Ctrl Pts',(-6.25638197848218,-0.0712687203542418,
5.60327588765145));
#9887=CARTESIAN_POINT('Ctrl Pts',(-4.59069347327753,0.0193838465750226,
7.03120889421505));
#9888=CARTESIAN_POINT('Ctrl Pts',(-3.63093094664952,0.0656817477729541,
7.57157329417422));
#9889=CARTESIAN_POINT('Ctrl Pts',(-1.59316574834101,0.153911777804031,8.23979317988505));
#9890=CARTESIAN_POINT('Ctrl Pts',(-0.538895882621613,0.193073454439265,
8.37505510863373));
#9891=CARTESIAN_POINT('Ctrl Pts',(1.61359623483333,0.27422539722241,8.242303244025));
#9892=CARTESIAN_POINT('Ctrl Pts',(2.69017757877837,0.31943101084386,7.95624289300489));
#9893=CARTESIAN_POINT('Ctrl Pts',(4.64693956999572,0.4109295297381,6.99221597546405));
#9894=CARTESIAN_POINT('Ctrl Pts',(5.51257792110755,0.456315648234544,6.33220373713382));
#9895=CARTESIAN_POINT('Ctrl Pts',(6.93322897944752,0.541692550568771,4.73085447095174));
#9896=CARTESIAN_POINT('Ctrl Pts',(7.47958407163772,0.578615355971894,3.80873401534467));
#9897=CARTESIAN_POINT('Ctrl Pts',(8.21180291906934,0.664508608103169,1.76545625178619));
#9898=CARTESIAN_POINT('Ctrl Pts',(8.37361188370897,0.711063595039071,0.657979619704897));
#9899=CARTESIAN_POINT('Ctrl Pts',(8.25647245025157,0.802327859707633,-1.51306685923906));
#9900=CARTESIAN_POINT('Ctrl Pts',(7.99512358570411,0.846201783309242,-2.55676482468719));
#9901=CARTESIAN_POINT('Ctrl Pts',(7.08200810399254,0.928401211867213,-4.5121718023247));
#9902=CARTESIAN_POINT('Ctrl Pts',(6.42989899223848,0.968163647926906,-5.40103844750506));
#9903=CARTESIAN_POINT('Ctrl Pts',(4.81779649078895,1.0578990590066,-6.87814948027013));
#9904=CARTESIAN_POINT('Ctrl Pts',(3.87293675512195,1.10434150518562,-7.45120330856285));
#9905=CARTESIAN_POINT('Ctrl Pts',(1.93192930928717,1.18983341635668,-8.15674066542193));
#9906=CARTESIAN_POINT('Ctrl Pts',(0.969300700853793,1.22843558712422,-8.32600000000001));
#9907=CARTESIAN_POINT('Ctrl Pts',(-2.25375273998907E-13,1.26372307941299,
-8.326));
#9908=CARTESIAN_POINT('Ctrl Pts',(-1.974809205052E-13,0.86277469534537,
-8.32600000000001));
#9909=CARTESIAN_POINT('Ctrl Pts',(0.626897877395358,0.839952413266184,-8.32600000000002));
#9910=CARTESIAN_POINT('Ctrl Pts',(1.25314594048656,0.815665821847271,-8.2552068339659));
#9911=CARTESIAN_POINT('Ctrl Pts',(2.94183309963131,0.74602281149041,-7.86668333894596));
#9912=CARTESIAN_POINT('Ctrl Pts',(3.95700950465341,0.69942798442542,-7.40817170741499));
#9913=CARTESIAN_POINT('Ctrl Pts',(5.71575539196035,0.608881692148581,-6.14647505899301));
#9914=CARTESIAN_POINT('Ctrl Pts',(6.45209755885893,0.565721351262088,-5.36841139969592));
#9915=CARTESIAN_POINT('Ctrl Pts',(7.61804276313728,0.484800491399616,-3.53790442254404));
#9916=CARTESIAN_POINT('Ctrl Pts',(8.02098224619923,0.442579217743075,-2.49314986709691));
#9917=CARTESIAN_POINT('Ctrl Pts',(8.39059674336028,0.351493380304156,-0.326347917050532));
#9918=CARTESIAN_POINT('Ctrl Pts',(8.36129455522583,0.305283315324501,0.772923514436969));
#9919=CARTESIAN_POINT('Ctrl Pts',(7.8889425125532,0.217421472437857,2.86303123979268));
#9920=CARTESIAN_POINT('Ctrl Pts',(7.4637722429967,0.178841792696816,3.83720615500331));
#9921=CARTESIAN_POINT('Ctrl Pts',(6.24471135935666,0.0970675653949035,5.61631486139091));
#9922=CARTESIAN_POINT('Ctrl Pts',(5.44645262225463,0.0516743286916036,6.39337067852439));
#9923=CARTESIAN_POINT('Ctrl Pts',(3.61583772491597,-0.0398425650265737,
7.5767649935127));
#9924=CARTESIAN_POINT('Ctrl Pts',(2.60667655209084,-0.0850653940335428,
7.98041956522313));
#9925=CARTESIAN_POINT('Ctrl Pts',(0.502323978040994,-0.170047473770475,
8.37877853787446));
#9926=CARTESIAN_POINT('Ctrl Pts',(-0.572212235113425,-0.207041635407368,
8.37429626480301));
#9927=CARTESIAN_POINT('Ctrl Pts',(-2.70226013375954,-0.293448947391339,
7.95263442165316));
#9928=CARTESIAN_POINT('Ctrl Pts',(-3.73399768157828,-0.340028369924945,
7.52354043446785));
#9929=CARTESIAN_POINT('Ctrl Pts',(-5.53447836288067,-0.431067133719925,
6.31070018191802));
#9930=CARTESIAN_POINT('Ctrl Pts',(-6.29521685254581,-0.474706202518919,
5.55211568688792));
#9931=CARTESIAN_POINT('Ctrl Pts',(-7.5080208242872,-0.556474917320835,3.76243196018632));
#9932=CARTESIAN_POINT('Ctrl Pts',(-7.93800651383442,-0.596989508342807,
2.7412949716939));
#9933=CARTESIAN_POINT('Ctrl Pts',(-8.37625091447417,-0.687192712219641,
0.595489613184537));
#9934=CARTESIAN_POINT('Ctrl Pts',(-8.38202861856108,-0.733568153513214,
-0.507715884559157));
#9935=CARTESIAN_POINT('Ctrl Pts',(-7.97453695305073,-0.82216555754434,-2.61532155874035));
#9936=CARTESIAN_POINT('Ctrl Pts',(-7.5798228992792,-0.86200280905928,-3.60262409777236));
#9937=CARTESIAN_POINT('Ctrl Pts',(-6.41670722618219,-0.942522461806419,
-5.41894367844299));
#9938=CARTESIAN_POINT('Ctrl Pts',(-5.64317509392435,-0.987528150287472,
-6.22038879433125));
#9939=CARTESIAN_POINT('Ctrl Pts',(-3.84785176083109,-1.07898562990653,-7.46208313858954));
#9940=CARTESIAN_POINT('Ctrl Pts',(-2.84847711250222,-1.12452574484206,-7.89778402590663));
#9941=CARTESIAN_POINT('Ctrl Pts',(-1.20336946459652,-1.19204472116218,-8.26073397776654));
#9942=CARTESIAN_POINT('Ctrl Pts',(-0.601927322205734,-1.21531207822038,
-8.32599999999999));
#9943=CARTESIAN_POINT('Ctrl Pts',(-1.81243908770057E-13,-1.23722530465462,
-8.326));
#9944=CARTESIAN_POINT('Origin',(0.,-25.4,0.));
#9945=CARTESIAN_POINT('',(1.68035912463422E-13,-3.33722530465466,-8.326));
#9946=CARTESIAN_POINT('',(-4.60289644721165E-14,-2.93627692058703,-8.326));
#9947=CARTESIAN_POINT('',(-1.01964092497009E-15,-25.4,-8.326));
#9948=CARTESIAN_POINT('Ctrl Pts',(-1.52516888007881E-13,-2.93627692058703,
-8.326));
#9949=CARTESIAN_POINT('Ctrl Pts',(-0.419347816656509,-2.92101051994014,
-8.326));
#9950=CARTESIAN_POINT('Ctrl Pts',(-0.838976472693165,-2.90506806032965,
-8.29432147418403));
#9951=CARTESIAN_POINT('Ctrl Pts',(-2.35405396764038,-2.84505473469001,-8.06325010554558));
#9952=CARTESIAN_POINT('Ctrl Pts',(-3.40812639263809,-2.79857044827765,-7.67736756524498));
#9953=CARTESIAN_POINT('Ctrl Pts',(-5.26618315455172,-2.70695816396692,-6.53696554210616));
#9954=CARTESIAN_POINT('Ctrl Pts',(-6.06103874368431,-2.66269210570163,-5.80764322935427));
#9955=CARTESIAN_POINT('Ctrl Pts',(-7.34007153167069,-2.5797462304383,-4.07666524588282));
#9956=CARTESIAN_POINT('Ctrl Pts',(-7.80765100377409,-2.54109299157087,-3.08813887717487));
#9957=CARTESIAN_POINT('Ctrl Pts',(-8.34142423238497,-2.45219871426703,-0.97347101194023));
#9958=CARTESIAN_POINT('Ctrl Pts',(-8.39697114654256,-2.40566826989119,0.133421787697617));
#9959=CARTESIAN_POINT('Ctrl Pts',(-8.08149228983829,-2.31607566197319,2.26470194062641));
#9960=CARTESIAN_POINT('Ctrl Pts',(-7.72908041097248,-2.27390250326293,3.27104224553266));
#9961=CARTESIAN_POINT('Ctrl Pts',(-6.64387894148651,-2.19515835887964,5.13783957042563));
#9962=CARTESIAN_POINT('Ctrl Pts',(-5.9057366629076,-2.15076126886918,5.97162633458237));
#9963=CARTESIAN_POINT('Ctrl Pts',(-4.16220688676714,-2.05953390545653,7.29208147936309));
#9964=CARTESIAN_POINT('Ctrl Pts',(-3.17798706527946,-2.01362295991409,7.77167435750885));
#9965=CARTESIAN_POINT('Ctrl Pts',(-1.10914838475207,-1.92680230808719,8.31901920508821));
#9966=CARTESIAN_POINT('Ctrl Pts',(-0.0468512596586299,-1.8893801589713,
8.39249445380201));
#9967=CARTESIAN_POINT('Ctrl Pts',(2.09630088469165,-1.80590378948209,8.13297569977981));
#9968=CARTESIAN_POINT('Ctrl Pts',(3.15440692553243,-1.76004638159588,7.78390467624997));
#9969=CARTESIAN_POINT('Ctrl Pts',(5.04585127685949,-1.66859639437445,6.70905328611966));
#9970=CARTESIAN_POINT('Ctrl Pts',(5.86709482506276,-1.62388233158846,6.00412148410425));
#9971=CARTESIAN_POINT('Ctrl Pts',(7.19812694415682,-1.54002990006924,4.32007762757575));
#9972=CARTESIAN_POINT('Ctrl Pts',(7.69482077893012,-1.50237294510652,3.35647285756903));
#9973=CARTESIAN_POINT('Ctrl Pts',(8.30237793912328,-1.41455134371416,1.26732241987429));
#9974=CARTESIAN_POINT('Ctrl Pts',(8.39703215218012,-1.36796367610518,0.159068361267252));
#9975=CARTESIAN_POINT('Ctrl Pts',(8.15419247908559,-1.27767534839152,-1.98876197171501));
#9976=CARTESIAN_POINT('Ctrl Pts',(7.83500228377835,-1.2347520572277,-3.00984574951449));
#9977=CARTESIAN_POINT('Ctrl Pts',(6.80494146750566,-1.15423861122331,-4.92514561074857));
#9978=CARTESIAN_POINT('Ctrl Pts',(6.08527294656668,-1.11109595639874,-5.79089739470389));
#9979=CARTESIAN_POINT('Ctrl Pts',(4.36875245723809,-1.01960431883729,-7.17070740544971));
#9980=CARTESIAN_POINT('Ctrl Pts',(3.39574973309031,-0.973488997974973,-7.67945245989225));
#9981=CARTESIAN_POINT('Ctrl Pts',(1.58727304806974,-0.896454993343481,-8.21213680034134));
#9982=CARTESIAN_POINT('Ctrl Pts',(0.795046098036533,-0.865220656033569,
-8.32600000000002));
#9983=CARTESIAN_POINT('Ctrl Pts',(-1.76803016671556E-13,-0.836276920587007,
-8.326));
#9984=CARTESIAN_POINT('Ctrl Pts',(-1.64313007644523E-13,-1.23722530465462,
-8.326));
#9985=CARTESIAN_POINT('Ctrl Pts',(0.45333287016887,-1.25372893469042,-8.32600000000001));
#9986=CARTESIAN_POINT('Ctrl Pts',(0.906883604181015,-1.27101861962826,-8.2889791048775));
#9987=CARTESIAN_POINT('Ctrl Pts',(2.45137675289882,-1.33260520473156,-8.03400595285804));
#9988=CARTESIAN_POINT('Ctrl Pts',(3.4994098080405,-1.37912460857061,-7.63599213029627));
#9989=CARTESIAN_POINT('Ctrl Pts',(5.3417347790895,-1.47059325393864,-6.47517577658188));
#9990=CARTESIAN_POINT('Ctrl Pts',(6.12721156907266,-1.51469212536274,-5.73756317941479));
#9991=CARTESIAN_POINT('Ctrl Pts',(7.38793936163156,-1.59731514352563,-3.99024063221344));
#9992=CARTESIAN_POINT('Ctrl Pts',(7.84519299083219,-1.6364171675431,-2.99279585597472));
#9993=CARTESIAN_POINT('Ctrl Pts',(8.35273678667891,-1.72567995947416,-0.869361554209782));
#9994=CARTESIAN_POINT('Ctrl Pts',(8.39451611548493,-1.77217678388878,0.236731474578972));
#9995=CARTESIAN_POINT('Ctrl Pts',(8.05356647674601,-1.86149975252815,2.36159729426944));
#9996=CARTESIAN_POINT('Ctrl Pts',(7.68954020709712,-1.90296397982766,3.36261837976914));
#9997=CARTESIAN_POINT('Ctrl Pts',(6.58294250017045,-1.98219883243943,5.21570282980361));
#9998=CARTESIAN_POINT('Ctrl Pts',(5.83497839553806,-2.02677082600436,6.04079910360755));
#9999=CARTESIAN_POINT('Ctrl Pts',(4.07693071225599,-2.11807821982965,7.33991611397237));
#10000=CARTESIAN_POINT('Ctrl Pts',(3.08837653689269,-2.16389552857394,7.80754669966619));
#10001=CARTESIAN_POINT('Ctrl Pts',(1.01371873022242,-2.25043234230026,8.33130831925508));
#10002=CARTESIAN_POINT('Ctrl Pts',(-0.0503438229743022,-2.2876583024077,
8.39259726328537));
#10003=CARTESIAN_POINT('Ctrl Pts',(-2.20140372280025,-2.37198004742297,
8.10655459135599));
#10004=CARTESIAN_POINT('Ctrl Pts',(-3.26463690440948,-2.41839613987866,
7.73978342056256));
#10005=CARTESIAN_POINT('Ctrl Pts',(-5.14681570295621,-2.51020813123452,
6.63166049983803));
#10006=CARTESIAN_POINT('Ctrl Pts',(-5.95614134912819,-2.55472405224028,
5.91551330576726));
#10007=CARTESIAN_POINT('Ctrl Pts',(-7.26359036630716,-2.63816729368409,
4.21009041318948));
#10008=CARTESIAN_POINT('Ctrl Pts',(-7.74711629613665,-2.67622471447422,
3.23525975383656));
#10009=CARTESIAN_POINT('Ctrl Pts',(-8.32134354280608,-2.76453738050967,
1.13442758980562));
#10010=CARTESIAN_POINT('Ctrl Pts',(-8.39826570590334,-2.81110609603825,
0.026624374117372));
#10011=CARTESIAN_POINT('Ctrl Pts',(-8.12245633024576,-2.90108553134084,
-2.11385784968141));
#10012=CARTESIAN_POINT('Ctrl Pts',(-7.7882058564614,-2.9437343272369,-3.12841177719816));
#10013=CARTESIAN_POINT('Ctrl Pts',(-6.73602202434712,-3.02309937664837,
-5.01639292405682));
#10014=CARTESIAN_POINT('Ctrl Pts',(-6.01308051593968,-3.06656282599005,
-5.86361355011189));
#10015=CARTESIAN_POINT('Ctrl Pts',(-4.29182791602042,-3.15766797377071,
-7.216839225372));
#10016=CARTESIAN_POINT('Ctrl Pts',(-3.31452643198635,-3.20371095642881,
-7.71469696420591));
#10017=CARTESIAN_POINT('Ctrl Pts',(-1.52959397443031,-3.2793189003798,-8.22031321013249));
#10018=CARTESIAN_POINT('Ctrl Pts',(-0.765970835835665,-3.30934005713638,
-8.32600000000001));
#10019=CARTESIAN_POINT('Ctrl Pts',(2.7602919949743E-13,-3.33722530465466,
-8.32600000000001));
#10020=CARTESIAN_POINT('Origin',(0.,-25.4,0.));
#10021=CARTESIAN_POINT('',(6.90525909241849E-14,-5.43722530465464,-8.326));
#10022=CARTESIAN_POINT('',(2.10354451091469E-14,-5.03627692058703,-8.326));
#10023=CARTESIAN_POINT('',(-1.01964092497009E-15,-25.4,-8.326));
#10024=CARTESIAN_POINT('Ctrl Pts',(-1.93317584162855E-13,-5.03627692058702,
-8.32600000000001));
#10025=CARTESIAN_POINT('Ctrl Pts',(-0.627541089026963,-5.01343122232191,
-8.326));
#10026=CARTESIAN_POINT('Ctrl Pts',(-1.25438846567005,-4.98911976048114,
-8.25506161187213));
#10027=CARTESIAN_POINT('Ctrl Pts',(-2.92207237103168,-4.9203349052019,-7.87098798089334));
#10028=CARTESIAN_POINT('Ctrl Pts',(-3.91824713956257,-4.87470570623752,
-7.42550637562141));
#10029=CARTESIAN_POINT('Ctrl Pts',(-5.70237834616604,-4.78328446629484,
-6.16615087989869));
#10030=CARTESIAN_POINT('Ctrl Pts',(-6.46817800278721,-4.73840654091963,
-5.35739132687811));
#10031=CARTESIAN_POINT('Ctrl Pts',(-7.61406835007107,-4.65827666942867,
-3.52978128523068));
#10032=CARTESIAN_POINT('Ctrl Pts',(-7.99942490620298,-4.61798142540627,
-2.5383477346419));
#10033=CARTESIAN_POINT('Ctrl Pts',(-8.38674744177094,-4.52916092693061,
-0.425434962331447));
#10034=CARTESIAN_POINT('Ctrl Pts',(-8.37005524029738,-4.48274354844585,
0.678768161280285));
#10035=CARTESIAN_POINT('Ctrl Pts',(-7.91068720079588,-4.39282183208492,
2.81787733391118));
#10036=CARTESIAN_POINT('Ctrl Pts',(-7.47238878950199,-4.35277187807424,
3.8317740885327));
#10037=CARTESIAN_POINT('Ctrl Pts',(-6.24504309267525,-4.27074256311847,
5.60866941930545));
#10038=CARTESIAN_POINT('Ctrl Pts',(-5.47677251068441,-4.22696068286926,
6.36100250850893));
#10039=CARTESIAN_POINT('Ctrl Pts',(-3.6634992643114,-4.13578340203622,7.55827563330548));
#10040=CARTESIAN_POINT('Ctrl Pts',(-2.62674553517158,-4.089217376626,7.97804394272964));
#10041=CARTESIAN_POINT('Ctrl Pts',(-0.493299661123184,-4.00311931726632,
8.37910696355535));
#10042=CARTESIAN_POINT('Ctrl Pts',(0.579550680952056,-3.96617845848151,
8.37358382216603));
#10043=CARTESIAN_POINT('Ctrl Pts',(2.67956787801854,-3.8809579531506,7.95637214776438));
#10044=CARTESIAN_POINT('Ctrl Pts',(3.68589481875409,-3.83563555477465,7.54307131598211));
#10045=CARTESIAN_POINT('Ctrl Pts',(5.50610740935759,-3.74412705080919,6.34205883767688));
#10046=CARTESIAN_POINT('Ctrl Pts',(6.29702077858317,-3.69884549288094,5.55759382721559));
#10047=CARTESIAN_POINT('Ctrl Pts',(7.49931750586196,-3.61744533361428,3.7672458386162));
#10048=CARTESIAN_POINT('Ctrl Pts',(7.91534818506142,-3.57852575872554,2.78918236097401));
#10049=CARTESIAN_POINT('Ctrl Pts',(8.36836596637517,-3.49044180108196,0.693790842857477));
#10050=CARTESIAN_POINT('Ctrl Pts',(8.38721689004991,-3.44417756367676,-0.406769286183216));
#10051=CARTESIAN_POINT('Ctrl Pts',(8.00606656997257,-3.35545392974148,-2.51737778980474));
#10052=CARTESIAN_POINT('Ctrl Pts',(7.6232516134654,-3.3150284961571,-3.50994129513667));
#10053=CARTESIAN_POINT('Ctrl Pts',(6.48204165644963,-3.23500481003877,-5.34060601389237));
#10054=CARTESIAN_POINT('Ctrl Pts',(5.71835232030774,-3.19016227447647,-6.15133700302137));
#10055=CARTESIAN_POINT('Ctrl Pts',(3.93728803867132,-3.09875232751809,-7.41546728068426));
#10056=CARTESIAN_POINT('Ctrl Pts',(2.9419976746152,-3.05309962121162,-7.86359913161293));
#10057=CARTESIAN_POINT('Ctrl Pts',(1.26823149266639,-2.98397125555753,-8.25348119269115));
#10058=CARTESIAN_POINT('Ctrl Pts',(0.634493343967036,-2.9593757164125,-8.32600000000003));
#10059=CARTESIAN_POINT('Ctrl Pts',(-1.35863542638504E-13,-2.93627692058703,
-8.32600000000001));
#10060=CARTESIAN_POINT('Ctrl Pts',(2.68188249386014E-13,-3.33722530465466,
-8.326));
#10061=CARTESIAN_POINT('Ctrl Pts',(0.284634040473044,-3.34758743634347,
-8.326));
#10062=CARTESIAN_POINT('Ctrl Pts',(0.5695698157431,-3.35826731999166,-8.31140488963583));
#10063=CARTESIAN_POINT('Ctrl Pts',(1.95122153822608,-3.41155987284974,-8.16898847079264));
#10064=CARTESIAN_POINT('Ctrl Pts',(3.01530817863659,-3.4572375489945,-7.8388272723186));
#10065=CARTESIAN_POINT('Ctrl Pts',(4.9271483037556,-3.54873600418471,-6.7969964311812));
#10066=CARTESIAN_POINT('Ctrl Pts',(5.76204111184506,-3.59366811490462,-6.10533174307115));
#10067=CARTESIAN_POINT('Ctrl Pts',(7.12030687096346,-3.67798896252267,-4.44617203508329));
#10068=CARTESIAN_POINT('Ctrl Pts',(7.63214563950504,-3.71529046447498,-3.49536994096109));
#10069=CARTESIAN_POINT('Ctrl Pts',(8.27791829973826,-3.80253606293005,-1.41992179028542));
#10070=CARTESIAN_POINT('Ctrl Pts',(8.3930281071515,-3.84913124309678,-0.31148901866247));
#10071=CARTESIAN_POINT('Ctrl Pts',(8.18833732112736,-3.93974926131201,1.84418418036667));
#10072=CARTESIAN_POINT('Ctrl Pts',(7.88663132312279,-3.98297698808641,2.87251004643474));
#10073=CARTESIAN_POINT('Ctrl Pts',(6.89238308755243,-4.06401504670441,4.80028969230388));
#10074=CARTESIAN_POINT('Ctrl Pts',(6.19377020061474,-4.10598316736002,5.6732273343516));
#10075=CARTESIAN_POINT('Ctrl Pts',(4.50926145560161,-4.1969500512168,7.08351703071612));
#10076=CARTESIAN_POINT('Ctrl Pts',(3.54449358779289,-4.24318556136984,7.61224353778558));
#10077=CARTESIAN_POINT('Ctrl Pts',(1.50056805248625,-4.3311499187908,8.25715346310258));
#10078=CARTESIAN_POINT('Ctrl Pts',(0.44488149708526,-4.36988227433181,8.38057447494808));
#10079=CARTESIAN_POINT('Ctrl Pts',(-1.70603330412962,-4.45148435351502,
8.22367441466779));
#10080=CARTESIAN_POINT('Ctrl Pts',(-2.7793896961637,-4.4968266124313,7.92552709037528));
#10081=CARTESIAN_POINT('Ctrl Pts',(-4.72420305139443,-4.58834064668239,
6.94006635187627));
#10082=CARTESIAN_POINT('Ctrl Pts',(-5.581564023546,-4.633609830387,6.27128069592846));
#10083=CARTESIAN_POINT('Ctrl Pts',(-6.98526054098617,-4.71870200902734,
4.6541116433428));
#10084=CARTESIAN_POINT('Ctrl Pts',(-7.52225758131639,-4.75566777851888,
3.72427989316282));
#10085=CARTESIAN_POINT('Ctrl Pts',(-8.23113434903166,-4.84193264488188,
1.6721619579118));
#10086=CARTESIAN_POINT('Ctrl Pts',(-8.38028167058735,-4.88850639197476,
0.564239048497007));
#10087=CARTESIAN_POINT('Ctrl Pts',(-8.23934139144515,-4.97961002486669,
-1.60298622995543));
#10088=CARTESIAN_POINT('Ctrl Pts',(-7.96698996357564,-5.02331543516025,
-2.64267550453953));
#10089=CARTESIAN_POINT('Ctrl Pts',(-7.03195186438206,-5.10520472094139,
-4.59070462858071));
#10090=CARTESIAN_POINT('Ctrl Pts',(-6.36743914444412,-5.14550073499438,
-5.47530658661011));
#10091=CARTESIAN_POINT('Ctrl Pts',(-4.73579600884035,-5.23557429482982,
-6.9346603998634));
#10092=CARTESIAN_POINT('Ctrl Pts',(-3.7853913736369,-5.28196966790777,-7.49587057678226));
#10093=CARTESIAN_POINT('Ctrl Pts',(-1.86790297413526,-5.36590075728786,
-8.16788467551488));
#10094=CARTESIAN_POINT('Ctrl Pts',(-0.936858401587628,-5.40311887762686,
-8.32600000000001));
#10095=CARTESIAN_POINT('Ctrl Pts',(2.76167977375508E-13,-5.43722530465465,
-8.32600000000001));
#10096=CARTESIAN_POINT('Origin',(0.,-25.4,0.));
#10097=CARTESIAN_POINT('',(1.3923078857642E-14,-7.53722530465463,-8.32600000000001));
#10098=CARTESIAN_POINT('',(1.79415698465829E-13,-7.13627692058703,-8.326));
#10099=CARTESIAN_POINT('',(-1.01964092497009E-15,-25.4,-8.326));
#10100=CARTESIAN_POINT('Ctrl Pts',(2.82274204010946E-13,-7.13627692058702,
-8.32600000000001));
#10101=CARTESIAN_POINT('Ctrl Pts',(-0.789165471781706,-7.10754726994771,
-8.32600000000001));
#10102=CARTESIAN_POINT('Ctrl Pts',(-1.57561086339154,-7.076558686669,-8.21381512205618));
#10103=CARTESIAN_POINT('Ctrl Pts',(-3.3793572552361,-6.9998128428404,-7.68664754117325));
#10104=CARTESIAN_POINT('Ctrl Pts',(-4.35323870101583,-6.95371174366766,
-7.18010110459946));
#10105=CARTESIAN_POINT('Ctrl Pts',(-6.06353261638026,-6.86268119196448,
-5.8114434991415));
#10106=CARTESIAN_POINT('Ctrl Pts',(-6.77919512355584,-6.81969313260729,
-4.95792394651815));
#10107=CARTESIAN_POINT('Ctrl Pts',(-7.81547082758754,-6.73990905249919,
-3.05997465800181));
#10108=CARTESIAN_POINT('Ctrl Pts',(-8.14103231066469,-6.69710048598408,
-2.04162001570176));
#10109=CARTESIAN_POINT('Ctrl Pts',(-8.39780737308328,-6.60693999020395,
0.103169378199973));
#10110=CARTESIAN_POINT('Ctrl Pts',(-8.31064190933164,-6.56035891466547,
1.2112666208665));
#10111=CARTESIAN_POINT('Ctrl Pts',(-7.71713685090388,-6.4723289820834,3.30537295994639));
#10112=CARTESIAN_POINT('Ctrl Pts',(-7.22599867976158,-6.43451331818395,
4.27370401224569));
#10113=CARTESIAN_POINT('Ctrl Pts',(-5.90492838340159,-6.35083333427368,
5.96679768736565));
#10114=CARTESIAN_POINT('Ctrl Pts',(-5.08870848526377,-6.30620192994361,
6.67649805336952));
#10115=CARTESIAN_POINT('Ctrl Pts',(-3.1951027538352,-6.21430444864484,7.76889631299521));
#10116=CARTESIAN_POINT('Ctrl Pts',(-2.12757422265706,-6.16792702929897,
8.12638776402861));
#10117=CARTESIAN_POINT('Ctrl Pts',(0.0262958920409874,-6.08391961518951,
8.39260803460962));
#10118=CARTESIAN_POINT('Ctrl Pts',(1.08896143852785,-6.04654298732901,8.32170952011937));
#10119=CARTESIAN_POINT('Ctrl Pts',(3.15903894726869,-5.95978221498718,7.77935928075863));
#10120=CARTESIAN_POINT('Ctrl Pts',(4.14418876263519,-5.91389061189867,7.30229745795536));
#10121=CARTESIAN_POINT('Ctrl Pts',(5.89081572379785,-5.82264522114307,5.98634910552458));
#10122=CARTESIAN_POINT('Ctrl Pts',(6.63104730371181,-5.77821055380764,5.15439329567684));
#10123=CARTESIAN_POINT('Ctrl Pts',(7.72078661688588,-5.69936214463135,3.2904951256647));
#10124=CARTESIAN_POINT('Ctrl Pts',(8.0756620491109,-5.65734359062175,2.28528884202502));
#10125=CARTESIAN_POINT('Ctrl Pts',(8.3965560385927,-5.56780792566576,0.155363280813972));
#10126=CARTESIAN_POINT('Ctrl Pts',(8.34393513110765,-5.52128403700471,-0.951373567734187));
#10127=CARTESIAN_POINT('Ctrl Pts',(7.81572462935436,-5.43231103653743,-3.06791414456359));
#10128=CARTESIAN_POINT('Ctrl Pts',(7.35033571627815,-5.39356666948127,-4.05832948874711));
#10129=CARTESIAN_POINT('Ctrl Pts',(6.07519282028708,-5.31068924186536,-5.79278841929773));
#10130=CARTESIAN_POINT('Ctrl Pts',(5.28232667201742,-5.26645830908955,-6.52388537427337));
#10131=CARTESIAN_POINT('Ctrl Pts',(3.42760068430076,-5.17487557640673,-7.66865048552837));
#10132=CARTESIAN_POINT('Ctrl Pts',(2.37480276131679,-5.12838325423159,-8.05712284670339));
#10133=CARTESIAN_POINT('Ctrl Pts',(0.853433947479236,-5.06803527645898,
-8.29321912371142));
#10134=CARTESIAN_POINT('Ctrl Pts',(0.426582072994635,-5.05180668508432,
-8.32600000000001));
#10135=CARTESIAN_POINT('Ctrl Pts',(-1.83880688453542E-13,-5.03627692058702,
-8.326));
#10136=CARTESIAN_POINT('Ctrl Pts',(3.22658566531686E-13,-5.43722530465465,
-8.326));
#10137=CARTESIAN_POINT('Ctrl Pts',(0.115242825540931,-5.44142073164033,
-8.326));
#10138=CARTESIAN_POINT('Ctrl Pts',(0.230570012134633,-5.44566951968454,
-8.32360735092844));
#10139=CARTESIAN_POINT('Ctrl Pts',(1.44802154484938,-5.49105499582223,-8.27298397950286));
#10140=CARTESIAN_POINT('Ctrl Pts',(2.53001450434268,-5.53600207189707,-8.00859729935472));
#10141=CARTESIAN_POINT('Ctrl Pts',(4.50752570799239,-5.62744383038148,-7.08320957009196));
#10142=CARTESIAN_POINT('Ctrl Pts',(5.38772903319495,-5.67302565544003,-6.43911344783354));
#10143=CARTESIAN_POINT('Ctrl Pts',(6.83852901515565,-5.75890426387314,-4.86611390641289));
#10144=CARTESIAN_POINT('Ctrl Pts',(7.40151074496943,-5.79586215273628,-3.95754172249426));
#10145=CARTESIAN_POINT('Ctrl Pts',(8.17496759702204,-5.88108712121583,-1.93016147232249));
#10146=CARTESIAN_POINT('Ctrl Pts',(8.35922730506451,-5.927594488038,-0.823817654718859));
#10147=CARTESIAN_POINT('Ctrl Pts',(8.28440438257484,-6.01911695318644,1.35337104478397));
#10148=CARTESIAN_POINT('Ctrl Pts',(8.04267463665364,-6.06327745927948,2.40388639830039));
#10149=CARTESIAN_POINT('Ctrl Pts',(7.16831860410432,-6.14601865095975,4.37218114667342));
#10150=CARTESIAN_POINT('Ctrl Pts',(6.53785084847891,-6.18495084955976,5.26853490975192));
#10151=CARTESIAN_POINT('Ctrl Pts',(4.96023544643382,-6.27407958464587,6.77651544047292));
#10152=CARTESIAN_POINT('Ctrl Pts',(4.02546522173726,-6.32058950742719,7.37025515833655));
#10153=CARTESIAN_POINT('Ctrl Pts',(2.01741401214559,-6.41001147690843,8.14665025570088));
#10154=CARTESIAN_POINT('Ctrl Pts',(0.96893740319249,-6.45172920697687,8.33655409840725));
#10155=CARTESIAN_POINT('Ctrl Pts',(-1.18962159763602,-6.53078477097846,
8.31405009682517));
#10156=CARTESIAN_POINT('Ctrl Pts',(-2.27913392655953,-6.5752934368299,8.08354565240009));
#10157=CARTESIAN_POINT('Ctrl Pts',(-4.28736690734935,-6.66657301189691,
7.21908582566198));
#10158=CARTESIAN_POINT('Ctrl Pts',(-5.1896363256036,-6.7124253012663,6.60034137853915));
#10159=CARTESIAN_POINT('Ctrl Pts',(-6.6869764967138,-6.79906641750539,5.07167386650422));
#10160=CARTESIAN_POINT('Ctrl Pts',(-7.27562957264802,-6.83635871872085,
4.18361484138809));
#10161=CARTESIAN_POINT('Ctrl Pts',(-8.11208318058106,-6.92053452190012,
2.18119273490226));
#10162=CARTESIAN_POINT('Ctrl Pts',(-8.33080510686291,-6.96693309058429,
1.07743706957574));
#10163=CARTESIAN_POINT('Ctrl Pts',(-8.32122271503474,-7.05878572940046,
-1.10760598980569));
#10164=CARTESIAN_POINT('Ctrl Pts',(-8.10988188534875,-7.10335578212811,
-2.16786387269312));
#10165=CARTESIAN_POINT('Ctrl Pts',(-7.29480546599385,-7.18690941030035,
-4.15548532458625));
#10166=CARTESIAN_POINT('Ctrl Pts',(-6.69673996384445,-7.22485069476321,
-5.06320242269887));
#10167=CARTESIAN_POINT('Ctrl Pts',(-5.17167919968289,-7.31303200118316,
-6.61713430741024));
#10168=CARTESIAN_POINT('Ctrl Pts',(-4.25301141865439,-7.35960695430917,
-7.24185823383286));
#10169=CARTESIAN_POINT('Ctrl Pts',(-2.26406967797738,-7.44967161048689,
-8.08192909903374));
#10170=CARTESIAN_POINT('Ctrl Pts',(-1.21879508517463,-7.49239522799274,
-8.30412804988923));
#10171=CARTESIAN_POINT('Ctrl Pts',(-0.106565493398858,-7.53333503073361,
-8.32548873079942));
#10172=CARTESIAN_POINT('Ctrl Pts',(-0.0532718526244207,-7.53528593734887,
-8.326));
#10173=CARTESIAN_POINT('Ctrl Pts',(-1.69645946028209E-13,-7.53722530465462,
-8.326));
#10174=CARTESIAN_POINT('Origin',(0.,-25.4,0.));
#10175=CARTESIAN_POINT('',(-2.09648082726249E-13,-9.63722530465461,-8.32599999999999));
#10176=CARTESIAN_POINT('',(-8.53327934765894E-14,-9.23627692058699,-8.326));
#10177=CARTESIAN_POINT('',(-1.01964092497009E-15,-25.4,-8.326));
#10178=CARTESIAN_POINT('Ctrl Pts',(-1.5931700403371E-13,-9.236276920587,
-8.32600000000001));
#10179=CARTESIAN_POINT('Ctrl Pts',(-0.962827742290914,-9.20122507702443,
-8.32599999999999));
#10180=CARTESIAN_POINT('Ctrl Pts',(-1.91916005087542,-9.16289949585406,
-8.15899449696305));
#10181=CARTESIAN_POINT('Ctrl Pts',(-3.85551855683091,-9.07771841623852,
-7.46019341735059));
#10182=CARTESIAN_POINT('Ctrl Pts',(-4.80149563487271,-9.03128485713617,
-6.88949770453631));
#10183=CARTESIAN_POINT('Ctrl Pts',(-6.41750042506982,-8.94148158700807,
-5.41591709451043));
#10184=CARTESIAN_POINT('Ctrl Pts',(-7.0720782020427,-8.90161624283425,-4.52790056294519));
#10185=CARTESIAN_POINT('Ctrl Pts',(-7.98957366844959,-8.81947856321835,
-2.5739625044236));
#10186=CARTESIAN_POINT('Ctrl Pts',(-8.25312633563117,-8.77563794010715,
-1.53105671006943));
#10187=CARTESIAN_POINT('Ctrl Pts',(-8.37502902429166,-8.6844049307812,0.63924624892485));
#10188=CARTESIAN_POINT('Ctrl Pts',(-8.21575204543581,-8.63784572502947,
1.74682324060707));
#10189=CARTESIAN_POINT('Ctrl Pts',(-7.4881957532555,-8.55187785526042,3.79187605116871));
#10190=CARTESIAN_POINT('Ctrl Pts',(-6.94371280324449,-8.51495006180625,
4.71553437529232));
#10191=CARTESIAN_POINT('Ctrl Pts',(-5.52645478157601,-8.42962999276952,
6.32005658747283));
#10192=CARTESIAN_POINT('Ctrl Pts',(-4.66246809746165,-8.38426688399616,
6.98183486007834));
#10193=CARTESIAN_POINT('Ctrl Pts',(-2.70808146161542,-8.29276432099371,
7.950168420921));
#10194=CARTESIAN_POINT('Ctrl Pts',(-1.63213515306542,-8.24753085845283,
8.23865365752571));
#10195=CARTESIAN_POINT('Ctrl Pts',(0.520048250783737,-8.16628844384065,
8.37624462091184));
#10196=CARTESIAN_POINT('Ctrl Pts',(1.57459773525679,-8.12721653133655,8.24335870237829));
#10197=CARTESIAN_POINT('Ctrl Pts',(3.61360696238517,-8.03903962169354,7.57982085407758));
#10198=CARTESIAN_POINT('Ctrl Pts',(4.57438581497659,-7.99275377962882,7.04179052142734));
#10199=CARTESIAN_POINT('Ctrl Pts',(6.24385941608477,-7.90203766145591,5.61738990668474));
#10200=CARTESIAN_POINT('Ctrl Pts',(6.93269095124139,-7.86057902586403,4.74111236724755));
#10201=CARTESIAN_POINT('Ctrl Pts',(7.91011108858901,-7.7792970103382,2.80752933505153));
#10202=CARTESIAN_POINT('Ctrl Pts',(8.20352963955394,-7.73593022547473,1.77589547569885));
#10203=CARTESIAN_POINT('Ctrl Pts',(8.39018480114286,-7.64516658335104,-0.383241908078162));
#10204=CARTESIAN_POINT('Ctrl Pts',(8.26542708644195,-7.59857317969374,-1.49163241907991));
#10205=CARTESIAN_POINT('Ctrl Pts',(7.60170970248472,-7.51160275538163,-3.56053457000042));
#10206=CARTESIAN_POINT('Ctrl Pts',(7.08273791404664,-7.47442901591286,-4.50535137706311));
#10207=CARTESIAN_POINT('Ctrl Pts',(5.71161189305219,-7.38988853142366,-6.15268615287862));
#10208=CARTESIAN_POINT('Ctrl Pts',(4.87031909218055,-7.34485756864492,-6.83796882684674));
#10209=CARTESIAN_POINT('Ctrl Pts',(2.94900870780505,-7.25334634450483,-7.86400420794327));
#10210=CARTESIAN_POINT('Ctrl Pts',(1.88220704353294,-7.20775908119327,-8.18516126286428));
#10211=CARTESIAN_POINT('Ctrl Pts',(0.522825152156074,-7.15556890449744,
-8.31370225250549));
#10212=CARTESIAN_POINT('Ctrl Pts',(0.261272938417734,-7.14578858893879,
-8.326));
#10213=CARTESIAN_POINT('Ctrl Pts',(2.80955814169204E-13,-7.13627692058702,
-8.326));
#10214=CARTESIAN_POINT('Ctrl Pts',(-1.90125692967058E-13,-7.53722530465462,
-8.326));
#10215=CARTESIAN_POINT('Ctrl Pts',(1.04852291534761,-7.57539688985758,-8.32600000000002));
#10216=CARTESIAN_POINT('Ctrl Pts',(2.08830637447319,-7.61741332770767,-8.12793571414206));
#10217=CARTESIAN_POINT('Ctrl Pts',(4.07495867046306,-7.70626649247324,-7.34153871441035));
#10218=CARTESIAN_POINT('Ctrl Pts',(4.99748301714605,-7.75233695005276,-6.7474970123295));
#10219=CARTESIAN_POINT('Ctrl Pts',(6.53860700822734,-7.83968146158204,-5.26119976282755));
#10220=CARTESIAN_POINT('Ctrl Pts',(7.15147389388194,-7.87759810417472,-4.39201734627695));
#10221=CARTESIAN_POINT('Ctrl Pts',(8.04067026318169,-7.96022838452596,-2.42636101998051));
#10222=CARTESIAN_POINT('Ctrl Pts',(8.29105868446047,-8.00586429958108,-1.3407477949843));
#10223=CARTESIAN_POINT('Ctrl Pts',(8.3533153449621,-8.09736952956764,0.836030904638805));
#10224=CARTESIAN_POINT('Ctrl Pts',(8.17583015512162,-8.14234811747502,1.90600725582994));
#10225=CARTESIAN_POINT('Ctrl Pts',(7.42586539952756,-8.22677161790711,3.91432172611022));
#10226=CARTESIAN_POINT('Ctrl Pts',(6.86245535308907,-8.26401027132523,4.8344735219243));
#10227=CARTESIAN_POINT('Ctrl Pts',(5.39478443440082,-8.3511276649061,6.43718960170184));
#10228=CARTESIAN_POINT('Ctrl Pts',(4.4946691345482,-8.39772243939458,7.0949904119213));
#10229=CARTESIAN_POINT('Ctrl Pts',(2.5282478613329,-8.4884092382017,8.00366763973184));
#10230=CARTESIAN_POINT('Ctrl Pts',(1.48742661994211,-8.53170225410734,8.2606703705065));
#10231=CARTESIAN_POINT('Ctrl Pts',(-0.677624860631812,-8.61285449078688,
8.37168276283262));
#10232=CARTESIAN_POINT('Ctrl Pts',(-1.78198178346068,-8.65458119998758,
8.20788193260203));
#10233=CARTESIAN_POINT('Ctrl Pts',(-3.84779404884213,-8.74543124868007,
7.46358798992179));
#10234=CARTESIAN_POINT('Ctrl Pts',(-4.79091179709949,-8.79169076047985,
6.89622044602366));
#10235=CARTESIAN_POINT('Ctrl Pts',(-6.37777986034509,-8.87975474067345,
5.45492399023233));
#10236=CARTESIAN_POINT('Ctrl Pts',(-7.01607527868148,-8.91864235756438,
4.60506176421419));
#10237=CARTESIAN_POINT('Ctrl Pts',(-7.96378240360662,-9.00007632614148,
2.66786398600753));
#10238=CARTESIAN_POINT('Ctrl Pts',(-8.24678415772775,-9.04536811559753,
1.59043701740506));
#10239=CARTESIAN_POINT('Ctrl Pts',(-8.37494108319709,-9.13687770840444,
-0.586445467481097));
#10240=CARTESIAN_POINT('Ctrl Pts',(-8.22882479580037,-9.18219128317005,
-1.66439067747666));
#10241=CARTESIAN_POINT('Ctrl Pts',(-7.53846529710902,-9.26739037080332,
-3.69115525929112));
#10242=CARTESIAN_POINT('Ctrl Pts',(-7.00596906938306,-9.3043347570921,-4.62271324724077));
#10243=CARTESIAN_POINT('Ctrl Pts',(-5.5904624310613,-9.39046073420771,-6.26861174815476));
#10244=CARTESIAN_POINT('Ctrl Pts',(-4.70805124321643,-9.43702813184697,
-6.95577446760812));
#10245=CARTESIAN_POINT('Ctrl Pts',(-2.76390130338,-9.52819326307102,-7.92578446611702));
#10246=CARTESIAN_POINT('Ctrl Pts',(-1.72807464976882,-9.57196243961983,
-8.21409243963136));
#10247=CARTESIAN_POINT('Ctrl Pts',(-0.444099013686395,-9.62087134292898,
-8.31712728198367));
#10248=CARTESIAN_POINT('Ctrl Pts',(-0.221925795915121,-9.62914607309612,
-8.32599999999999));
#10249=CARTESIAN_POINT('Ctrl Pts',(-5.92095816820404E-13,-9.6372253046546,
-8.326));
#10250=CARTESIAN_POINT('Origin',(0.,-25.4,0.));
#10251=CARTESIAN_POINT('',(-9.90421138979677E-14,-11.7372253046546,-8.326));
#10252=CARTESIAN_POINT('',(-4.00615157147562E-14,-11.336276920587,-8.32600000000001));
#10253=CARTESIAN_POINT('',(-1.01964092497009E-15,-25.4,-8.326));
#10254=CARTESIAN_POINT('Ctrl Pts',(-1.69645946028209E-13,-11.336276920587,
-8.326));
#10255=CARTESIAN_POINT('Ctrl Pts',(-0.0871960257465394,-11.3331025402493,
-8.326));
#10256=CARTESIAN_POINT('Ctrl Pts',(-0.174447220291238,-11.3298973610918,
-8.32463023531683));
#10257=CARTESIAN_POINT('Ctrl Pts',(-1.32159335929085,-11.2873770915746,
-8.28855269462512));
#10258=CARTESIAN_POINT('Ctrl Pts',(-2.3653020782673,-11.2444309137276,-8.05305278559879));
#10259=CARTESIAN_POINT('Ctrl Pts',(-4.34591435243672,-11.1541173109236,
-7.1867106920077));
#10260=CARTESIAN_POINT('Ctrl Pts',(-5.25763171742414,-11.1075285653815,
-6.54929208811676));
#10261=CARTESIAN_POINT('Ctrl Pts',(-6.76083033989904,-11.0197490755468,
-4.97661114831729));
#10262=CARTESIAN_POINT('Ctrl Pts',(-7.3456088754959,-10.9821222281375,-4.06416580190189));
#10263=CARTESIAN_POINT('Ctrl Pts',(-8.13593319278081,-10.8982351388597,
-2.06861178668239));
#10264=CARTESIAN_POINT('Ctrl Pts',(-8.33445896658462,-10.8535046155213,
-1.00453653720931));
#10265=CARTESIAN_POINT('Ctrl Pts',(-8.31673721429141,-10.7620500738183,
1.17103636056043));
#10266=CARTESIAN_POINT('Ctrl Pts',(-8.08856308821634,-10.7162053646745,
2.26161649865052));
#10267=CARTESIAN_POINT('Ctrl Pts',(-7.23918189662006,-10.6327795247358,
4.2461980510198));
#10268=CARTESIAN_POINT('Ctrl Pts',(-6.64331845503563,-10.5953324209896,
5.12858740153929));
#10269=CARTESIAN_POINT('Ctrl Pts',(-5.13292371355345,-10.5084801268576,
6.6446909752));
#10270=CARTESIAN_POINT('Ctrl Pts',(-4.22456190574248,-10.462559050157,7.25615579875248));
#10271=CARTESIAN_POINT('Ctrl Pts',(-2.20800795669339,-10.3713414629086,
8.10325408239908));
#10272=CARTESIAN_POINT('Ctrl Pts',(-1.11657276023476,-10.3269643782068,
8.32416776740145));
#10273=CARTESIAN_POINT('Ctrl Pts',(1.04284823483265,-10.2482754933851,8.3277332034444));
#10274=CARTESIAN_POINT('Ctrl Pts',(2.09043928045532,-10.2060195316864,8.12832978682023));
#10275=CARTESIAN_POINT('Ctrl Pts',(4.09310626916356,-10.1163968212246,7.33305826301642));
#10276=CARTESIAN_POINT('Ctrl Pts',(5.0232235754974,-10.0698630308749,6.73012390343341));
#10277=CARTESIAN_POINT('Ctrl Pts',(6.58535863862057,-9.98101056785104,5.20847487455484));
#10278=CARTESIAN_POINT('Ctrl Pts',(7.20621183314151,-9.94240469857657,4.3087710844042));
#10279=CARTESIAN_POINT('Ctrl Pts',(8.06313620508689,-9.8594225795479,2.33474501859507));
#10280=CARTESIAN_POINT('Ctrl Pts',(8.29597620131348,-9.81513799275605,1.28127796251173));
#10281=CARTESIAN_POINT('Ctrl Pts',(8.35167616643896,-9.72351025955491,-0.898414913581594));
#10282=CARTESIAN_POINT('Ctrl Pts',(8.1572962509068,-9.67703035837541,-2.00410536278288));
#10283=CARTESIAN_POINT('Ctrl Pts',(7.36530564639993,-9.5921105506584,-4.02422627435801));
#10284=CARTESIAN_POINT('Ctrl Pts',(6.79480785101672,-9.55508992471361,-4.92674058358165));
#10285=CARTESIAN_POINT('Ctrl Pts',(5.33037633488831,-9.46898644920149,-6.4868281483814));
#10286=CARTESIAN_POINT('Ctrl Pts',(4.44365565862945,-9.4233213765627,-7.12359656949709));
#10287=CARTESIAN_POINT('Ctrl Pts',(2.45697842123912,-9.33191767918727,-8.03129742379779));
#10288=CARTESIAN_POINT('Ctrl Pts',(1.37267689681404,-9.28709405993964,-8.2858118290869));
#10289=CARTESIAN_POINT('Ctrl Pts',(0.180130366492069,-9.24286528284347,
-8.32453949447813));
#10290=CARTESIAN_POINT('Ctrl Pts',(0.0900378828094111,-9.2395547590251,
-8.32600000000001));
#10291=CARTESIAN_POINT('Ctrl Pts',(-1.69645946028209E-13,-9.23627692058699,
-8.326));
#10292=CARTESIAN_POINT('Ctrl Pts',(-5.87307980026708E-13,-9.6372253046546,
-8.326));
#10293=CARTESIAN_POINT('Ctrl Pts',(0.869000389542001,-9.66886135373401,
-8.32600000000007));
#10294=CARTESIAN_POINT('Ctrl Pts',(1.73399941374016,-9.70321097215906,-8.18996555552375));
#10295=CARTESIAN_POINT('Ctrl Pts',(3.60396064025448,-9.78400592166834,-7.58484055309296));
#10296=CARTESIAN_POINT('Ctrl Pts',(4.56801084048846,-9.83041971757347,-7.04638868262423));
#10297=CARTESIAN_POINT('Ctrl Pts',(6.20286970073507,-9.91922029391959,-5.65316958515805));
#10298=CARTESIAN_POINT('Ctrl Pts',(6.8680568557066,-9.95947314318247,-4.82318427548233));
#10299=CARTESIAN_POINT('Ctrl Pts',(7.87622322720337,-10.0396380060417,-2.91617670929505));
#10300=CARTESIAN_POINT('Ctrl Pts',(8.1928178586592,-10.084527539032,-1.84831884736067));
#10301=CARTESIAN_POINT('Ctrl Pts',(8.38951602297935,-10.175952367871,0.326547223819863));
#10302=CARTESIAN_POINT('Ctrl Pts',(8.27632441033917,-10.221573749385,1.41181471663556));
#10303=CARTESIAN_POINT('Ctrl Pts',(7.64792358066077,-10.3075582523984,3.45726320832134));
#10304=CARTESIAN_POINT('Ctrl Pts',(7.14680640941996,-10.3445420065178,4.40073958274844));
#10305=CARTESIAN_POINT('Ctrl Pts',(5.78508544492922,-10.4296237060143,6.09011385799029));
#10306=CARTESIAN_POINT('Ctrl Pts',(4.92173077957157,-10.4761186151316,6.80683464583901));
#10307=CARTESIAN_POINT('Ctrl Pts',(3.0022771914387,-10.567691467586,7.83901819148436));
#10308=CARTESIAN_POINT('Ctrl Pts',(1.97251798521658,-10.6119107462533,8.15924986493847));
#10309=CARTESIAN_POINT('Ctrl Pts',(-0.16749159896407,-10.6947655384569,
8.39463882152912));
#10310=CARTESIAN_POINT('Ctrl Pts',(-1.25808996118376,-10.7335405198673,
8.30153012264513));
#10311=CARTESIAN_POINT('Ctrl Pts',(-3.35478832608991,-10.8225394833933,
7.69880181699771));
#10312=CARTESIAN_POINT('Ctrl Pts',(-4.33903155554408,-10.8690611361328,
7.1901937790795));
#10313=CARTESIAN_POINT('Ctrl Pts',(-6.02187123199346,-10.9585779435994,
5.84600366272615));
#10314=CARTESIAN_POINT('Ctrl Pts',(-6.71423630389552,-11.0005458801513,
5.03555110976292));
#10315=CARTESIAN_POINT('Ctrl Pts',(-7.78196847488304,-11.0794287420123,
3.15904051589254));
#10316=CARTESIAN_POINT('Ctrl Pts',(-8.13147695047584,-11.12387577742,2.10170903930992));
#10317=CARTESIAN_POINT('Ctrl Pts',(-8.39600473501651,-11.2151270044095,
-0.0690272918744915));
#10318=CARTESIAN_POINT('Ctrl Pts',(-8.31569897347412,-11.261012150754,-1.16056937320085));
#10319=CARTESIAN_POINT('Ctrl Pts',(-7.74871382918034,-11.3477530860962,
-3.22401230937071));
#10320=CARTESIAN_POINT('Ctrl Pts',(-7.27798106075176,-11.3851151234394,
-4.17943658060089));
#10321=CARTESIAN_POINT('Ctrl Pts',(-5.96909251183774,-11.4691505252429,
-5.91053942909384));
#10322=CARTESIAN_POINT('Ctrl Pts',(-5.12520597859944,-11.5155315283573,
-6.65556068873632));
#10323=CARTESIAN_POINT('Ctrl Pts',(-3.23165076425933,-11.6074217081022,
-7.74769905945298));
#10324=CARTESIAN_POINT('Ctrl Pts',(-2.20872951052089,-11.6520429968389,
-8.09890090453043));
#10325=CARTESIAN_POINT('Ctrl Pts',(-0.766347204124753,-11.7087709278027,
-8.29957434137255));
#10326=CARTESIAN_POINT('Ctrl Pts',(-0.383003348969663,-11.7232820281137,
-8.326));
#10327=CARTESIAN_POINT('Ctrl Pts',(-1.91097138113605E-13,-11.7372253046546,
-8.32600000000001));
#10328=CARTESIAN_POINT('Origin',(0.,-25.4,0.));
#10329=CARTESIAN_POINT('',(-3.00001195540908E-14,-13.8372253046546,-8.326));
#10330=CARTESIAN_POINT('',(-2.20333979338266E-13,-13.436276920587,-8.326));
#10331=CARTESIAN_POINT('',(-1.01964092497009E-15,-25.4,-8.326));
#10332=CARTESIAN_POINT('Ctrl Pts',(-6.35810848415019E-13,-13.436276920587,
-8.326));
#10333=CARTESIAN_POINT('Ctrl Pts',(-0.244293380369658,-13.4273833948025,
-8.32599999999998));
#10334=CARTESIAN_POINT('Ctrl Pts',(-0.488864284435648,-13.4182537891015,
-8.31524867723662));
#10335=CARTESIAN_POINT('Ctrl Pts',(-1.7952150574658,-13.3682692059687,-8.19979093626448));
#10336=CARTESIAN_POINT('Ctrl Pts',(-2.82947595083118,-13.3243729980939,
-7.90272719891034));
#10337=CARTESIAN_POINT('Ctrl Pts',(-4.76705283660299,-13.2330879564291,
-6.91562734063026));
#10338=CARTESIAN_POINT('Ctrl Pts',(-5.6443386572485,-13.1865359381765,-6.2203189320574));
#10339=CARTESIAN_POINT('Ctrl Pts',(-7.04515688427244,-13.1006929553017,
-4.56244341391435));
#10340=CARTESIAN_POINT('Ctrl Pts',(-7.56903468065117,-13.0637724887533,
-3.62765171586709));
#10341=CARTESIAN_POINT('Ctrl Pts',(-8.2425265460097,-12.9783573924836,-1.59574859717597));
#10342=CARTESIAN_POINT('Ctrl Pts',(-8.37970838905144,-12.9329559048327,
-0.515712065229338));
#10343=CARTESIAN_POINT('Ctrl Pts',(-8.23288905208651,-12.8414603721068,
1.66083595041613));
#10344=CARTESIAN_POINT('Ctrl Pts',(-7.94070750201063,-12.7962736361084,
2.73576384733817));
#10345=CARTESIAN_POINT('Ctrl Pts',(-6.97650406028944,-12.7151826690141,
4.66480211027158));
#10346=CARTESIAN_POINT('Ctrl Pts',(-6.33093644428556,-12.6759595128334,
5.5092335064573));
#10347=CARTESIAN_POINT('Ctrl Pts',(-4.73104640127706,-12.587693759401,6.93757502589118));
#10348=CARTESIAN_POINT('Ctrl Pts',(-3.78217867448249,-12.5413878669107,
7.49718997555689));
#10349=CARTESIAN_POINT('Ctrl Pts',(-1.71192558243361,-12.4507782382054,
8.2223536847459));
#10350=CARTESIAN_POINT('Ctrl Pts',(-0.609468416702,-12.40952625874,8.37650681930984));
#10351=CARTESIAN_POINT('Ctrl Pts',(1.55233521257709,-12.3281418750017,8.24882408974617));
#10352=CARTESIAN_POINT('Ctrl Pts',(2.5919037050054,-12.2847172399287,7.98338947018905));
#10353=CARTESIAN_POINT('Ctrl Pts',(4.55251481294434,-12.1938940018742,7.05815735135888));
#10354=CARTESIAN_POINT('Ctrl Pts',(5.44795676229049,-12.1473023705306,6.39241160247143));
#10355=CARTESIAN_POINT('Ctrl Pts',(6.90163061743603,-12.0604488147846,4.77800454784065));
#10356=CARTESIAN_POINT('Ctrl Pts',(7.45669437328654,-12.0233213068294,3.85480445672747));
#10357=CARTESIAN_POINT('Ctrl Pts',(8.19070822572816,-11.9386883178769,1.84150655381739));
#10358=CARTESIAN_POINT('Ctrl Pts',(8.35983152585037,-11.8936163918223,0.769309821443966));
#10359=CARTESIAN_POINT('Ctrl Pts',(8.27995043713631,-11.8021017440288,-1.40769291435304));
#10360=CARTESIAN_POINT('Ctrl Pts',(8.02080968950356,-11.7565537587041,-2.49121441667634));
#10361=CARTESIAN_POINT('Ctrl Pts',(7.11592151099839,-11.6742411722816,-4.44931325825822));
#10362=CARTESIAN_POINT('Ctrl Pts',(6.49628867115953,-11.6360973086953,-5.3133046025694));
#10363=CARTESIAN_POINT('Ctrl Pts',(4.94296495827753,-11.5485593337285,-6.78767575167891));
#10364=CARTESIAN_POINT('Ctrl Pts',(4.01488982970492,-11.5024345196705,-7.37468934344307));
#10365=CARTESIAN_POINT('Ctrl Pts',(2.04236887930033,-11.4146088993274,-8.13667492393123));
#10366=CARTESIAN_POINT('Ctrl Pts',(1.02513969015335,-11.3735972370578,-8.32600000000002));
#10367=CARTESIAN_POINT('Ctrl Pts',(-1.49047441055927E-13,-11.336276920587,
-8.326));
#10368=CARTESIAN_POINT('Ctrl Pts',(-1.70974345792274E-13,-11.7372253046546,
-8.326));
#10369=CARTESIAN_POINT('Ctrl Pts',(0.688416805123358,-11.7622871896619,
-8.32600000000001));
#10370=CARTESIAN_POINT('Ctrl Pts',(1.37560149155916,-11.7890985396939,-8.24063136044071));
#10371=CARTESIAN_POINT('Ctrl Pts',(3.11270832515499,-11.8615930580718,-7.80030659717876));
#10372=CARTESIAN_POINT('Ctrl Pts',(4.11545846611232,-11.908173194906,-7.32097096414827));
#10373=CARTESIAN_POINT('Ctrl Pts',(5.84334509313178,-11.9983179442442,-6.02492877478023));
#10374=CARTESIAN_POINT('Ctrl Pts',(6.56181117057933,-12.0411124930625,-5.23330616179504));
#10375=CARTESIAN_POINT('Ctrl Pts',(7.68588015961778,-12.1208597058931,-3.38610622472077));
#10376=CARTESIAN_POINT('Ctrl Pts',(8.06641453193172,-12.1638889131946,-2.33928227228454));
#10377=CARTESIAN_POINT('Ctrl Pts',(8.39489220525927,-12.2549263330369,-0.17363210769324));
#10378=CARTESIAN_POINT('Ctrl Pts',(8.34581543744271,-12.301022417095,0.922927880507992));
#10379=CARTESIAN_POINT('Ctrl Pts',(7.83683890332679,-12.388457021665,3.00287221665176));
#10380=CARTESIAN_POINT('Ctrl Pts',(7.39420399893262,-12.4264764337694,3.96973644201845));
#10381=CARTESIAN_POINT('Ctrl Pts',(6.14318644496827,-12.5089591261339,5.72720131525916));
#10382=CARTESIAN_POINT('Ctrl Pts',(5.33108418628558,-12.5545545097282,6.48989702116947));
#10383=CARTESIAN_POINT('Ctrl Pts',(3.48106058093707,-12.6460648708137,7.6393636637798));
#10384=CARTESIAN_POINT('Ctrl Pts',(2.46673345852369,-12.6910872200773,8.02453229494171));
#10385=CARTESIAN_POINT('Ctrl Pts',(0.354198819465129,-12.7756083676375,
8.38678967926924));
#10386=CARTESIAN_POINT('Ctrl Pts',(-0.723663939789811,-12.8127923416359,
8.36301614042901));
#10387=CARTESIAN_POINT('Ctrl Pts',(-2.84695595370087,-12.8997871229495,
7.90170264944797));
#10388=CARTESIAN_POINT('Ctrl Pts',(-3.86880978107385,-12.9463808201591,
7.45481040798338));
#10389=CARTESIAN_POINT('Ctrl Pts',(-5.64429487073648,-13.0371318739719,
6.21236493967363));
#10390=CARTESIAN_POINT('Ctrl Pts',(-6.39039052642516,-13.0804865120355,
5.44195071395798));
#10391=CARTESIAN_POINT('Ctrl Pts',(-7.57502979177055,-13.1617471005116,
3.62765948359466));
#10392=CARTESIAN_POINT('Ctrl Pts',(-7.98880913892081,-13.2032495293137,
2.59237801568459));
#10393=CARTESIAN_POINT('Ctrl Pts',(-8.38590534881367,-13.2939878427895,
0.433843164257152));
#10394=CARTESIAN_POINT('Ctrl Pts',(-8.37057874153018,-13.3402694076479,
-0.667129147202364));
#10395=CARTESIAN_POINT('Ctrl Pts',(-7.9240781663077,-13.4284276948276,-2.76428885879811));
#10396=CARTESIAN_POINT('Ctrl Pts',(-7.51111629860612,-13.4674686056598,
-3.74366776027912));
#10397=CARTESIAN_POINT('Ctrl Pts',(-6.31445379093895,-13.5487426811493,
-5.53777579763203));
#10398=CARTESIAN_POINT('Ctrl Pts',(-5.52602162297095,-13.5939858440471,
-6.3247116488873));
#10399=CARTESIAN_POINT('Ctrl Pts',(-3.70933867906954,-13.6854897128754,
-7.53161712802861));
#10400=CARTESIAN_POINT('Ctrl Pts',(-2.7039832981551,-13.7308447110542,-7.94815175625943));
#10401=CARTESIAN_POINT('Ctrl Pts',(-1.10368897537432,-13.7958920421356,
-8.27112684548052));
#10402=CARTESIAN_POINT('Ctrl Pts',(-0.551922163868698,-13.8171325211826,
-8.32599999999999));
#10403=CARTESIAN_POINT('Ctrl Pts',(-1.69447789133415E-13,-13.8372253046546,
-8.326));
#10404=CARTESIAN_POINT('Origin',(0.,-25.4,0.));
#10405=CARTESIAN_POINT('',(1.31710802876467E-13,-15.9372253046546,-8.326));
#10406=CARTESIAN_POINT('',(-5.24127468637111E-14,-15.536276920587,-8.32600000000001));
#10407=CARTESIAN_POINT('',(-1.01964092497009E-15,-25.4,-8.326));
#10408=CARTESIAN_POINT('Ctrl Pts',(-1.9824419883463E-13,-15.536276920587,
-8.326));
#10409=CARTESIAN_POINT('Ctrl Pts',(-0.415423225689894,-15.5211533950802,
-8.32599999999999));
#10410=CARTESIAN_POINT('Ctrl Pts',(-0.831152842721723,-15.5053652841283,
-8.29491160871503));
#10411=CARTESIAN_POINT('Ctrl Pts',(-2.30456298631406,-15.4470470746465,
-8.07231905411615));
#10412=CARTESIAN_POINT('Ctrl Pts',(-3.32443099059752,-15.4022721166688,
-7.70851768241614));
#10413=CARTESIAN_POINT('Ctrl Pts',(-5.19603470084908,-15.3108059798038,
-6.59853293999313));
#10414=CARTESIAN_POINT('Ctrl Pts',(-6.02375926394927,-15.2649962294663,
-5.85269690189743));
#10415=CARTESIAN_POINT('Ctrl Pts',(-7.31145534060758,-15.1817081186679,
-4.12044158562378));
#10416=CARTESIAN_POINT('Ctrl Pts',(-7.77422058168194,-15.1441900200468,
-3.16181276029789));
#10417=CARTESIAN_POINT('Ctrl Pts',(-8.32487343007585,-15.0572517101063,
-1.09367456439759));
#10418=CARTESIAN_POINT('Ctrl Pts',(-8.39640058252918,-15.0113034100589,
-0.000630146698329115));
#10419=CARTESIAN_POINT('Ctrl Pts',(-8.11382169386083,-14.9200971440347,
2.16903662735235));
#10420=CARTESIAN_POINT('Ctrl Pts',(-7.75547962811613,-14.8758650529199,
3.22339452550135));
#10421=CARTESIAN_POINT('Ctrl Pts',(-6.67192674647674,-14.7971488574488,
5.09171755891762));
#10422=CARTESIAN_POINT('Ctrl Pts',(-5.97213680740976,-14.7547493610765,
5.89689272580657));
#10423=CARTESIAN_POINT('Ctrl Pts',(-4.27672996110017,-14.6650590678691,
7.22756982132451));
#10424=CARTESIAN_POINT('Ctrl Pts',(-3.28721224745853,-14.6185165723781,
7.72803382321316));
#10425=CARTESIAN_POINT('Ctrl Pts',(-1.18669435827851,-14.5297789102049,
8.31171454696549));
#10426=CARTESIAN_POINT('Ctrl Pts',(-0.0978809398525554,-14.4912994342431,
8.39542208880966));
#10427=CARTESIAN_POINT('Ctrl Pts',(2.03857652379367,-14.4082182045706,8.14310743117581));
#10428=CARTESIAN_POINT('Ctrl Pts',(3.06652100905073,-14.3638832033155,7.81422681871336));
#10429=CARTESIAN_POINT('Ctrl Pts',(4.9789354556467,-14.2722139334238,6.76526385610018));
#10430=CARTESIAN_POINT('Ctrl Pts',(5.83695116708594,-14.2257464873203,6.04060234053506));
#10431=CARTESIAN_POINT('Ctrl Pts',(7.18398591264743,-14.1409536612427,4.33953455985475));
#10432=CARTESIAN_POINT('Ctrl Pts',(7.67661647837247,-14.1038984858139,3.39276329165898));
#10433=CARTESIAN_POINT('Ctrl Pts',(8.28800307877674,-14.017702196901,1.34227671597481));
#10434=CARTESIAN_POINT('Ctrl Pts',(8.39210620743553,-13.9720035985342,0.255172344540094));
#10435=CARTESIAN_POINT('Ctrl Pts',(8.17659970973539,-13.8806179549867,-1.91876156453496));
#10436=CARTESIAN_POINT('Ctrl Pts',(7.85084545688346,-13.8358466947024,-2.9838058877545));
#10437=CARTESIAN_POINT('Ctrl Pts',(6.82614140066146,-13.756034658513,-4.88242021150409));
#10438=CARTESIAN_POINT('Ctrl Pts',(6.15347965511124,-13.7153428614236,-5.70697927224458));
#10439=CARTESIAN_POINT('Ctrl Pts',(4.50536797928717,-13.6263423599158,-7.0867556877632));
#10440=CARTESIAN_POINT('Ctrl Pts',(3.53566489294802,-13.5798940837778,-7.61705694325303));
#10441=CARTESIAN_POINT('Ctrl Pts',(1.68355465962175,-13.500260965082,-8.19782418226262));
#10442=CARTESIAN_POINT('Ctrl Pts',(0.843529862891192,-13.4669857125087,
-8.32600000000006));
#10443=CARTESIAN_POINT('Ctrl Pts',(-6.21447338033931E-13,-13.436276920587,
-8.326));
#10444=CARTESIAN_POINT('Ctrl Pts',(-1.22263310586845E-13,-13.8372253046546,
-8.326));
#10445=CARTESIAN_POINT('Ctrl Pts',(0.506006521673632,-13.8556465244225,
-8.32600000000001));
#10446=CARTESIAN_POINT('Ctrl Pts',(1.01207216474324,-13.8750393390131,-8.2798766955888));
#10447=CARTESIAN_POINT('Ctrl Pts',(2.60142913319411,-13.9390688051404,-7.98638465930482));
#10448=CARTESIAN_POINT('Ctrl Pts',(3.63984296492492,-13.9856294345243,-7.56974845942933));
#10449=CARTESIAN_POINT('Ctrl Pts',(5.45736661377731,-14.0768513846503,-6.37771201034996));
#10450=CARTESIAN_POINT('Ctrl Pts',(6.22814566591867,-14.1206802871203,-5.62748653598145));
#10451=CARTESIAN_POINT('Ctrl Pts',(7.46034339023599,-14.202796288597,-3.85487086634778));
#10452=CARTESIAN_POINT('Ctrl Pts',(7.90140763876149,-14.2426981553964,-2.84338012778482));
#10453=CARTESIAN_POINT('Ctrl Pts',(8.36780531265433,-14.332525185874,-0.706523397054396));
#10454=CARTESIAN_POINT('Ctrl Pts',(8.38814146698981,-14.3789555675698,0.397989054372284));
#10455=CARTESIAN_POINT('Ctrl Pts',(8.00755289703476,-14.4678499428711,2.51265925082595));
#10456=CARTESIAN_POINT('Ctrl Pts',(7.62530940326286,-14.5083049882139,3.5054772831053));
#10457=CARTESIAN_POINT('Ctrl Pts',(6.48515189101122,-14.5883047810943,5.33682811766344));
#10458=CARTESIAN_POINT('Ctrl Pts',(5.72193762573087,-14.6331393193333,6.14800146386527));
#10459=CARTESIAN_POINT('Ctrl Pts',(3.94156448946698,-14.724546642076,7.41320398774386));
#10460=CARTESIAN_POINT('Ctrl Pts',(2.9464738700826,-14.770204593253,7.86193134254663));
#10461=CARTESIAN_POINT('Ctrl Pts',(0.86280018710557,-14.8562885270598,8.34853027366915));
#10462=CARTESIAN_POINT('Ctrl Pts',(-0.20417723742401,-14.893302526408,8.39050850143965));
#10463=CARTESIAN_POINT('Ctrl Pts',(-2.34939178007754,-14.978248993173,8.06461889796505));
#10464=CARTESIAN_POINT('Ctrl Pts',(-3.40374961079458,-15.0247314331787,
7.67931854162733));
#10465=CARTESIAN_POINT('Ctrl Pts',(-5.26255306531183,-15.1163502780165,
6.53989769688107));
#10466=CARTESIAN_POINT('Ctrl Pts',(-6.05785492677433,-15.1606241903758,
5.81097467512499));
#10467=CARTESIAN_POINT('Ctrl Pts',(-7.33776083397924,-15.2435854173261,
4.08077858908891));
#10468=CARTESIAN_POINT('Ctrl Pts',(-7.805831728621,-15.282218517097,3.09267575201798));
#10469=CARTESIAN_POINT('Ctrl Pts',(-8.34085273165634,-15.3710950941658,
0.978428950091469));
#10470=CARTESIAN_POINT('Ctrl Pts',(-8.39705642800904,-15.4176269663975,
-0.128497816196545));
#10471=CARTESIAN_POINT('Ctrl Pts',(-8.08279322671259,-15.5072323289714,
-2.26008138417037));
#10472=CARTESIAN_POINT('Ctrl Pts',(-7.73093398441479,-15.5494404810598,
-3.26667650095998));
#10473=CARTESIAN_POINT('Ctrl Pts',(-6.64675040664428,-15.6281612235212,
-5.13412346942883));
#10474=CARTESIAN_POINT('Ctrl Pts',(-5.90907723633758,-15.6725498490239,
-5.96832003585186));
#10475=CARTESIAN_POINT('Ctrl Pts',(-4.16624352443,-15.7637730910409,-7.28978471501692));
#10476=CARTESIAN_POINT('Ctrl Pts',(-3.18223310098026,-15.8096883371853,
-7.76994489155944));
#10477=CARTESIAN_POINT('Ctrl Pts',(-1.43620030413394,-15.8829833267367,
-8.23289356433938));
#10478=CARTESIAN_POINT('Ctrl Pts',(-0.718940118465088,-15.9110522152675,
-8.326));
#10479=CARTESIAN_POINT('Ctrl Pts',(2.76445533131664E-13,-15.9372253046546,
-8.32600000000001));
#10480=CARTESIAN_POINT('Origin',(0.,-25.4,0.));
#10481=CARTESIAN_POINT('',(1.72372721153364E-13,-18.0372253046546,-8.326));
#10482=CARTESIAN_POINT('',(-1.03630498060333E-14,-17.636276920587,-8.326));
#10483=CARTESIAN_POINT('',(-1.01964092497009E-15,-25.4,-8.326));
#10484=CARTESIAN_POINT('Ctrl Pts',(-2.12052597703405E-13,-17.636276920587,
-8.326));
#10485=CARTESIAN_POINT('Ctrl Pts',(-0.575058079507399,-17.6153418717128,
-8.32599999999999));
#10486=CARTESIAN_POINT('Ctrl Pts',(-1.14982045747753,-17.5931655233299,
-8.26643034587313));
#10487=CARTESIAN_POINT('Ctrl Pts',(-2.77096762089726,-17.5269746993386,
-7.92516931059649));
#10488=CARTESIAN_POINT('Ctrl Pts',(-3.77359980056906,-17.4815322151829,
-7.49975562662993));
#10489=CARTESIAN_POINT('Ctrl Pts',(-5.58048141429174,-17.3900458012541,
-6.27670419988311));
#10490=CARTESIAN_POINT('Ctrl Pts',(-6.3620523412699,-17.3449105381877,-5.48301789632078));
#10491=CARTESIAN_POINT('Ctrl Pts',(-7.54320702466148,-17.2639844312338,
-3.67860486814112));
#10492=CARTESIAN_POINT('Ctrl Pts',(-7.94772870978091,-17.2245911121536,
-2.69558273995902));
#10493=CARTESIAN_POINT('Ctrl Pts',(-8.37624041010279,-17.1362290890949,
-0.593576442852489));
#10494=CARTESIAN_POINT('Ctrl Pts',(-8.38183638881273,-17.0899021394706,
0.508475507353455));
#10495=CARTESIAN_POINT('Ctrl Pts',(-7.96571678629875,-16.9994090296343,
2.66117731448738));
#10496=CARTESIAN_POINT('Ctrl Pts',(-7.54444213160671,-16.9583766883461,
3.68991327890768));
#10497=CARTESIAN_POINT('Ctrl Pts',(-6.34680823611166,-16.8768811055922,
5.49287750595405));
#10498=CARTESIAN_POINT('Ctrl Pts',(-5.5939483096094,-16.833393974563,6.2578793076948));
#10499=CARTESIAN_POINT('Ctrl Pts',(-3.80689607512934,-16.7425070311971,
7.48675513016755));
#10500=CARTESIAN_POINT('Ctrl Pts',(-2.78045510064503,-16.6959180237583,
7.9254790738769));
#10501=CARTESIAN_POINT('Ctrl Pts',(-0.654016405705544,-16.6091923630911,
8.36853836200114));
#10502=CARTESIAN_POINT('Ctrl Pts',(0.422300111506851,-16.5721100296044,
8.38342505306291));
#10503=CARTESIAN_POINT('Ctrl Pts',(2.53109525486195,-16.4873763282887,8.0045779717921));
#10504=CARTESIAN_POINT('Ctrl Pts',(3.54309116781857,-16.4422602642142,7.6109128844606));
#10505=CARTESIAN_POINT('Ctrl Pts',(5.38427974268193,-16.350743224854,6.44582578693569));
#10506=CARTESIAN_POINT('Ctrl Pts',(6.19005720279719,-16.3052388201027,5.67650372197135));
#10507=CARTESIAN_POINT('Ctrl Pts',(7.42641387110462,-16.2230803922604,3.90907302938784));
#10508=CARTESIAN_POINT('Ctrl Pts',(7.8610288922322,-16.1848182227143,2.93887109003904));
#10509=CARTESIAN_POINT('Ctrl Pts',(8.35324018828346,-16.0971869998293,0.854249485064087));
#10510=CARTESIAN_POINT('Ctrl Pts',(8.39326929677321,-16.0510368938999,-0.243595606274021));
#10511=CARTESIAN_POINT('Ctrl Pts',(8.04488101332369,-15.9596881118743,-2.41665263240238));
#10512=CARTESIAN_POINT('Ctrl Pts',(7.65032609785298,-15.9168802102447,-3.46873641199449));
#10513=CARTESIAN_POINT('Ctrl Pts',(6.49875765868641,-15.8362219575584,-5.31165057763646));
#10514=CARTESIAN_POINT('Ctrl Pts',(5.76993233127877,-15.7932139260652,-6.09548733907829));
#10515=CARTESIAN_POINT('Ctrl Pts',(4.02413471964635,-15.7028324013838,-7.37177188741203));
#10516=CARTESIAN_POINT('Ctrl Pts',(3.01415431952855,-15.6562411476875,-7.83911325276364));
#10517=CARTESIAN_POINT('Ctrl Pts',(1.3048478767382,-15.5853938080833,-8.24922164553926));
#10518=CARTESIAN_POINT('Ctrl Pts',(0.652861729446362,-15.560044419386,-8.32600000000001));
#10519=CARTESIAN_POINT('Ctrl Pts',(-1.69170233377258E-13,-15.536276920587,
-8.326));
#10520=CARTESIAN_POINT('Ctrl Pts',(2.71588307398929E-13,-15.9372253046546,
-8.326));
#10521=CARTESIAN_POINT('Ctrl Pts',(0.332370296269366,-15.949325279674,-8.326));
#10522=CARTESIAN_POINT('Ctrl Pts',(0.665068926132207,-15.9618554937788,
-8.30609914404716));
#10523=CARTESIAN_POINT('Ctrl Pts',(2.09179478361076,-16.0174100114443,-8.13413559434496));
#10524=CARTESIAN_POINT('Ctrl Pts',(3.15009218418154,-16.063262048947,-7.78565152309358));
#10525=CARTESIAN_POINT('Ctrl Pts',(5.04218002261011,-16.1547139850303,-6.71182196403841));
#10526=CARTESIAN_POINT('Ctrl Pts',(5.86385151991641,-16.1994350303207,-6.00729918400101));
#10527=CARTESIAN_POINT('Ctrl Pts',(7.19573372747264,-16.2833021503588,-4.32402888611314));
#10528=CARTESIAN_POINT('Ctrl Pts',(7.69290123095891,-16.320946271798,-3.36082636447661));
#10529=CARTESIAN_POINT('Ctrl Pts',(8.30165570219128,-16.4087500355188,-1.27210025950698));
#10530=CARTESIAN_POINT('Ctrl Pts',(8.39694883678225,-16.4553381700915,-0.163835092499947));
#10531=CARTESIAN_POINT('Ctrl Pts',(8.15529886321142,-16.5456372268563,1.984250469281));
#10532=CARTESIAN_POINT('Ctrl Pts',(7.83665298720733,-16.5885702247514,3.00556515635138));
#10533=CARTESIAN_POINT('Ctrl Pts',(6.8077136801888,-16.6691002127173,4.92125852722286));
#10534=CARTESIAN_POINT('Ctrl Pts',(6.08870950300239,-16.7122042267477,5.78723709941025));
#10535=CARTESIAN_POINT('Ctrl Pts',(4.37319166116847,-16.8036796223934,7.16801100261096));
#10536=CARTESIAN_POINT('Ctrl Pts',(3.40044148216312,-16.849798978357,7.67738545666204));
#10537=CARTESIAN_POINT('Ctrl Pts',(1.34649982119402,-16.9373171129223,8.2837169348852));
#10538=CARTESIAN_POINT('Ctrl Pts',(0.288331930262472,-16.97543654558,8.3874699219568));
#10539=CARTESIAN_POINT('Ctrl Pts',(-1.85974418193972,-17.0577818452421,
8.1902928011815));
#10540=CARTESIAN_POINT('Ctrl Pts',(-2.92741157807384,-17.1033390022504,
7.8720676097236));
#10541=CARTESIAN_POINT('Ctrl Pts',(-4.85177226945907,-17.1948529603484,
6.85118544144144));
#10542=CARTESIAN_POINT('Ctrl Pts',(-5.6951352910351,-17.2399154235644,6.16798979411118));
#10543=CARTESIAN_POINT('Ctrl Pts',(-7.0704344504019,-17.3245269623444,4.52450254583816));
#10544=CARTESIAN_POINT('Ctrl Pts',(-7.59171871260332,-17.3616647877063,
3.5816196117483));
#10545=CARTESIAN_POINT('Ctrl Pts',(-8.26124523219371,-17.4485454946569,
1.51485170868987));
#10546=CARTESIAN_POINT('Ctrl Pts',(-8.38913173063085,-17.4951375912553,
0.406492290752532));
#10547=CARTESIAN_POINT('Ctrl Pts',(-8.20833131569507,-17.5859471021696,
-1.75373624602508));
#10548=CARTESIAN_POINT('Ctrl Pts',(-7.91760598460155,-17.6293583608581,
-2.78642807414316));
#10549=CARTESIAN_POINT('Ctrl Pts',(-6.94563509800759,-17.7107190270286,
-4.72188209281742));
#10550=CARTESIAN_POINT('Ctrl Pts',(-6.25995560544519,-17.7520185073925,
-5.59923662458799));
#10551=CARTESIAN_POINT('Ctrl Pts',(-4.59534922424053,-17.842652874823,-7.02817804474219));
#10552=CARTESIAN_POINT('Ctrl Pts',(-3.63587814624271,-17.8889541784923,
-7.56920912840256));
#10553=CARTESIAN_POINT('Ctrl Pts',(-1.75941205318623,-17.9702285311227,
-8.18587600226779));
#10554=CARTESIAN_POINT('Ctrl Pts',(-0.881962201508673,-18.0051173794697,
-8.32600000000001));
#10555=CARTESIAN_POINT('Ctrl Pts',(2.67563748934663E-13,-18.0372253046546,
-8.32600000000001));
#10556=CARTESIAN_POINT('Origin',(0.,-25.4,0.));
#10557=CARTESIAN_POINT('',(3.96816528613292E-9,-20.1372253049435,-8.326));
#10558=CARTESIAN_POINT('',(1.34659832785628E-13,-19.736276920587,-8.326));
#10559=CARTESIAN_POINT('',(-1.01964092497009E-15,-25.4,-8.326));
#10560=CARTESIAN_POINT('Ctrl Pts',(3.03784775113058E-13,-19.736276920587,
-8.326));
#10561=CARTESIAN_POINT('Ctrl Pts',(-0.741011693602677,-19.7093003132238,
-8.326));
#10562=CARTESIAN_POINT('Ctrl Pts',(-1.48004434879021,-19.68031679053,-8.22708890753572));
#10563=CARTESIAN_POINT('Ctrl Pts',(-3.2444565536996,-19.6059354644762,-7.74428951636322));
#10564=CARTESIAN_POINT('Ctrl Pts',(-4.22535623213429,-19.5599586218775,
-7.25581078810072));
#10565=CARTESIAN_POINT('Ctrl Pts',(-5.95826066548303,-19.4687804626706,
-5.91929300528484));
#10566=CARTESIAN_POINT('Ctrl Pts',(-6.6889796239238,-19.4247794053195,-5.07891910823867));
#10567=CARTESIAN_POINT('Ctrl Pts',(-7.75818481398095,-19.3458715811982,
-3.20181469785529));
#10568=CARTESIAN_POINT('Ctrl Pts',(-8.10174283459321,-19.3033982210791,
-2.19143413684825));
#10569=CARTESIAN_POINT('Ctrl Pts',(-8.39797991796542,-19.2136214509322,
-0.0557730275832109));
#10570=CARTESIAN_POINT('Ctrl Pts',(-8.3320695963325,-19.1670703405566,1.05161138666675));
#10571=CARTESIAN_POINT('Ctrl Pts',(-7.77864352391814,-19.078456621778,3.15960516538214));
#10572=CARTESIAN_POINT('Ctrl Pts',(-7.30332110660647,-19.040107635104,4.14146876881184));
#10573=CARTESIAN_POINT('Ctrl Pts',(-6.01051168074491,-18.9569200440293,
5.86008506322163));
#10574=CARTESIAN_POINT('Ctrl Pts',(-5.2086265645188,-18.9125313569302,6.58306620743989));
#10575=CARTESIAN_POINT('Ctrl Pts',(-3.3388282817735,-18.8208186777339,7.70790782175316));
#10576=CARTESIAN_POINT('Ctrl Pts',(-2.28028135621384,-18.7743653587606,
8.08456695747027));
#10577=CARTESIAN_POINT('Ctrl Pts',(-0.132301086442923,-18.6897097506465,
8.39182795746986));
#10578=CARTESIAN_POINT('Ctrl Pts',(0.933296066553777,-18.652611722947,8.34082228835986));
#10579=CARTESIAN_POINT('Ctrl Pts',(3.01278616610347,-18.5663156313633,7.83688331731904));
#10580=CARTESIAN_POINT('Ctrl Pts',(4.0048717208109,-18.5205815362637,7.37932832753217));
#10581=CARTESIAN_POINT('Ctrl Pts',(5.77491249608914,-18.4292168573335,6.09825850022494));
#10582=CARTESIAN_POINT('Ctrl Pts',(6.53104614376202,-18.3845028252529,5.28055450329049));
#10583=CARTESIAN_POINT('Ctrl Pts',(7.65556865793812,-18.3048586762036,3.43904357504579));
#10584=CARTESIAN_POINT('Ctrl Pts',(8.02932411892815,-18.2639491185334,2.4424249145819));
#10585=CARTESIAN_POINT('Ctrl Pts',(8.39149230014016,-18.1748542313203,0.322984826192618));
#10586=CARTESIAN_POINT('Ctrl Pts',(8.36118956244984,-18.1283908287504,-0.78231314465672));
#10587=CARTESIAN_POINT('Ctrl Pts',(7.87562154473628,-18.038824561216,-2.91296669748745));
#10588=CARTESIAN_POINT('Ctrl Pts',(7.42701502102502,-17.9993096945417,-3.91790521670791));
#10589=CARTESIAN_POINT('Ctrl Pts',(6.18155268726809,-17.9169573879563,-5.67878863076229));
#10590=CARTESIAN_POINT('Ctrl Pts',(5.40392870253753,-17.8730015678831,-6.4231967110492));
#10591=CARTESIAN_POINT('Ctrl Pts',(3.5748326958408,-17.7816615041576,-7.60080875598084));
#10592=CARTESIAN_POINT('Ctrl Pts',(2.5319159568273,-17.7351180128823,-8.00883030942075));
#10593=CARTESIAN_POINT('Ctrl Pts',(0.963266230846582,-17.6722227700236,
-8.28422523926223));
#10594=CARTESIAN_POINT('Ctrl Pts',(0.481561790093202,-17.6538082273729,
-8.32600000000001));
#10595=CARTESIAN_POINT('Ctrl Pts',(-1.88044024795886E-13,-17.636276920587,
-8.326));
#10596=CARTESIAN_POINT('Ctrl Pts',(2.95805047123565E-13,-18.0372253046546,
-8.326));
#10597=CARTESIAN_POINT('Ctrl Pts',(0.168981087311088,-18.0433770786193,
-8.326));
#10598=CARTESIAN_POINT('Ctrl Pts',(0.338120011567569,-18.0496427233294,
-8.3208557368868));
#10599=CARTESIAN_POINT('Ctrl Pts',(1.60830093220243,-18.0975131031637,-8.24333772622879));
#10600=CARTESIAN_POINT('Ctrl Pts',(2.68506258215882,-18.1427107214706,-7.9579700686103));
#10601=CARTESIAN_POINT('Ctrl Pts',(4.642501116715,-18.2342079995147,-6.99517399461026));
#10602=CARTESIAN_POINT('Ctrl Pts',(5.5086104621158,-18.2796006496375,-6.33566678619455));
#10603=CARTESIAN_POINT('Ctrl Pts',(6.93023001768936,-18.3649937606886,-4.73522384198799));
#10604=CARTESIAN_POINT('Ctrl Pts',(7.47711943818315,-18.4019154738673,-3.813541860389));
#10605=CARTESIAN_POINT('Ctrl Pts',(8.21066834594864,-18.4877874049101,-1.77077129506958));
#10606=CARTESIAN_POINT('Ctrl Pts',(8.37319984712582,-18.534341145119,-0.663324320842134));
#10607=CARTESIAN_POINT('Ctrl Pts',(8.25742001501766,-18.6256142494957,1.50793244212956));
#10608=CARTESIAN_POINT('Ctrl Pts',(7.9967003642083,-18.6694976394034,2.55185559747756));
#10609=CARTESIAN_POINT('Ctrl Pts',(7.08483442339588,-18.7517146642827,4.50768116646479));
#10610=CARTESIAN_POINT('Ctrl Pts',(6.43342871760873,-18.7914480807177,5.39679016863165));
#10611=CARTESIAN_POINT('Ctrl Pts',(4.82243930383149,-18.8811641058222,6.87490679647979));
#10612=CARTESIAN_POINT('Ctrl Pts',(3.87789919103356,-18.9276090400981,7.44863260436268));
#10613=CARTESIAN_POINT('Ctrl Pts',(1.85840928867414,-19.0165892949646,8.18419978535578));
#10614=CARTESIAN_POINT('Ctrl Pts',(0.807893080887373,-19.0572352662045,
8.35352848045677));
#10615=CARTESIAN_POINT('Ctrl Pts',(-1.3486079894212,-19.1370832046557,8.28976112626951));
#10616=CARTESIAN_POINT('Ctrl Pts',(-2.43362679443577,-19.1818666240449,
8.03840168180975));
#10617=CARTESIAN_POINT('Ctrl Pts',(-4.42319592982404,-19.2732565577242,
7.13636457911092));
#10618=CARTESIAN_POINT('Ctrl Pts',(-5.31198409205434,-19.3189474613863,
6.50194818245679));
#10619=CARTESIAN_POINT('Ctrl Pts',(-6.78075924333669,-19.4051223267751,
4.94598748806984));
#10620=CARTESIAN_POINT('Ctrl Pts',(-7.3536522617107,-19.442169075152,4.04539476239995));
#10621=CARTESIAN_POINT('Ctrl Pts',(-8.15153415864958,-19.5269912651094,
2.02759603787036));
#10622=CARTESIAN_POINT('Ctrl Pts',(-8.3491344671574,-19.5734616444342,0.922132099992329));
#10623=CARTESIAN_POINT('Ctrl Pts',(-8.29952591628968,-19.6651214263525,
-1.25832316929844));
#10624=CARTESIAN_POINT('Ctrl Pts',(-8.06952074714483,-19.7094448324464,
-2.31271368112304));
#10625=CARTESIAN_POINT('Ctrl Pts',(-7.21813885438952,-19.7925032020478,
-4.28855363912642));
#10626=CARTESIAN_POINT('Ctrl Pts',(-6.60032745014865,-19.8310114214651,
-5.18932082489098));
#10627=CARTESIAN_POINT('Ctrl Pts',(-5.04311010714147,-19.9197756220679,
-6.71528832105067));
#10628=CARTESIAN_POINT('Ctrl Pts',(-4.11448679814829,-19.9663161675756,
-7.32113175104967));
#10629=CARTESIAN_POINT('Ctrl Pts',(-2.11386189931371,-20.0559877100324,
-8.12226356506916));
#10630=CARTESIAN_POINT('Ctrl Pts',(-1.06658045254075,-20.0983712645419,
-8.32480731712692));
#10631=CARTESIAN_POINT('Ctrl Pts',(-0.00623416757088782,-20.1369983123485,
-8.32599824958923));
#10632=CARTESIAN_POINT('Ctrl Pts',(-0.00311703891250096,-20.1371118285306,
-8.32600000000297));
#10633=CARTESIAN_POINT('Ctrl Pts',(7.93618616483201E-9,-20.1372253049435,
-8.326));
#10634=CARTESIAN_POINT('Origin',(0.,-25.4,0.));
#10635=CARTESIAN_POINT('',(-1.37067252491379E-13,-22.2372253046546,-8.32600000000001));
#10636=CARTESIAN_POINT('',(1.39802199830121E-13,-21.836276920587,-8.326));
#10637=CARTESIAN_POINT('',(-1.01964092497009E-15,-25.4,-8.326));
#10638=CARTESIAN_POINT('Ctrl Pts',(3.3056890558214E-13,-21.836276920587,
-8.32600000000001));
#10639=CARTESIAN_POINT('Ctrl Pts',(-0.908108585131477,-21.8032171336015,
-8.326));
#10640=CARTESIAN_POINT('Ctrl Pts',(-1.81110815181515,-21.7672208890341,
-8.17744265861093));
#10641=CARTESIAN_POINT('Ctrl Pts',(-3.70730244560357,-21.6846788454566,
-7.53463291746772));
#10642=CARTESIAN_POINT('Ctrl Pts',(-4.66250514039434,-21.6383304747457,
-6.98396946186045));
#10643=CARTESIAN_POINT('Ctrl Pts',(-6.31142773900649,-21.5479614016373,
-5.54048487926333));
#10644=CARTESIAN_POINT('Ctrl Pts',(-6.98699738054398,-21.5071555424562,
-4.65967258766987));
#10645=CARTESIAN_POINT('Ctrl Pts',(-7.94140241989562,-21.4255424931981,
-2.7182147358875));
#10646=CARTESIAN_POINT('Ctrl Pts',(-8.22341469315457,-21.3819897412754,
-1.68215698586221));
#10647=CARTESIAN_POINT('Ctrl Pts',(-8.3852952316952,-21.2910366853893,0.481486280730521));
#10648=CARTESIAN_POINT('Ctrl Pts',(-8.24730836793455,-21.2444512489582,
1.58968726280175));
#10649=CARTESIAN_POINT('Ctrl Pts',(-7.55906152604825,-21.1578617658357,
3.64952736702381));
#10650=CARTESIAN_POINT('Ctrl Pts',(-7.03031309405226,-21.1208213621961,
4.58619078151074));
#10651=CARTESIAN_POINT('Ctrl Pts',(-5.64153242231531,-21.0359810148221,
6.21721342455858));
#10652=CARTESIAN_POINT('Ctrl Pts',(-4.79150414422494,-20.990818741746,6.89361317693311));
#10653=CARTESIAN_POINT('Ctrl Pts',(-2.85736689459058,-20.8993007037906,
7.89775595756132));
#10654=CARTESIAN_POINT('Ctrl Pts',(-1.78695446083802,-20.8538433842544,
8.20647662272373));
#10655=CARTESIAN_POINT('Ctrl Pts',(0.362500134543461,-20.7718492172337,
8.38456025275674));
#10656=CARTESIAN_POINT('Ctrl Pts',(1.4194733277575,-20.7334552437087,8.27149545687334));
#10657=CARTESIAN_POINT('Ctrl Pts',(3.46870639771315,-20.6457251120916,7.64692224576267));
#10658=CARTESIAN_POINT('Ctrl Pts',(4.43772923043642,-20.5995488348411,7.12838368637743));
#10659=CARTESIAN_POINT('Ctrl Pts',(6.13860673557218,-20.508312040779,5.73360395780598));
#10660=CARTESIAN_POINT('Ctrl Pts',(6.84794643020952,-20.4657585990833,4.86432701474728));
#10661=CARTESIAN_POINT('Ctrl Pts',(7.86050887218106,-20.3849878927729,2.94290729834406));
#10662=CARTESIAN_POINT('Ctrl Pts',(8.17118244694402,-20.3419144199962,1.91825091451713));
#10663=CARTESIAN_POINT('Ctrl Pts',(8.39542277107465,-20.2514616608006,-0.233491008519554));
#10664=CARTESIAN_POINT('Ctrl Pts',(8.2907872614984,-20.2048684103033,-1.34187787606265));
#10665=CARTESIAN_POINT('Ctrl Pts',(7.66455310005366,-20.1173266040453,-3.42437238721642));
#10666=CARTESIAN_POINT('Ctrl Pts',(7.16046463414603,-20.0798574060706,-4.38171071135767));
#10667=CARTESIAN_POINT('Ctrl Pts',(5.8161487017165,-19.9957759382129,-6.05364322287303));
#10668=CARTESIAN_POINT('Ctrl Pts',(4.98823156595436,-19.9509540545005,-6.75214584378655));
#10669=CARTESIAN_POINT('Ctrl Pts',(3.0867817751318,-19.8594768129244,-7.81096398868598));
#10670=CARTESIAN_POINT('Ctrl Pts',(2.02571973403472,-19.8137050882996,-8.15083850481592));
#10671=CARTESIAN_POINT('Ctrl Pts',(0.620131098081054,-19.7592165139285,
-8.30869825973521));
#10672=CARTESIAN_POINT('Ctrl Pts',(0.309905806485666,-19.7475590735318,
-8.326));
#10673=CARTESIAN_POINT('Ctrl Pts',(3.26197402422679E-13,-19.736276920587,
-8.326));
#10674=CARTESIAN_POINT('Ctrl Pts',(7.93620114070137E-9,-20.1372253049435,
-8.32599999999999));
#10675=CARTESIAN_POINT('Ctrl Pts',(1.09929152081772,-20.1772451262137,-8.32599999895217));
#10676=CARTESIAN_POINT('Ctrl Pts',(2.18807547233758,-20.2214584908025,-8.10828355822521));
#10677=CARTESIAN_POINT('Ctrl Pts',(4.20468880037571,-20.3125406121911,-7.2677332005755));
#10678=CARTESIAN_POINT('Ctrl Pts',(5.11496013298754,-20.3584826994036,-6.65857615086658));
#10679=CARTESIAN_POINT('Ctrl Pts',(6.62946625597013,-20.4454012489607,-5.1464414550283));
#10680=CARTESIAN_POINT('Ctrl Pts',(7.22760191635294,-20.4829026282789,-4.26583029573217));
#10681=CARTESIAN_POINT('Ctrl Pts',(8.08233451684404,-20.566222427601,-2.28377129814597));
#10682=CARTESIAN_POINT('Ctrl Pts',(8.31349443187262,-20.6120402658695,-1.19383037979337));
#10683=CARTESIAN_POINT('Ctrl Pts',(8.33718568320761,-20.7035038407883,0.981957405275777));
#10684=CARTESIAN_POINT('Ctrl Pts',(8.14147282185833,-20.7482686311639,2.04684781861082));
#10685=CARTESIAN_POINT('Ctrl Pts',(7.35656369922082,-20.8322282201805,4.04412649904621));
#10686=CARTESIAN_POINT('Ctrl Pts',(6.77467342822941,-20.8697940363974,4.95760578517001));
#10687=CARTESIAN_POINT('Ctrl Pts',(5.27625057320422,-20.9574851722186,6.53435496530883));
#10688=CARTESIAN_POINT('Ctrl Pts',(4.36607083693896,-21.0040759043001,7.17453133414064));
#10689=CARTESIAN_POINT('Ctrl Pts',(2.38731926118937,-21.0944419268729,8.04659023476296));
#10690=CARTESIAN_POINT('Ctrl Pts',(1.34397410464132,-21.1374357954337,8.28498884029207));
#10691=CARTESIAN_POINT('Ctrl Pts',(-0.828146017691834,-21.2180697833976,
8.3591011927717));
#10692=CARTESIAN_POINT('Ctrl Pts',(-1.93675392260759,-21.260933224618,8.173743957929));
#10693=CARTESIAN_POINT('Ctrl Pts',(-3.99238573558019,-21.3523060506757,
7.38694470104383));
#10694=CARTESIAN_POINT('Ctrl Pts',(-4.92252070723055,-21.3984504126804,
6.80256882669288));
#10695=CARTESIAN_POINT('Ctrl Pts',(-6.48039524342482,-21.486060263998,5.33266026336641));
#10696=CARTESIAN_POINT('Ctrl Pts',(-7.10255463824954,-21.5242948102021,
4.47059799089661));
#10697=CARTESIAN_POINT('Ctrl Pts',(-8.01327983054783,-21.606488629631,2.51532444642886));
#10698=CARTESIAN_POINT('Ctrl Pts',(-8.27567542750925,-21.6520030919063,
1.43260040955898));
#10699=CARTESIAN_POINT('Ctrl Pts',(-8.36212210043179,-21.7435197071686,
-0.744449129507846));
#10700=CARTESIAN_POINT('Ctrl Pts',(-8.1961189482673,-21.7886257042918,-1.81745636394051));
#10701=CARTESIAN_POINT('Ctrl Pts',(-7.46804495038655,-21.8733363379352,
-3.83260132312565));
#10702=CARTESIAN_POINT('Ctrl Pts',(-6.916075171964,-21.910428541569,-4.75693730423157));
#10703=CARTESIAN_POINT('Ctrl Pts',(-5.46760684795329,-21.997183556465,-6.37567231116854));
#10704=CARTESIAN_POINT('Ctrl Pts',(-4.57391746847598,-22.043773228963,-7.04436040383322));
#10705=CARTESIAN_POINT('Ctrl Pts',(-2.61549840024866,-22.1346456897299,
-7.97573112283634));
#10706=CARTESIAN_POINT('Ctrl Pts',(-1.57641225491258,-22.1781185513746,
-8.24429567455344));
#10707=CARTESIAN_POINT('Ctrl Pts',(-0.343231816087832,-22.2246185042882,
-8.32069940223016));
#10708=CARTESIAN_POINT('Ctrl Pts',(-0.17152966831258,-22.2309807493349,
-8.326));
#10709=CARTESIAN_POINT('Ctrl Pts',(-1.23893950654264E-13,-22.2372253046546,
-8.326));
#10710=CARTESIAN_POINT('Origin',(0.,-25.4,0.));
#10711=CARTESIAN_POINT('',(-1.64753439167969E-13,-24.3372253046546,-8.326));
#10712=CARTESIAN_POINT('',(-1.89759924326649E-15,-23.936276920587,-8.326));
#10713=CARTESIAN_POINT('',(-1.01964092497009E-15,-25.4,-8.326));
#10714=CARTESIAN_POINT('',(8.27736571547526,-24.9,0.898606038414384));
#10715=CARTESIAN_POINT('Ctrl Pts',(-1.50296441958631E-13,-24.3372253046546,
-8.326));
#10716=CARTESIAN_POINT('Ctrl Pts',(0.742893768952232,-24.3642704291657,
-8.32600000000001));
#10717=CARTESIAN_POINT('Ctrl Pts',(1.48389594827494,-24.3933362330634,-8.22658551882158));
#10718=CARTESIAN_POINT('Ctrl Pts',(3.262585844936,-24.4683481831947,-7.73851252336228));
#10719=CARTESIAN_POINT('Ctrl Pts',(4.25400469153752,-24.51489739812,-7.24102168886792));
#10720=CARTESIAN_POINT('Ctrl Pts',(5.95405524569837,-24.6046545861794,-5.91520506535258));
#10721=CARTESIAN_POINT('Ctrl Pts',(6.65650698446997,-24.6471111704798,-5.11192419028058));
#10722=CARTESIAN_POINT('Ctrl Pts',(7.62856775351797,-24.7174862679998,-3.44733676201697));
#10723=CARTESIAN_POINT('Ctrl Pts',(7.94693649975717,-24.7515948625903,-2.63174017322248));
#10724=CARTESIAN_POINT('Ctrl Pts',(8.32586411060715,-24.8243159404673,-0.901809617782638));
#10725=CARTESIAN_POINT('Ctrl Pts',(8.37455760848785,-24.8623656438899,0.00333846992109366));
#10726=CARTESIAN_POINT('Ctrl Pts',(8.27736571547527,-24.9,0.898606038414273));
#10727=CARTESIAN_POINT('',(2.19919404320626,-24.9,8.03030644249185));
#10728=CARTESIAN_POINT('Origin',(0.,-24.9,0.));
#10729=CARTESIAN_POINT('Ctrl Pts',(2.19919404320625,-24.9,8.03030644249185));
#10730=CARTESIAN_POINT('Ctrl Pts',(2.94095280141566,-24.8687265114472,7.82716706615144));
#10731=CARTESIAN_POINT('Ctrl Pts',(3.65097101877844,-24.8364691142525,7.52223989839009));
#10732=CARTESIAN_POINT('Ctrl Pts',(4.96518040040976,-24.7719179658425,6.7273581096632));
#10733=CARTESIAN_POINT('Ctrl Pts',(5.56341734142977,-24.7399313157154,6.24170146387279));
#10734=CARTESIAN_POINT('Ctrl Pts',(6.81761446664068,-24.666028411966,4.89794559820416));
#10735=CARTESIAN_POINT('Ctrl Pts',(7.39050128363734,-24.6286357804595,3.98122819228775));
#10736=CARTESIAN_POINT('Ctrl Pts',(8.1584498305441,-24.5444501764425,1.97857293787148));
#10737=CARTESIAN_POINT('Ctrl Pts',(8.34533182165618,-24.4995800271944,0.911176187470449));
#10738=CARTESIAN_POINT('Ctrl Pts',(8.30293131992899,-24.4080926332995,-1.26517821701211));
#10739=CARTESIAN_POINT('Ctrl Pts',(8.06242989867319,-24.3623612521532,-2.3530624439374));
#10740=CARTESIAN_POINT('Ctrl Pts',(7.19095506233322,-24.2793749941559,-4.32718696989518));
#10741=CARTESIAN_POINT('Ctrl Pts',(6.58568461817839,-24.2416861622831,-5.2022412392326));
#10742=CARTESIAN_POINT('Ctrl Pts',(5.0582780140935,-24.1545605163226,-6.70188470152501));
#10743=CARTESIAN_POINT('Ctrl Pts',(4.1420442351946,-24.1085545504541,-7.30375365526574));
#10744=CARTESIAN_POINT('Ctrl Pts',(2.13977222107689,-24.0185490972115,-8.11791910308778));
#10745=CARTESIAN_POINT('Ctrl Pts',(1.07469957386274,-23.9754014697511,-8.32600000000002));
#10746=CARTESIAN_POINT('Ctrl Pts',(-1.75692793646931E-13,-23.936276920587,
-8.326));
#10747=CARTESIAN_POINT('Origin',(0.,-24.4,0.));
#10748=CARTESIAN_POINT('',(2.33295215237571E-15,-24.4,19.05));
#10749=CARTESIAN_POINT('',(-2.33295215237571E-15,-24.4,-19.05));
#10750=CARTESIAN_POINT('Origin',(0.,-24.4,0.));
#10751=CARTESIAN_POINT('Origin',(0.,-24.4,0.));
#10752=CARTESIAN_POINT('',(-2.21048747246097E-15,-25.4,-18.05));
#10753=CARTESIAN_POINT('Origin',(-2.21048747246097E-15,-24.4,-18.05));
#10754=CARTESIAN_POINT('Origin',(0.,-25.4,0.));
#10755=CARTESIAN_POINT('Origin',(0.,14.4,0.));
#10756=CARTESIAN_POINT('',(-2.21048747246097E-15,15.4,-18.05));
#10757=CARTESIAN_POINT('Origin',(0.,15.4,0.));
#10758=CARTESIAN_POINT('',(-2.33295215237571E-15,14.4,-19.05));
#10759=CARTESIAN_POINT('Origin',(-2.21048747246097E-15,14.4,-18.05));
#10760=CARTESIAN_POINT('',(2.33295215237571E-15,14.4,19.05));
#10761=CARTESIAN_POINT('Origin',(0.,14.4,0.));
#10762=CARTESIAN_POINT('Origin',(0.,14.4,0.));
#10763=CARTESIAN_POINT('Origin',(17.3316043908594,-21.9,45.4192193816532));
#10764=CARTESIAN_POINT('',(19.3316043908594,-22.9,48.883320996791));
#10765=CARTESIAN_POINT('',(13.8675027757216,-22.9,47.4192193816532));
#10766=CARTESIAN_POINT('Origin',(17.3316043908594,-22.9,45.4192193816532));
#10767=CARTESIAN_POINT('',(19.8316043908594,-21.9,49.7493464005754));
#10768=CARTESIAN_POINT('Origin',(19.3316043908594,-21.9,48.883320996791));
#10769=CARTESIAN_POINT('',(13.0014773719372,-21.9,47.9192193816532));
#10770=CARTESIAN_POINT('Origin',(17.3316043908594,-21.9,45.4192193816532));
#10771=CARTESIAN_POINT('Origin',(13.8675027757216,-21.9,47.4192193816532));
#10772=CARTESIAN_POINT('Origin',(17.3316043908594,-7.90000000000001,45.4192193816532));
#10773=CARTESIAN_POINT('',(13.0014773719372,-7.9,47.9192193816532));
#10774=CARTESIAN_POINT('',(19.1957890247756,-4.56844441699029,48.6480818822852));
#10775=CARTESIAN_POINT('Origin',(17.3316043908594,-7.90000000000001,45.4192193816532));
#10776=CARTESIAN_POINT('',(11.9501151712092,11.6489333498058,36.0982066328347));
#10777=CARTESIAN_POINT('',(19.1957890247756,-4.56844441699029,48.6480818822853));
#10778=CARTESIAN_POINT('',(10.1102324883161,11.3230083161312,36.8657033664312));
#10779=CARTESIAN_POINT('Origin',(10.384104613565,7.6499999999371,33.3857967817714));
#10780=CARTESIAN_POINT('',(6.05397759465256,7.65,35.8857967818225));
#10781=CARTESIAN_POINT('Ctrl Pts',(6.05397759465256,7.65,35.8857967818225));
#10782=CARTESIAN_POINT('Ctrl Pts',(6.08928976743534,7.74017246065655,35.9469592592079));
#10783=CARTESIAN_POINT('Ctrl Pts',(6.12832838012931,7.83131579263958,36.006848308931));
#10784=CARTESIAN_POINT('Ctrl Pts',(6.17111895326201,7.92309626160611,36.0651473231755));
#10785=CARTESIAN_POINT('Ctrl Pts',(6.21435423570126,8.01583057684584,36.1240522211999));
#10786=CARTESIAN_POINT('Ctrl Pts',(6.26141987741726,8.10921506410549,36.1813336075092));
#10787=CARTESIAN_POINT('Ctrl Pts',(6.3122944546444,8.2028829922255,36.2366721483555));
#10788=CARTESIAN_POINT('Ctrl Pts',(6.36402406580603,8.29812516943968,36.2929407476491));
#10789=CARTESIAN_POINT('Ctrl Pts',(6.41969173269722,8.39366006533703,36.3472003412477));
#10790=CARTESIAN_POINT('Ctrl Pts',(6.47922558198133,8.48908360809998,36.3991269669764));
#10791=CARTESIAN_POINT('Ctrl Pts',(6.53926650009729,8.5853199036908,36.4514958683812));
#10792=CARTESIAN_POINT('Ctrl Pts',(6.60323963772497,8.68144252076869,36.5014915701947));
#10793=CARTESIAN_POINT('Ctrl Pts',(6.67102226579008,8.77702401761752,36.5487983543273));
#10794=CARTESIAN_POINT('Ctrl Pts',(6.73940230767439,8.87344793838393,36.5965220849163));
#10795=CARTESIAN_POINT('Ctrl Pts',(6.81165913893223,8.96932067908334,36.6415089425318));
#10796=CARTESIAN_POINT('Ctrl Pts',(6.88761899106763,9.06419708738261,36.6834566789221));
#10797=CARTESIAN_POINT('Ctrl Pts',(6.91875332268202,9.1030849139822,36.7006501659884));
#10798=CARTESIAN_POINT('Ctrl Pts',(6.95050922415029,9.14180532432651,36.7173333620187));
#10799=CARTESIAN_POINT('Ctrl Pts',(6.98287254062646,9.18032765868938,36.7334867131329));
#10800=CARTESIAN_POINT('Ctrl Pts',(7.06065466533108,9.27291239170125,36.7723097420302));
#10801=CARTESIAN_POINT('Ctrl Pts',(7.14193522550449,9.36433490372364,36.8080617552191));
#10802=CARTESIAN_POINT('Ctrl Pts',(7.22639353034653,9.45421392953755,36.8405831329111));
#10803=CARTESIAN_POINT('Ctrl Pts',(7.31498815818374,9.54849475671312,36.8746972364177));
#10804=CARTESIAN_POINT('Ctrl Pts',(7.40707923745252,9.64107659815097,36.9052560617205));
#10805=CARTESIAN_POINT('Ctrl Pts',(7.5022523237989,9.73153397866236,36.9321141600708));
#10806=CARTESIAN_POINT('Ctrl Pts',(7.59398106932454,9.81871768107638,36.9580002562715));
#10807=CARTESIAN_POINT('Ctrl Pts',(7.68857206543916,9.90392756518674,36.9804487410977));
#10808=CARTESIAN_POINT('Ctrl Pts',(7.78562171747329,9.98680273224879,36.9993663118177));
#10809=CARTESIAN_POINT('Ctrl Pts',(7.88226230101848,10.0693285768903,37.0182041441574));
#10810=CARTESIAN_POINT('Ctrl Pts',(7.98134035104027,10.1495389355592,37.0335406880032));
#10811=CARTESIAN_POINT('Ctrl Pts',(8.08243321548938,10.2271033948173,37.0453212245668));
#10812=CARTESIAN_POINT('Ctrl Pts',(8.18238435349759,10.3037918536328,37.0569687136581));
#10813=CARTESIAN_POINT('Ctrl Pts',(8.28430455192637,10.37789350802,37.0651400528604));
#10814=CARTESIAN_POINT('Ctrl Pts',(8.3877691935037,10.4491198811129,37.0698195899984));
#10815=CARTESIAN_POINT('Ctrl Pts',(8.40167504206957,10.4586928438471,37.0704485288688));
#10816=CARTESIAN_POINT('Ctrl Pts',(8.41560877166897,10.4682139182184,37.071014447974));
#10817=CARTESIAN_POINT('Ctrl Pts',(8.429569336418,10.4776824519197,37.0715173614424));
#10818=CARTESIAN_POINT('Ctrl Pts',(8.53515074276735,10.549291381947,37.0753208115335));
#10819=CARTESIAN_POINT('Ctrl Pts',(8.64225116327287,10.6178811928978,37.0755170775839));
#10820=CARTESIAN_POINT('Ctrl Pts',(8.75036064416503,10.683271528406,37.072237567608));
#10821=CARTESIAN_POINT('Ctrl Pts',(8.86231822477556,10.7509893982765,37.0688413252113));
#10822=CARTESIAN_POINT('Ctrl Pts',(8.97535731700236,10.815275468209,37.0617173928374));
#10823=CARTESIAN_POINT('Ctrl Pts',(9.08891450935123,10.8759743328058,37.0510506189197));
#10824=CARTESIAN_POINT('Ctrl Pts',(9.19619874745181,10.933320162754,37.0409730827542));
#10825=CARTESIAN_POINT('Ctrl Pts',(9.30394500151563,10.9874643718571,37.0277337487462));
#10826=CARTESIAN_POINT('Ctrl Pts',(9.41168854166736,11.0383162475296,37.0115189784436));
#10827=CARTESIAN_POINT('Ctrl Pts',(9.51841693092522,11.0886890009553,36.9954569823913));
#10828=CARTESIAN_POINT('Ctrl Pts',(9.62514225220611,11.1358311057241,36.9764755314245));
#10829=CARTESIAN_POINT('Ctrl Pts',(9.73142938425917,11.1796944882328,36.9547824460045));
#10830=CARTESIAN_POINT('Ctrl Pts',(9.83642685367666,11.2230256429507,36.9333525792938));
#10831=CARTESIAN_POINT('Ctrl Pts',(9.94099637984397,11.2631571549113,36.9092766665018));
#10832=CARTESIAN_POINT('Ctrl Pts',(10.0447401308685,11.3000824629291,36.8827785309424));
#10833=CARTESIAN_POINT('Ctrl Pts',(10.0666087164109,11.3078661053085,36.877192876496));
#10834=CARTESIAN_POINT('Ctrl Pts',(10.0884406962602,11.3155074248239,36.8714996709178));
#10835=CARTESIAN_POINT('Ctrl Pts',(10.1102324887055,11.3230065889554,36.8657011341632));
#10836=CARTESIAN_POINT('',(5.75580351837084,8.31737776679611,35.3693441322026));
#10837=CARTESIAN_POINT('Origin',(17.3316043908594,-22.9,45.4192193816532));
#10838=CARTESIAN_POINT('',(19.8316043908594,-7.90000000000001,49.7493464005754));
#10839=CARTESIAN_POINT('',(19.8316043908594,-22.9,49.7493464005754));
#10840=CARTESIAN_POINT('Origin',(17.3316043908594,-7.90000000000001,45.4192193816532));
#10841=CARTESIAN_POINT('',(13.0014773719372,-7.90000000000001,47.9192193816532));
#10842=CARTESIAN_POINT('Origin',(17.33160439086,-7.90000000000001,-45.419219381653));
#10843=CARTESIAN_POINT('',(13.0014773719379,-7.90000000000001,-47.919219381653));
#10844=CARTESIAN_POINT('',(19.8316043908601,-7.90000000000001,-49.7493464005752));
#10845=CARTESIAN_POINT('Origin',(17.33160439086,-7.90000000000001,-45.419219381653));
#10846=CARTESIAN_POINT('',(19.8316043908601,-21.9,-49.7493464005752));
#10847=CARTESIAN_POINT('',(19.8316043908601,-22.9,-49.7493464005752));
#10848=CARTESIAN_POINT('',(13.0014773719379,-21.9,-47.919219381653));
#10849=CARTESIAN_POINT('Origin',(17.33160439086,-21.9,-45.419219381653));
#10850=CARTESIAN_POINT('',(13.0014773719379,-7.90000000000001,-47.919219381653));
#10851=CARTESIAN_POINT('Origin',(17.33160439086,-7.90000000000001,-45.419219381653));
#10852=CARTESIAN_POINT('',(6.05397759465306,7.65,-35.8857967818224));
#10853=CARTESIAN_POINT('',(10.1102324887059,11.3230065889554,-36.865701134163));
#10854=CARTESIAN_POINT('Ctrl Pts',(6.05397759465306,7.65,-35.8857967818224));
#10855=CARTESIAN_POINT('Ctrl Pts',(6.08928976743518,7.74017246065474,-35.9469592592067));
#10856=CARTESIAN_POINT('Ctrl Pts',(6.12832838012837,7.83131579263597,-36.0068483089287));
#10857=CARTESIAN_POINT('Ctrl Pts',(6.17111895326016,7.92309626160072,-36.0651473231721));
#10858=CARTESIAN_POINT('Ctrl Pts',(6.21435423569857,8.01583057683878,-36.1240522211956));
#10859=CARTESIAN_POINT('Ctrl Pts',(6.26141987741361,8.10921506409678,-36.1813336075041));
#10860=CARTESIAN_POINT('Ctrl Pts',(6.31229445463966,8.20288299221516,-36.2366721483496));
#10861=CARTESIAN_POINT('Ctrl Pts',(6.36402406580065,8.29812516942855,-36.292940747643));
#10862=CARTESIAN_POINT('Ctrl Pts',(6.41969173269114,8.39366006532512,-36.3472003412414));
#10863=CARTESIAN_POINT('Ctrl Pts',(6.47922558197449,8.48908360808729,-36.3991269669699));
#10864=CARTESIAN_POINT('Ctrl Pts',(6.53926650008992,8.58531990367772,-36.4514958683748));
#10865=CARTESIAN_POINT('Ctrl Pts',(6.60323963771704,8.68144252075522,-36.5014915701884));
#10866=CARTESIAN_POINT('Ctrl Pts',(6.67102226578152,8.77702401760362,-36.5487983543211));
#10867=CARTESIAN_POINT('Ctrl Pts',(6.73940230766558,8.87344793837014,-36.5965220849105));
#10868=CARTESIAN_POINT('Ctrl Pts',(6.81165913892316,8.96932067906961,-36.6415089425263));
#10869=CARTESIAN_POINT('Ctrl Pts',(6.88761899105827,9.06419708736885,-36.6834566789171));
#10870=CARTESIAN_POINT('Ctrl Pts',(6.91875332267609,9.10308491397287,-36.7006501659855));
#10871=CARTESIAN_POINT('Ctrl Pts',(6.95050922414792,9.14180532432155,-36.7173333620177));
#10872=CARTESIAN_POINT('Ctrl Pts',(6.9828725406278,9.18032765868873,-36.7334867131338));
#10873=CARTESIAN_POINT('Ctrl Pts',(7.0606546653326,9.2729123917006,-36.7723097420312));
#10874=CARTESIAN_POINT('Ctrl Pts',(7.14193522550624,9.36433490372311,-36.8080617552203));
#10875=CARTESIAN_POINT('Ctrl Pts',(7.22639353034854,9.45421392953721,-36.8405831329123));
#10876=CARTESIAN_POINT('Ctrl Pts',(7.31498815818571,9.54849475671266,-36.8746972364189));
#10877=CARTESIAN_POINT('Ctrl Pts',(7.40707923745448,9.6410765981505,-36.9052560617216));
#10878=CARTESIAN_POINT('Ctrl Pts',(7.50225232380081,9.73153397866191,-36.9321141600718));
#10879=CARTESIAN_POINT('Ctrl Pts',(7.59398106932713,9.81871768107662,-36.9580002562726));
#10880=CARTESIAN_POINT('Ctrl Pts',(7.68857206544245,9.90392756518769,-36.9804487410988));
#10881=CARTESIAN_POINT('Ctrl Pts',(7.78562171747729,9.9868027322504,-36.9993663118188));
#10882=CARTESIAN_POINT('Ctrl Pts',(7.8822623010229,10.0693285768923,-37.0182041441584));
#10883=CARTESIAN_POINT('Ctrl Pts',(7.9813403510451,10.1495389355616,-37.0335406880041));
#10884=CARTESIAN_POINT('Ctrl Pts',(8.08243321549461,10.22710339482,-37.0453212245677));
#10885=CARTESIAN_POINT('Ctrl Pts',(8.18238435350325,10.3037918536358,-37.0569687136589));
#10886=CARTESIAN_POINT('Ctrl Pts',(8.28430455193243,10.3778935080232,-37.0651400528611));
#10887=CARTESIAN_POINT('Ctrl Pts',(8.38776919351014,10.4491198811163,-37.069819589999));
#10888=CARTESIAN_POINT('Ctrl Pts',(8.40167504207419,10.4586928438492,-37.0704485288693));
#10889=CARTESIAN_POINT('Ctrl Pts',(8.41560877167175,10.4682139182192,-37.0710144479744));
#10890=CARTESIAN_POINT('Ctrl Pts',(8.42956933641895,10.4776824519193,-37.0715173614427));
#10891=CARTESIAN_POINT('Ctrl Pts',(8.53515074276891,10.5492913819469,-37.0753208115339));
#10892=CARTESIAN_POINT('Ctrl Pts',(8.64225116327509,10.6178811928981,-37.0755170775842));
#10893=CARTESIAN_POINT('Ctrl Pts',(8.75036064416794,10.6832715284068,-37.0722375676082));
#10894=CARTESIAN_POINT('Ctrl Pts',(8.86231822477821,10.750989398277,-37.0688413252115));
#10895=CARTESIAN_POINT('Ctrl Pts',(8.97535731700476,10.8152754682094,-37.0617173928375));
#10896=CARTESIAN_POINT('Ctrl Pts',(9.08891450935341,10.8759743328061,-37.0510506189198));
#10897=CARTESIAN_POINT('Ctrl Pts',(9.19619874745444,10.9333201627546,-37.0409730827541));
#10898=CARTESIAN_POINT('Ctrl Pts',(9.30394500151872,10.987464371858,-37.027733748746));
#10899=CARTESIAN_POINT('Ctrl Pts',(9.41168854167092,11.0383162475307,-37.0115189784432));
#10900=CARTESIAN_POINT('Ctrl Pts',(9.51841693092913,11.0886890009566,-36.9954569823907));
#10901=CARTESIAN_POINT('Ctrl Pts',(9.62514225221039,11.1358311057255,-36.9764755314237));
#10902=CARTESIAN_POINT('Ctrl Pts',(9.73142938426382,11.1796944882344,-36.9547824460035));
#10903=CARTESIAN_POINT('Ctrl Pts',(9.83642685368137,11.2230256429523,-36.9333525792928));
#10904=CARTESIAN_POINT('Ctrl Pts',(9.94099637984871,11.2631571549129,-36.9092766665007));
#10905=CARTESIAN_POINT('Ctrl Pts',(10.0447401308733,11.3000824629307,-36.8827785309411));
#10906=CARTESIAN_POINT('Ctrl Pts',(10.0666087164143,11.3078661053095,-36.8771928764951));
#10907=CARTESIAN_POINT('Ctrl Pts',(10.0884406962621,11.3155074248244,-36.8714996709173));
#10908=CARTESIAN_POINT('Ctrl Pts',(10.1102324887059,11.3230065889554,-36.865701134163));
#10909=CARTESIAN_POINT('',(11.9501151712097,11.6489333498058,-36.0982066328345));
#10910=CARTESIAN_POINT('Origin',(10.3841046135622,7.6499999999151,-33.3857967817529));
#10911=CARTESIAN_POINT('',(19.1957890247762,-4.56844441699029,-48.648081882285));
#10912=CARTESIAN_POINT('',(19.1957890247762,-4.56844441699029,-48.648081882285));
#10913=CARTESIAN_POINT('Origin',(17.33160439086,-7.90000000000001,-45.419219381653));
#10914=CARTESIAN_POINT('',(13.0014773719379,-7.90000000000001,-47.919219381653));
#10915=CARTESIAN_POINT('Origin',(0.,24.9,0.));
#10916=CARTESIAN_POINT('',(-1.08087326492746E-15,25.4,-8.82600000000003));
#10917=CARTESIAN_POINT('',(-1.01964092497009E-15,24.9,-8.326));
#10918=CARTESIAN_POINT('Origin',(0.,25.4,0.));
#10919=CARTESIAN_POINT('Origin',(0.,13.15,0.));
#10920=CARTESIAN_POINT('',(1.82293408768471,12.6595351585866,-19.3672161093864));
#10921=CARTESIAN_POINT('',(-7.41942469371926E-7,12.7590298799455,-19.2383203234121));
#10922=CARTESIAN_POINT('Ctrl Pts',(1.82293408768471,12.6595351585866,-19.3672161093864));
#10923=CARTESIAN_POINT('Ctrl Pts',(1.78888997792411,12.6607896844181,-19.3640610554799));
#10924=CARTESIAN_POINT('Ctrl Pts',(1.75461498816483,12.6621343910058,-19.361044358231));
#10925=CARTESIAN_POINT('Ctrl Pts',(1.72025845212816,12.6635474656982,-19.358140139342));
#10926=CARTESIAN_POINT('Ctrl Pts',(1.68456107776077,12.6650156886952,-19.3551225770122));
#10927=CARTESIAN_POINT('Ctrl Pts',(1.6487753668818,12.6665577514038,-19.3522264959792));
#10928=CARTESIAN_POINT('Ctrl Pts',(1.61301220996673,12.6681551150688,-19.3494277462689));
#10929=CARTESIAN_POINT('Ctrl Pts',(1.57497663282431,12.669853976527,-19.3464511617138));
#10930=CARTESIAN_POINT('Ctrl Pts',(1.53696644084721,12.6716154025952,-19.3435847123621));
#10931=CARTESIAN_POINT('Ctrl Pts',(1.49905533094398,12.6734233512426,-19.3408040316618));
#10932=CARTESIAN_POINT('Ctrl Pts',(1.45973281213481,12.6752986087826,-19.3379198278117));
#10933=CARTESIAN_POINT('Ctrl Pts',(1.42051649491172,12.6772239582494,-19.3351279625462));
#10934=CARTESIAN_POINT('Ctrl Pts',(1.38143082867857,12.6791875669107,-19.3324052587621));
#10935=CARTESIAN_POINT('Ctrl Pts',(1.34004990580164,12.6812664860236,-19.3295226676189));
#10936=CARTESIAN_POINT('Ctrl Pts',(1.29881519384669,12.683388313637,-19.3267176591772));
#10937=CARTESIAN_POINT('Ctrl Pts',(1.25769687566335,12.6855451971966,-19.3239661713634));
#10938=CARTESIAN_POINT('Ctrl Pts',(1.23647135280047,12.6866585934474,-19.3225458368245));
#10939=CARTESIAN_POINT('Ctrl Pts',(1.2152759371352,12.6877814266293,-19.3211398124163));
#10940=CARTESIAN_POINT('Ctrl Pts',(1.19410123994597,12.6889131739459,-19.3197450375488));
#10941=CARTESIAN_POINT('Ctrl Pts',(1.14719948359475,12.6914199836738,-19.3166556242542));
#10942=CARTESIAN_POINT('Ctrl Pts',(1.10043265364891,12.6939663244445,-19.3136179280417));
#10943=CARTESIAN_POINT('Ctrl Pts',(1.05358207653531,12.6965557025242,-19.3105915433049));
#10944=CARTESIAN_POINT('Ctrl Pts',(1.02728833978127,12.6980089274316,-19.3088930591348));
#10945=CARTESIAN_POINT('Ctrl Pts',(1.00096726291399,12.699475822638,-19.3071982112495));
#10946=CARTESIAN_POINT('Ctrl Pts',(0.974573185146914,12.7009578120448,-19.3055001747126));
#10947=CARTESIAN_POINT('Ctrl Pts',(0.956266388874189,12.7019857122574,-19.3043224253243));
#10948=CARTESIAN_POINT('Ctrl Pts',(0.937924370736718,12.7030208856048,-19.30314314581));
#10949=CARTESIAN_POINT('Ctrl Pts',(0.91953055081917,12.7040639541404,-19.30196006824));
#10950=CARTESIAN_POINT('Ctrl Pts',(0.910862311987517,12.7045555087618,-19.3014025332104));
#10951=CARTESIAN_POINT('Ctrl Pts',(0.902182660540566,12.7050488136889,-19.3008441612167));
#10952=CARTESIAN_POINT('Ctrl Pts',(0.893505909217807,12.705543019972,-19.3002857525201));
#10953=CARTESIAN_POINT('Ctrl Pts',(0.822076183406764,12.7096114803876,-19.2956887577922));
#10954=CARTESIAN_POINT('Ctrl Pts',(0.750602616626036,12.7137542634669,-19.2910724211421));
#10955=CARTESIAN_POINT('Ctrl Pts',(0.679155770279492,12.717948730176,-19.2863841545952));
#10956=CARTESIAN_POINT('Ctrl Pts',(0.605333316726877,12.7222826628776,-19.2815400032141));
#10957=CARTESIAN_POINT('Ctrl Pts',(0.53153928875299,12.7266718216052,-19.2766193209322));
#10958=CARTESIAN_POINT('Ctrl Pts',(0.457798195777434,12.7310987618933,-19.2715763930781));
#10959=CARTESIAN_POINT('Ctrl Pts',(0.444313844229887,12.7319082755134,-19.2706542395099));
#10960=CARTESIAN_POINT('Ctrl Pts',(0.430831125913135,12.7327190709993,-19.2697280242799));
#10961=CARTESIAN_POINT('Ctrl Pts',(0.417350010399558,12.733531065795,-19.268797499997));
#10962=CARTESIAN_POINT('Ctrl Pts',(0.343529011221796,12.7379774535652,-19.2637020587293));
#10963=CARTESIAN_POINT('Ctrl Pts',(0.26971644232983,12.7424626536921,-19.2584731521507));
#10964=CARTESIAN_POINT('Ctrl Pts',(0.195920274301196,12.7469772849337,-19.2530745663503));
#10965=CARTESIAN_POINT('Ctrl Pts',(0.13061107197285,12.7509727087215,-19.2482968476456));
#10966=CARTESIAN_POINT('Ctrl Pts',(0.0653136611866498,12.7549912939957,
-19.2433864290818));
#10967=CARTESIAN_POINT('Ctrl Pts',(-1.16478701239764E-7,12.7590298412712,
-19.2383203719261));
#10968=CARTESIAN_POINT('',(-6.07314264709754,13.15,-18.0560083736136));
#10969=CARTESIAN_POINT('Ctrl Pts',(-1.36740623685183E-6,12.7590299186198,
-19.238320274898));
#10970=CARTESIAN_POINT('Ctrl Pts',(-0.0976846971834283,12.7650699730032,
-19.2307434734679));
#10971=CARTESIAN_POINT('Ctrl Pts',(-0.195826602486313,12.7711799956073,
-19.2227859628905));
#10972=CARTESIAN_POINT('Ctrl Pts',(-0.294252134116968,12.7773367444421,
-19.2143959580921));
#10973=CARTESIAN_POINT('Ctrl Pts',(-0.359553588796595,12.7814215042431,
-19.2088295211217));
#10974=CARTESIAN_POINT('Ctrl Pts',(-0.424981033355307,12.7855269574494,
-19.2030729859267));
#10975=CARTESIAN_POINT('Ctrl Pts',(-0.490495587159556,12.7896476277827,
-19.1971137495186));
#10976=CARTESIAN_POINT('Ctrl Pts',(-0.602712929565564,12.7967057644391,
-19.1869064042244));
#10977=CARTESIAN_POINT('Ctrl Pts',(-0.714605986300817,12.8037719382783,
-19.1761531494054));
#10978=CARTESIAN_POINT('Ctrl Pts',(-0.82612323045651,12.8108347372977,-19.1648175733631));
#10979=CARTESIAN_POINT('Ctrl Pts',(-0.943193195446338,12.8182492106394,
-19.1529175708078));
#10980=CARTESIAN_POINT('Ctrl Pts',(-1.0598491202423,12.8256599893232,-19.1403761143674));
#10981=CARTESIAN_POINT('Ctrl Pts',(-1.17609035809504,12.8330594679584,-19.1271552243471));
#10982=CARTESIAN_POINT('Ctrl Pts',(-1.2847832692999,12.8399784485982,-19.11479285578));
#10983=CARTESIAN_POINT('Ctrl Pts',(-1.39311451381811,12.8468876427769,-19.1018366670684));
#10984=CARTESIAN_POINT('Ctrl Pts',(-1.50112450746874,12.8537845810569,-19.08825515445));
#10985=CARTESIAN_POINT('Ctrl Pts',(-1.62066135458927,12.8614175623108,-19.0732242194165));
#10986=CARTESIAN_POINT('Ctrl Pts',(-1.73981679586176,12.869034758093,-19.0574096075086));
#10987=CARTESIAN_POINT('Ctrl Pts',(-1.85866951308033,12.8766408833612,-19.0407937879716));
#10988=CARTESIAN_POINT('Ctrl Pts',(-1.9837153295282,12.884643343603,-19.023312162237));
#10989=CARTESIAN_POINT('Ctrl Pts',(-2.10842629293182,12.8926335674546,-19.0049439848625));
#10990=CARTESIAN_POINT('Ctrl Pts',(-2.23294928564757,12.9006206698086,-18.9856519958004));
#10991=CARTESIAN_POINT('Ctrl Pts',(-2.36105802888851,12.9088377678914,-18.9658044767241));
#10992=CARTESIAN_POINT('Ctrl Pts',(-2.48896829721021,12.9170515954563,-18.9449794918307));
#10993=CARTESIAN_POINT('Ctrl Pts',(-2.61689111717973,12.9252753964184,-18.9231141413901));
#10994=CARTESIAN_POINT('Ctrl Pts',(-2.74926523716585,12.9337853590314,-18.9004879475377));
#10995=CARTESIAN_POINT('Ctrl Pts',(-2.8816532683033,12.9423060343459,-18.8767481373003));
#10996=CARTESIAN_POINT('Ctrl Pts',(-3.01433566154705,12.9508550880408,-18.8517957698283));
#10997=CARTESIAN_POINT('Ctrl Pts',(-3.03374933409837,12.9521059588233,-18.8481448175079));
#10998=CARTESIAN_POINT('Ctrl Pts',(-3.05316937993749,12.953357441682,-18.8444678500867));
#10999=CARTESIAN_POINT('Ctrl Pts',(-3.07259674806375,12.9546095964169,-18.8407644990186));
#11000=CARTESIAN_POINT('Ctrl Pts',(-3.23684149935945,12.9651956851594,-18.8094552670537));
#11001=CARTESIAN_POINT('Ctrl Pts',(-3.40082753073851,12.9757755153363,-18.7764116206451));
#11002=CARTESIAN_POINT('Ctrl Pts',(-3.56454054604347,12.9863481136657,-18.7415646366649));
#11003=CARTESIAN_POINT('Ctrl Pts',(-3.6174038037455,12.9897620266586,-18.7303124763473));
#11004=CARTESIAN_POINT('Ctrl Pts',(-3.67023898229499,12.9931752118673,-18.7188721447255));
#11005=CARTESIAN_POINT('Ctrl Pts',(-3.72304664363111,12.9965877069929,-18.7072408831335));
#11006=CARTESIAN_POINT('Ctrl Pts',(-3.88049171455976,13.0067619984406,-18.6725624906427));
#11007=CARTESIAN_POINT('Ctrl Pts',(-4.0376742623794,13.0169318588212,-18.6361554750793));
#11008=CARTESIAN_POINT('Ctrl Pts',(-4.19448641334882,13.0270950616618,-18.5980827891145));
#11009=CARTESIAN_POINT('Ctrl Pts',(-4.36539686099497,13.0381719937508,-18.5565871539797));
#11010=CARTESIAN_POINT('Ctrl Pts',(-4.53586787392932,13.0492410451786,-18.5131132431364));
#11011=CARTESIAN_POINT('Ctrl Pts',(-4.70580770848692,13.060302140562,-18.4677001278632));
#11012=CARTESIAN_POINT('Ctrl Pts',(-4.88444462846006,13.071929314473,-18.4199628856803));
#11013=CARTESIAN_POINT('Ctrl Pts',(-5.06249585260001,13.0835477606057,-18.3700830167689));
#11014=CARTESIAN_POINT('Ctrl Pts',(-5.23989080423082,13.0951596114433,-18.3180572321707));
#11015=CARTESIAN_POINT('Ctrl Pts',(-5.42489221768705,13.1072693631474,-18.2638006504677));
#11016=CARTESIAN_POINT('Ctrl Pts',(-5.60918160043135,13.1193720281311,-18.2072102845129));
#11017=CARTESIAN_POINT('Ctrl Pts',(-5.79269367431625,13.1314711984988,-18.1482289026053));
#11018=CARTESIAN_POINT('Ctrl Pts',(-5.88638240479708,13.1376482084777,-18.118117037615));
#11019=CARTESIAN_POINT('Ctrl Pts',(-5.97986860207494,13.1438243177559,-18.0873811205117));
#11020=CARTESIAN_POINT('Ctrl Pts',(-6.07314264709754,13.15,-18.0560083736136));
#11021=CARTESIAN_POINT('',(18.6735332660427,13.15,-3.76850837361349));
#11022=CARTESIAN_POINT('Origin',(0.,13.15,0.));
#11023=CARTESIAN_POINT('',(15.8610341074696,12.6595351585866,-11.2623152840526));
#11024=CARTESIAN_POINT('Ctrl Pts',(18.6735332660427,13.15,-3.76850837361349));
#11025=CARTESIAN_POINT('Ctrl Pts',(18.635609003944,13.1379692270563,-3.95642887150844));
#11026=CARTESIAN_POINT('Ctrl Pts',(18.595290610597,13.1259554920877,-4.14350652629558));
#11027=CARTESIAN_POINT('Ctrl Pts',(18.5526294017364,13.1139455297031,-4.32990938943143));
#11028=CARTESIAN_POINT('Ctrl Pts',(18.5107522750365,13.10215630174,-4.51288630277349));
#11029=CARTESIAN_POINT('Ctrl Pts',(18.4666170044181,13.0903706662367,-4.69521392858484));
#11030=CARTESIAN_POINT('Ctrl Pts',(18.4202313065065,13.0785760987623,-4.87702411982452));
#11031=CARTESIAN_POINT('Ctrl Pts',(18.3751916837961,13.0671238000367,-5.0535583272856));
#11032=CARTESIAN_POINT('Ctrl Pts',(18.3280297551566,13.0556630399901,-5.22960544275274));
#11033=CARTESIAN_POINT('Ctrl Pts',(18.2787228864419,13.0441829769088,-5.4052483437446));
#11034=CARTESIAN_POINT('Ctrl Pts',(18.2319440507293,13.0332915129232,-5.57188578440453));
#11035=CARTESIAN_POINT('Ctrl Pts',(18.1832340569148,13.0223826439743,-5.73815981936693));
#11036=CARTESIAN_POINT('Ctrl Pts',(18.132554518669,13.0114481775998,-5.90409869240932));
#11037=CARTESIAN_POINT('Ctrl Pts',(18.1097293612668,13.0065234895551,-5.97883459228983));
#11038=CARTESIAN_POINT('Ctrl Pts',(18.0865044745234,13.0015936267203,-6.0535018781925));
#11039=CARTESIAN_POINT('Ctrl Pts',(18.0628754032633,12.9966579427863,-6.12809973553589));
#11040=CARTESIAN_POINT('Ctrl Pts',(18.0183561237835,12.9873586736755,-6.26864875767551));
#11041=CARTESIAN_POINT('Ctrl Pts',(17.972373035958,12.9780292666563,-6.40910769298485));
#11042=CARTESIAN_POINT('Ctrl Pts',(17.9250244537378,12.9686821009643,-6.54928034556807));
#11043=CARTESIAN_POINT('Ctrl Pts',(17.8807222934487,12.9599363347065,-6.68043424779068));
#11044=CARTESIAN_POINT('Ctrl Pts',(17.8352244399587,12.9511750020392,-6.81133765846827));
#11045=CARTESIAN_POINT('Ctrl Pts',(17.7886209010951,12.9424107435037,-6.94178628068565));
#11046=CARTESIAN_POINT('Ctrl Pts',(17.7539427147616,12.9358891660017,-7.03885448062299));
#11047=CARTESIAN_POINT('Ctrl Pts',(17.7186524670563,12.9293660137816,-7.13567005199129));
#11048=CARTESIAN_POINT('Ctrl Pts',(17.6827922878973,12.9228475964183,-7.23213062593721));
#11049=CARTESIAN_POINT('Ctrl Pts',(17.6352878328313,12.9142125624615,-7.35991322792396));
#11050=CARTESIAN_POINT('Ctrl Pts',(17.5867942563818,12.9055857664759,-7.48707423642674));
#11051=CARTESIAN_POINT('Ctrl Pts',(17.5373852100854,12.8969734463818,-7.61356929829063));
#11052=CARTESIAN_POINT('Ctrl Pts',(17.4919426291,12.8890525071474,-7.72990957449293));
#11053=CARTESIAN_POINT('Ctrl Pts',(17.4456790187502,12.8811371827701,-7.84580544759027));
#11054=CARTESIAN_POINT('Ctrl Pts',(17.3985927372716,12.8732239828729,-7.96135319383724));
#11055=CARTESIAN_POINT('Ctrl Pts',(17.3588829295431,12.8665504542662,-8.05879938501738));
#11056=CARTESIAN_POINT('Ctrl Pts',(17.3185880217668,12.8598784744127,-8.15599735052392));
#11057=CARTESIAN_POINT('Ctrl Pts',(17.2777163855609,12.8532079839213,-8.25297752920841));
#11058=CARTESIAN_POINT('Ctrl Pts',(17.2313167512056,12.845635291744,-8.36307453653147));
#11059=CARTESIAN_POINT('Ctrl Pts',(17.1841737380798,12.8380640091309,-8.47289269012394));
#11060=CARTESIAN_POINT('Ctrl Pts',(17.1363234461559,12.8305004633246,-8.5824610079591));
#11061=CARTESIAN_POINT('Ctrl Pts',(17.0906598957075,12.8232825688958,-8.68702209228785));
#11062=CARTESIAN_POINT('Ctrl Pts',(17.0443519564341,12.8160717028972,-8.7913556001471));
#11063=CARTESIAN_POINT('Ctrl Pts',(16.997455397443,12.8088775452789,-8.89544771685909));
#11064=CARTESIAN_POINT('Ctrl Pts',(16.9549407548744,12.8023555947072,-8.98981368381757));
#11065=CARTESIAN_POINT('Ctrl Pts',(16.9119423673544,12.7958473962748,-9.08398094533463));
#11066=CARTESIAN_POINT('Ctrl Pts',(16.8685236708355,12.7893635951273,-9.17790944158495));
#11067=CARTESIAN_POINT('Ctrl Pts',(16.831166098439,12.7837849138173,-9.25872579214598));
#11068=CARTESIAN_POINT('Ctrl Pts',(16.7934219290083,12.7782136874733,-9.33951840434077));
#11069=CARTESIAN_POINT('Ctrl Pts',(16.7554251187229,12.7726724740285,-9.42009967844722));
#11070=CARTESIAN_POINT('Ctrl Pts',(16.7500131624358,12.771883228702,-9.43157701903831));
#11071=CARTESIAN_POINT('Ctrl Pts',(16.7445961295867,12.7710945998699,-9.44305000107886));
#11072=CARTESIAN_POINT('Ctrl Pts',(16.7391744571789,12.7703066605067,-9.45451800992888));
#11073=CARTESIAN_POINT('Ctrl Pts',(16.7095471419653,12.7660008806425,-9.51718618452878));
#11074=CARTESIAN_POINT('Ctrl Pts',(16.6797728051853,12.7617151304109,-9.57972202319642));
#11075=CARTESIAN_POINT('Ctrl Pts',(16.6498373535122,12.757449305424,-9.64220564374232));
#11076=CARTESIAN_POINT('Ctrl Pts',(16.6211714013588,12.7533643850993,-9.70203946540951));
#11077=CARTESIAN_POINT('Ctrl Pts',(16.5923573963794,12.7492976981851,-9.76182568605953));
#11078=CARTESIAN_POINT('Ctrl Pts',(16.5634043886492,12.7452532521653,-9.82159229151741));
#11079=CARTESIAN_POINT('Ctrl Pts',(16.5359798968833,12.7414223245601,-9.87820363893009));
#11080=CARTESIAN_POINT('Ctrl Pts',(16.5084304766136,12.7376113278547,-9.93479754780587));
#11081=CARTESIAN_POINT('Ctrl Pts',(16.4807870976986,12.7338278436748,-9.9913559826116));
#11082=CARTESIAN_POINT('Ctrl Pts',(16.479246381964,12.7336169695401,-9.99450829154966));
#11083=CARTESIAN_POINT('Ctrl Pts',(16.4777053811798,12.7334061820622,-9.99766047853941));
#11084=CARTESIAN_POINT('Ctrl Pts',(16.4761641031983,12.7331954829858,-10.0008125362049));
#11085=CARTESIAN_POINT('Ctrl Pts',(16.4461689478205,12.7290950211555,-10.0621554351298));
#11086=CARTESIAN_POINT('Ctrl Pts',(16.4160888758792,12.725029433906,-10.1234195935806));
#11087=CARTESIAN_POINT('Ctrl Pts',(16.3859390142828,12.7210081247693,-10.1846516877651));
#11088=CARTESIAN_POINT('Ctrl Pts',(16.3574486213335,12.7172081511904,-10.2425135263293));
#11089=CARTESIAN_POINT('Ctrl Pts',(16.3288958340789,12.7134477064406,-10.3003465245089));
#11090=CARTESIAN_POINT('Ctrl Pts',(16.3003198960741,12.7097399996136,-10.358156854131));
#11091=CARTESIAN_POINT('Ctrl Pts',(16.2762833586279,12.7066212766527,-10.4067837846802));
#11092=CARTESIAN_POINT('Ctrl Pts',(16.2523127582846,12.7035507329856,-10.4552276437463));
#11093=CARTESIAN_POINT('Ctrl Pts',(16.2283644290953,12.7005283628054,-10.5036422639959));
#11094=CARTESIAN_POINT('Ctrl Pts',(16.2050726155633,12.6975888473968,-10.5507296536072));
#11095=CARTESIAN_POINT('Ctrl Pts',(16.1818016507761,12.6946948638812,-10.5977893480704));
#11096=CARTESIAN_POINT('Ctrl Pts',(16.1585395211624,12.6918520765314,-10.6449228641774));
#11097=CARTESIAN_POINT('Ctrl Pts',(16.1500867003578,12.690819085466,-10.6620498930506));
#11098=CARTESIAN_POINT('Ctrl Pts',(16.1416353373009,12.6897929124041,-10.6791862812815));
#11099=CARTESIAN_POINT('Ctrl Pts',(16.133185909691,12.6887740383049,-10.6963355459743));
#11100=CARTESIAN_POINT('Ctrl Pts',(16.1101815887034,12.68600006261,-10.7430259500949));
#11101=CARTESIAN_POINT('Ctrl Pts',(16.0871876783737,12.6832787578847,-10.7898158379825));
#11102=CARTESIAN_POINT('Ctrl Pts',(16.064233957608,12.6806283209993,-10.8367452553848));
#11103=CARTESIAN_POINT('Ctrl Pts',(16.0426664098205,12.6781379437413,-10.8808406098069));
#11104=CARTESIAN_POINT('Ctrl Pts',(16.0211342964406,12.675710111483,-10.9250589443984));
#11105=CARTESIAN_POINT('Ctrl Pts',(15.9996942678004,12.6733674903699,-10.9693973797136));
#11106=CARTESIAN_POINT('Ctrl Pts',(15.9787445551771,12.6710784430964,-11.0127218310757));
#11107=CARTESIAN_POINT('Ctrl Pts',(15.9578825024016,12.6688706813128,-11.0561609810969));
#11108=CARTESIAN_POINT('Ctrl Pts',(15.9371949671836,12.6667735640339,-11.0996774884489));
#11109=CARTESIAN_POINT('Ctrl Pts',(15.917184796503,12.6647451119131,-11.1417691504261));
#11110=CARTESIAN_POINT('Ctrl Pts',(15.8973376991438,12.6628201182914,-11.1839331484321));
#11111=CARTESIAN_POINT('Ctrl Pts',(15.8777677308615,12.6610338566175,-11.2261030546386));
#11112=CARTESIAN_POINT('Ctrl Pts',(15.8721658177008,12.6605225383244,-11.2381742112781));
#11113=CARTESIAN_POINT('Ctrl Pts',(15.8665868518027,12.6600226469234,-11.250245643483));
#11114=CARTESIAN_POINT('Ctrl Pts',(15.8610341074696,12.6595351585866,-11.2623152840526));
#11115=CARTESIAN_POINT('',(15.6532787469445,12.65,-11.7122740947458));
#11116=CARTESIAN_POINT('Ctrl Pts',(15.8610341074696,12.6595351585866,-11.2623152840526));
#11117=CARTESIAN_POINT('Ctrl Pts',(15.8165145702369,12.655626684734,-11.3590845188816));
#11118=CARTESIAN_POINT('Ctrl Pts',(15.7718505903917,12.6527974939087,-11.4558489811135));
#11119=CARTESIAN_POINT('Ctrl Pts',(15.7271279180831,12.6512766915384,-11.5525992725652));
#11120=CARTESIAN_POINT('Ctrl Pts',(15.7025232501934,12.6504400054614,-11.6058275048357));
#11121=CARTESIAN_POINT('Ctrl Pts',(15.6779011866278,12.65,-11.6590517667082));
#11122=CARTESIAN_POINT('Ctrl Pts',(15.6532787469445,12.65,-11.7122740947458));
#11123=CARTESIAN_POINT('',(2.31648752866421,12.65,-19.4122740947459));
#11124=CARTESIAN_POINT('Origin',(0.,12.65,0.));
#11125=CARTESIAN_POINT('Ctrl Pts',(2.31648752866421,12.65,-19.4122740947459));
#11126=CARTESIAN_POINT('Ctrl Pts',(2.2103311248206,12.65,-19.4026632604047));
#11127=CARTESIAN_POINT('Ctrl Pts',(2.10416883388078,12.6514513272156,-19.3930461613134));
#11128=CARTESIAN_POINT('Ctrl Pts',(1.99804499033973,12.6541030519185,-19.3833359160023));
#11129=CARTESIAN_POINT('Ctrl Pts',(1.93965979583085,12.6555619272985,-19.3779937182238));
#11130=CARTESIAN_POINT('Ctrl Pts',(1.881286570062,12.6573848689003,-19.3726239534149));
#11131=CARTESIAN_POINT('Ctrl Pts',(1.82293408768471,12.6595351585866,-19.3672161093864));
#11132=CARTESIAN_POINT('Origin',(0.,-23.4,0.));
#11133=CARTESIAN_POINT('',(-2.42665362134782,-22.9,19.3988105873015));
#11134=CARTESIAN_POINT('',(18.0131895824794,-22.9,7.59786161137834));
#11135=CARTESIAN_POINT('Origin',(4.90959474333048E-17,-22.9,8.50366754002165E-17));
#11136=CARTESIAN_POINT('',(-6.07314264709777,-23.4,18.0560083736135));
#11137=CARTESIAN_POINT('Ctrl Pts',(-2.42665362134782,-22.9,19.3988105873015));
#11138=CARTESIAN_POINT('Ctrl Pts',(-2.49483230883249,-22.9,19.3675892623714));
#11139=CARTESIAN_POINT('Ctrl Pts',(-2.56318139468448,-22.9014413252167,
19.3371168853022));
#11140=CARTESIAN_POINT('Ctrl Pts',(-2.63168706866709,-22.9040302787143,
19.3072597052728));
#11141=CARTESIAN_POINT('Ctrl Pts',(-2.70103054707964,-22.9066508943588,
19.2770373806321));
#11142=CARTESIAN_POINT('Ctrl Pts',(-2.77053455038377,-22.9104479219792,
19.2474455750134));
#11143=CARTESIAN_POINT('Ctrl Pts',(-2.8402082733943,-22.9151689742963,19.2183597505841));
#11144=CARTESIAN_POINT('Ctrl Pts',(-2.91389838884986,-22.9201621751085,
19.187597252648));
#11145=CARTESIAN_POINT('Ctrl Pts',(-2.98777825664906,-22.9261892251367,
19.1574008581504));
#11146=CARTESIAN_POINT('Ctrl Pts',(-3.06188524730074,-22.9330040852335,
19.1276368660924));
#11147=CARTESIAN_POINT('Ctrl Pts',(-3.12537434075582,-22.9388425261926,
19.1021373975976));
#11148=CARTESIAN_POINT('Ctrl Pts',(-3.1890306252501,-22.9452603057855,19.0769556044239));
#11149=CARTESIAN_POINT('Ctrl Pts',(-3.2528923076016,-22.9521283804573,19.0520136663235));
#11150=CARTESIAN_POINT('Ctrl Pts',(-3.27850056656131,-22.9548824487541,
19.0420120568089));
#11151=CARTESIAN_POINT('Ctrl Pts',(-3.30407836463786,-22.957705512208,19.0320737013011));
#11152=CARTESIAN_POINT('Ctrl Pts',(-3.32962845656234,-22.960593031896,19.0221941700939));
#11153=CARTESIAN_POINT('Ctrl Pts',(-3.43797011955961,-22.9728371633792,
18.9803013720646));
#11154=CARTESIAN_POINT('Ctrl Pts',(-3.54647772773345,-22.9863118482884,
18.9392088437263));
#11155=CARTESIAN_POINT('Ctrl Pts',(-3.65506054302364,-23.000712480614,18.8987487638366));
#11156=CARTESIAN_POINT('Ctrl Pts',(-3.77015005916127,-23.0159760543387,
18.855864159998));
#11157=CARTESIAN_POINT('Ctrl Pts',(-3.8853241639595,-23.0322800742794,18.8136901601118));
#11158=CARTESIAN_POINT('Ctrl Pts',(-4.00050877634662,-23.0493077902531,
18.772042864334));
#11159=CARTESIAN_POINT('Ctrl Pts',(-4.0530285423963,-23.0570717757436,18.7530532945857));
#11160=CARTESIAN_POINT('Ctrl Pts',(-4.10555093233817,-23.0649868063103,
18.734173429334));
#11161=CARTESIAN_POINT('Ctrl Pts',(-4.15807096335396,-23.0730255541293,
18.715386756417));
#11162=CARTESIAN_POINT('Ctrl Pts',(-4.18604852539236,-23.0773078167531,
18.705379045133));
#11163=CARTESIAN_POINT('Ctrl Pts',(-4.21404153215336,-23.0816279527546,
18.6953900829876));
#11164=CARTESIAN_POINT('Ctrl Pts',(-4.24204848892154,-23.0859836968891,
18.6854192437152));
#11165=CARTESIAN_POINT('Ctrl Pts',(-4.36416486299477,-23.104975681077,18.6419442332563));
#11166=CARTESIAN_POINT('Ctrl Pts',(-4.48640499350052,-23.1246111362377,
18.598870351077));
#11167=CARTESIAN_POINT('Ctrl Pts',(-4.60869052279136,-23.1447278442301,
18.556125457237));
#11168=CARTESIAN_POINT('Ctrl Pts',(-4.74760212112971,-23.1675796409777,
18.5075689227186));
#11169=CARTESIAN_POINT('Ctrl Pts',(-4.886572286895,-23.1910529746397,18.4594369686117));
#11170=CARTESIAN_POINT('Ctrl Pts',(-5.02554817388977,-23.2149438103717,
18.4116315716704));
#11171=CARTESIAN_POINT('Ctrl Pts',(-5.18078521662232,-23.2416300418297,
18.3582326072292));
#11172=CARTESIAN_POINT('Ctrl Pts',(-5.33603027633239,-23.2688383566178,
18.3052415157176));
#11173=CARTESIAN_POINT('Ctrl Pts',(-5.49127574609483,-23.2963096837761,
18.2525271420218));
#11174=CARTESIAN_POINT('Ctrl Pts',(-5.68520897685116,-23.3306269700528,
18.1866761460876));
#11175=CARTESIAN_POINT('Ctrl Pts',(-5.87914576531621,-23.3653575842081,
18.1212592702554));
#11176=CARTESIAN_POINT('Ctrl Pts',(-6.07314264709777,-23.4,18.0560083736135));
#11177=CARTESIAN_POINT('',(-2.33295215237571E-15,-23.4,19.05));
#11178=CARTESIAN_POINT('Origin',(0.,-23.4,0.));
#11179=CARTESIAN_POINT('',(18.6735332660427,-23.4,3.76850837361377));
#11180=CARTESIAN_POINT('Origin',(0.,-23.4,0.));
#11181=CARTESIAN_POINT('Ctrl Pts',(18.6735332660427,-23.4,3.76850837361377));
#11182=CARTESIAN_POINT('Ctrl Pts',(18.6350144631045,-23.3670436986399,3.95937491196879));
#11183=CARTESIAN_POINT('Ctrl Pts',(18.5966676676154,-23.3340202715025,4.15019613839664));
#11184=CARTESIAN_POINT('Ctrl Pts',(18.5586614537198,-23.3013555121996,4.34116274406092));
#11185=CARTESIAN_POINT('Ctrl Pts',(18.5277984165564,-23.2748300160513,4.49623763428238));
#11186=CARTESIAN_POINT('Ctrl Pts',(18.4971580439715,-23.2485394308233,4.65140928850101));
#11187=CARTESIAN_POINT('Ctrl Pts',(18.4668399407577,-23.2227118267817,4.80675183465115));
#11188=CARTESIAN_POINT('Ctrl Pts',(18.4388540307315,-23.1988709882634,4.95014479327899));
#11189=CARTESIAN_POINT('Ctrl Pts',(18.4111419439031,-23.1754236716161,5.09368400762515));
#11190=CARTESIAN_POINT('Ctrl Pts',(18.3838068036978,-23.1525653654293,5.23739146952049));
#11191=CARTESIAN_POINT('Ctrl Pts',(18.359835246298,-23.1325197686369,5.36341576080758));
#11192=CARTESIAN_POINT('Ctrl Pts',(18.3361535391227,-23.1129267586639,5.48956941598828));
#11193=CARTESIAN_POINT('Ctrl Pts',(18.3128553330328,-23.0939393205251,5.61583514399125));
#11194=CARTESIAN_POINT('Ctrl Pts',(18.309586231902,-23.0912750872682,5.63355219193056));
#11195=CARTESIAN_POINT('Ctrl Pts',(18.3063247250108,-23.0886228202051,5.6512713887974));
#11196=CARTESIAN_POINT('Ctrl Pts',(18.3030711156135,-23.0859829876023,5.66899262803536));
#11197=CARTESIAN_POINT('Ctrl Pts',(18.2977029311688,-23.0816274837341,5.69823119640761));
#11198=CARTESIAN_POINT('Ctrl Pts',(18.2923574142506,-23.0773075842935,5.72746674517875));
#11199=CARTESIAN_POINT('Ctrl Pts',(18.2870358543619,-23.0730255541509,5.75669829321656));
#11200=CARTESIAN_POINT('Ctrl Pts',(18.2649583928884,-23.055260771366,5.877970700012));
#11201=CARTESIAN_POINT('Ctrl Pts',(18.2432675843708,-23.0380976121135,5.9994818912581));
#11202=CARTESIAN_POINT('Ctrl Pts',(18.2221517586248,-23.0218415529585,6.12126924644107));
#11203=CARTESIAN_POINT('Ctrl Pts',(18.2022839003277,-23.0065462439498,6.23585884119596));
#11204=CARTESIAN_POINT('Ctrl Pts',(18.1829249568717,-22.9920537993276,6.35069295735908));
#11205=CARTESIAN_POINT('Ctrl Pts',(18.1642557197366,-22.9786542883935,6.46578579604177));
#11206=CARTESIAN_POINT('Ctrl Pts',(18.1555179094392,-22.9723828813846,6.51965298856382));
#11207=CARTESIAN_POINT('Ctrl Pts',(18.1469315449829,-22.9663514277283,6.57357660250184));
#11208=CARTESIAN_POINT('Ctrl Pts',(18.1385172401805,-22.960592775276,6.62755666242319));
#11209=CARTESIAN_POINT('Ctrl Pts',(18.1342982464804,-22.9577053450025,6.65462265754528));
#11210=CARTESIAN_POINT('Ctrl Pts',(18.1301163408571,-22.9548823672323,6.68174205639669));
#11211=CARTESIAN_POINT('Ctrl Pts',(18.1259739819792,-22.9521283805007,6.70891945903846));
#11212=CARTESIAN_POINT('Ctrl Pts',(18.113919279733,-22.9441139879726,6.78800857379809));
#11213=CARTESIAN_POINT('Ctrl Pts',(18.1022868108286,-22.9367118504463,6.86701914290839));
#11214=CARTESIAN_POINT('Ctrl Pts',(18.0911547751198,-22.9301299080703,6.94606439194116));
#11215=CARTESIAN_POINT('Ctrl Pts',(18.0804160048456,-22.923780488343,7.02231718099403));
#11216=CARTESIAN_POINT('Ctrl Pts',(18.0701428237499,-22.9181939831416,7.09860216030664));
#11217=CARTESIAN_POINT('Ctrl Pts',(18.0604250099349,-22.9135965970109,7.17500646404394));
#11218=CARTESIAN_POINT('Ctrl Pts',(18.0512249388187,-22.9092441490059,7.24734012276077));
#11219=CARTESIAN_POINT('Ctrl Pts',(18.0425226047623,-22.9057780702216,7.31978062515643));
#11220=CARTESIAN_POINT('Ctrl Pts',(18.0344129323305,-22.9034297890292,7.39239005519619));
#11221=CARTESIAN_POINT('Ctrl Pts',(18.0267815700159,-22.9012200099356,7.46071696639418));
#11222=CARTESIAN_POINT('Ctrl Pts',(18.0196750266457,-22.9,7.52919337317792));
#11223=CARTESIAN_POINT('Ctrl Pts',(18.0131895824794,-22.9,7.59786161137834));
#11224=CARTESIAN_POINT('Origin',(0.,-23.4,0.));
#11225=CARTESIAN_POINT('',(-15.5865359611318,-22.9,-11.8009489759233));
#11226=CARTESIAN_POINT('',(-15.5865359611318,-22.9,11.8009489759233));
#11227=CARTESIAN_POINT('Origin',(-9.81918948666111E-17,-22.9,0.));
#11228=CARTESIAN_POINT('',(-12.6003906189451,-23.4,-14.2875));
#11229=CARTESIAN_POINT('Ctrl Pts',(-15.5865359611318,-22.9,-11.8009489759233));
#11230=CARTESIAN_POINT('Ctrl Pts',(-15.5254081568604,-22.9,-11.8443827888175));
#11231=CARTESIAN_POINT('Ctrl Pts',(-15.4648437612788,-22.9014413252167,
-11.8883386449565));
#11232=CARTESIAN_POINT('Ctrl Pts',(-15.4047338478967,-22.9040302787143,
-11.9327377089142));
#11233=CARTESIAN_POINT('Ctrl Pts',(-15.3438888077885,-22.9066508943588,
-11.9776797604873));
#11234=CARTESIAN_POINT('Ctrl Pts',(-15.2835095507252,-22.9104479219794,
-12.0230760902052));
#11235=CARTESIAN_POINT('Ctrl Pts',(-15.2234836263725,-22.9151689742967,
-12.068872392095));
#11236=CARTESIAN_POINT('Ctrl Pts',(-15.1599974639465,-22.920162175109,-12.1173086551203));
#11237=CARTESIAN_POINT('Ctrl Pts',(-15.0969066853077,-22.9261892251374,
-12.1661923002148));
#11238=CARTESIAN_POINT('Ctrl Pts',(-15.03407681674,-22.9330040852346,-12.2154888406893));
#11239=CARTESIAN_POINT('Ctrl Pts',(-14.9802490825162,-22.9388425261934,
-12.2577222742345));
#11240=CARTESIAN_POINT('Ctrl Pts',(-14.9266128676709,-22.9452603057859,
-12.3002593371276));
#11241=CARTESIAN_POINT('Ctrl Pts',(-14.8730816744838,-22.9521283804573,
-12.3430942073196));
#11242=CARTESIAN_POINT('Ctrl Pts',(-14.8516158970855,-22.9548824487541,
-12.3602708053681));
#11243=CARTESIAN_POINT('Ctrl Pts',(-14.8302201297056,-22.957705512208,-12.3774526505213));
#11244=CARTESIAN_POINT('Ctrl Pts',(-14.8088891587405,-22.960593031896,-12.3946399135934));
#11245=CARTESIAN_POINT('Ctrl Pts',(-14.7184380998966,-22.9728371633814,
-12.4675201470358));
#11246=CARTESIAN_POINT('Ctrl Pts',(-14.6285971223469,-22.9863118482931,
-12.5409442280624));
#11247=CARTESIAN_POINT('Ctrl Pts',(-14.5392662576623,-23.0007124806216,
-12.6147496645868));
#11248=CARTESIAN_POINT('Ctrl Pts',(-14.4445823432294,-23.015976054348,-12.6929778073595));
#11249=CARTESIAN_POINT('Ctrl Pts',(-14.350471535541,-23.0322800742906,-12.7716345080375));
#11250=CARTESIAN_POINT('Ctrl Pts',(-14.2568116131964,-23.0493077902663,
-12.8505636606085));
#11251=CARTESIAN_POINT('Ctrl Pts',(-14.2141062803874,-23.0570717757524,
-12.8865523273134));
#11252=CARTESIAN_POINT('Ctrl Pts',(-14.1714946425131,-23.0649868063146,
-12.9225981186239));
#11253=CARTESIAN_POINT('Ctrl Pts',(-14.1289648910311,-23.073025554129,-12.9586884632117));
#11254=CARTESIAN_POINT('Ctrl Pts',(-14.1063091778062,-23.0773078167528,
-12.9779138870309));
#11255=CARTESIAN_POINT('Ctrl Pts',(-14.0836619794504,-23.0816279527543,
-12.9971620609415));
#11256=CARTESIAN_POINT('Ctrl Pts',(-14.0610235009594,-23.0859836968888,
-13.0164313773492));
#11257=CARTESIAN_POINT('Ctrl Pts',(-13.9623148504585,-23.1049756810725,
-13.1004497542657));
#11258=CARTESIAN_POINT('Ctrl Pts',(-13.8638917090216,-23.1246111362285,
-13.1847758715363));
#11259=CARTESIAN_POINT('Ctrl Pts',(-13.7657307804515,-23.144727844216,-13.2693057994777));
#11260=CARTESIAN_POINT('Ctrl Pts',(-13.6542237888969,-23.1675796409578,
-13.3653285052362));
#11261=CARTESIAN_POINT('Ctrl Pts',(-13.5430552110511,-23.1910529746138,
-13.4616142220801));
#11262=CARTESIAN_POINT('Ctrl Pts',(-13.4321665793915,-23.2149438103394,
-13.5580681722366));
#11263=CARTESIAN_POINT('Ctrl Pts',(-13.3083031983276,-23.2416300417875,
-13.6658079125919));
#11264=CARTESIAN_POINT('Ctrl Pts',(-13.1847890370931,-23.2688383565652,
-13.7737585323181));
#11265=CARTESIAN_POINT('Ctrl Pts',(-13.0615143154905,-23.2963096837132,
-13.8818478660677));
#11266=CARTESIAN_POINT('Ctrl Pts',(-12.9075190646744,-23.3306269700103,
-14.0168734726555));
#11267=CARTESIAN_POINT('Ctrl Pts',(-12.753897994041,-23.3653575841868,-14.1521192203606));
#11268=CARTESIAN_POINT('Ctrl Pts',(-12.6003906189451,-23.4,-14.2875));
#11269=CARTESIAN_POINT('',(-12.6003906189451,-23.4,14.2875));
#11270=CARTESIAN_POINT('Origin',(0.,-23.4,0.));
#11271=CARTESIAN_POINT('Ctrl Pts',(-12.6003906189451,-23.4,14.2875));
#11272=CARTESIAN_POINT('Ctrl Pts',(-12.7464264885013,-23.3670436986217,
14.1587084688864));
#11273=CARTESIAN_POINT('Ctrl Pts',(-12.8925091205016,-23.3340202714665,
14.0300885565564));
#11274=CARTESIAN_POINT('Ctrl Pts',(-13.0388879454113,-23.3013555121465,
13.9016909069208));
#11275=CARTESIAN_POINT('Ctrl Pts',(-13.1577552213119,-23.2748300159846,
13.7974252875346));
#11276=CARTESIAN_POINT('Ctrl Pts',(-13.2768176295818,-23.2485394307436,
13.6933041193317));
#11277=CARTESIAN_POINT('Ctrl Pts',(-13.396189169292,-23.22271182669,13.5893765986257));
#11278=CARTESIAN_POINT('Ctrl Pts',(-13.5063781591052,-23.1988709881879,
13.4934436103423));
#11279=CARTESIAN_POINT('Ctrl Pts',(-13.6168307216849,-23.1754236715566,
13.3976746320453));
#11280=CARTESIAN_POINT('Ctrl Pts',(-13.7276174642274,-23.1525653653853,
13.3021479753249));
#11281=CARTESIAN_POINT('Ctrl Pts',(-13.8247719233332,-23.1325197685822,
13.2183758519566));
#11282=CARTESIAN_POINT('Ctrl Pts',(-13.9221833399697,-23.112926758599,13.1347900642995));
#11283=CARTESIAN_POINT('Ctrl Pts',(-14.0198835650604,-23.093939320451,13.0514803619139));
#11284=CARTESIAN_POINT('Ctrl Pts',(-14.0335924279632,-23.0912750872191,
13.0397907134262));
#11285=CARTESIAN_POINT('Ctrl Pts',(-14.0473069490115,-23.0886228201808,
13.0281065672791));
#11286=CARTESIAN_POINT('Ctrl Pts',(-14.0610271875519,-23.0859829876025,
13.0164282393766));
#11287=CARTESIAN_POINT('Ctrl Pts',(-14.0836644383102,-23.0816274837344,
12.9971599710891));
#11288=CARTESIAN_POINT('Ctrl Pts',(-14.1063104077805,-23.0773075842938,
12.9779128432561));
#11289=CARTESIAN_POINT('Ctrl Pts',(-14.1289648910289,-23.0730255541512,
12.9586884631858));
#11290=CARTESIAN_POINT('Ctrl Pts',(-14.2229511453529,-23.0552607713666,
12.8789326173029));
#11291=CARTESIAN_POINT('Ctrl Pts',(-14.317337519555,-23.0380976121144,12.7993922304769));
#11292=CARTESIAN_POINT('Ctrl Pts',(-14.412250550128,-23.0218415529598,12.7202117113694));
#11293=CARTESIAN_POINT('Ctrl Pts',(-14.5015541210375,-23.0065462439525,
12.6457108439954));
#11294=CARTESIAN_POINT('Ctrl Pts',(-14.5913239111188,-22.9920537993316,
12.5715284490981));
#11295=CARTESIAN_POINT('Ctrl Pts',(-14.6816626146348,-22.9786542883986,
12.4978139961358));
#11296=CARTESIAN_POINT('Ctrl Pts',(-14.7239440666521,-22.9723828813878,
12.4633132341744));
#11297=CARTESIAN_POINT('Ctrl Pts',(-14.7663501039695,-22.9663514277299,
12.4289154174509));
#11298=CARTESIAN_POINT('Ctrl Pts',(-14.8088910547694,-22.960592775276,12.3946383857669));
#11299=CARTESIAN_POINT('Ctrl Pts',(-14.8302213972738,-22.9577053450025,
12.3774516324831));
#11300=CARTESIAN_POINT('Ctrl Pts',(-14.8516165328029,-22.9548823672323,
12.3602702965515));
#11301=CARTESIAN_POINT('Ctrl Pts',(-14.8730816744606,-22.9521283805007,
12.3430942072107));
#11302=CARTESIAN_POINT('Ctrl Pts',(-14.9355475058829,-22.9441139879725,
12.2931099714499));
#11303=CARTESIAN_POINT('Ctrl Pts',(-14.9981564314485,-22.9367118504461,
12.2435306733137));
#11304=CARTESIAN_POINT('Ctrl Pts',(-15.0610456073057,-22.93012990807,12.1943674230766));
#11305=CARTESIAN_POINT('Ctrl Pts',(-15.1217130745985,-22.9237804883426,
12.1469409806861));
#11306=CARTESIAN_POINT('Ctrl Pts',(-15.1826412140633,-22.9181939831412,
12.099901655222));
#11307=CARTESIAN_POINT('Ctrl Pts',(-15.2439503751515,-22.9135965970105,
12.0532836297194));
#11308=CARTESIAN_POINT('Ctrl Pts',(-15.301993125592,-22.9092441490055,12.0091493050565));
#11309=CARTESIAN_POINT('Ctrl Pts',(-15.3603772739025,-22.9057780702211,
11.9653926114926));
#11310=CARTESIAN_POINT('Ctrl Pts',(-15.4192040486566,-22.9034297890288,
11.92206471413));
#11311=CARTESIAN_POINT('Ctrl Pts',(-15.4745612083561,-22.9012200099355,
11.8812923049035));
#11312=CARTESIAN_POINT('Ctrl Pts',(-15.5303102445029,-22.9,11.8408996544229));
#11313=CARTESIAN_POINT('Ctrl Pts',(-15.5865359611318,-22.9,11.8009489759233));
#11314=CARTESIAN_POINT('Origin',(0.,-25.4,0.));
#11315=CARTESIAN_POINT('Ctrl Pts',(-1.69645946028209E-13,-23.936276920587,
-8.326));
#11316=CARTESIAN_POINT('Ctrl Pts',(-0.0274010994650395,-23.9352793807263,
-8.326));
#11317=CARTESIAN_POINT('Ctrl Pts',(-0.0548082522194444,-23.9342787773939,
-8.32586473338683));
#11318=CARTESIAN_POINT('Ctrl Pts',(-1.14031167491963,-23.8945355941156,
-8.31514470485895));
#11319=CARTESIAN_POINT('Ctrl Pts',(-2.18666730607269,-23.8519857556232,
-8.10308607630245));
#11320=CARTESIAN_POINT('Ctrl Pts',(-4.18172956133545,-23.7621201564241,
-7.28308681563853));
#11321=CARTESIAN_POINT('Ctrl Pts',(-5.10558039539358,-23.7155608683631,
-6.66808549943798));
#11322=CARTESIAN_POINT('Ctrl Pts',(-6.64725277062572,-23.6270772146309,
-5.12854094782683));
#11323=CARTESIAN_POINT('Ctrl Pts',(-7.25548788820093,-23.5888585730357,
-4.22441382368631));
#11324=CARTESIAN_POINT('Ctrl Pts',(-8.08933343975371,-23.5055600699609,
-2.24286143339713));
#11325=CARTESIAN_POINT('Ctrl Pts',(-8.31034359466962,-23.4611158669201,
-1.18559733477432));
#11326=CARTESIAN_POINT('Ctrl Pts',(-8.34064497983556,-23.3693592227615,
0.997162148839258));
#11327=CARTESIAN_POINT('Ctrl Pts',(-8.13284787200331,-23.3229214829502,
2.10184963932125));
#11328=CARTESIAN_POINT('Ctrl Pts',(-7.3163309983539,-23.2384100139353,4.1122567565138));
#11329=CARTESIAN_POINT('Ctrl Pts',(-6.7358412207762,-23.2012608476925,5.00678392849045));
#11330=CARTESIAN_POINT('Ctrl Pts',(-5.25329289484859,-23.1148604650577,
6.54961825083766));
#11331=CARTESIAN_POINT('Ctrl Pts',(-4.35797920905201,-23.0690898974778,
7.17652229072915));
#11332=CARTESIAN_POINT('Ctrl Pts',(-2.35933360070256,-22.9777488620224,
8.06051204332207));
#11333=CARTESIAN_POINT('Ctrl Pts',(-1.27209948259276,-22.9330956672779,
8.3018387364197));
#11334=CARTESIAN_POINT('Ctrl Pts',(0.885423436170803,-22.8536280810239,
8.34574012634027));
#11335=CARTESIAN_POINT('Ctrl Pts',(1.93493869722947,-22.812483370607,8.1665258638054));
#11336=CARTESIAN_POINT('Ctrl Pts',(3.94897071169433,-22.7232897406262,7.41135356538661));
#11337=CARTESIAN_POINT('Ctrl Pts',(4.88886987738679,-22.6768113197837,6.82799620615969));
#11338=CARTESIAN_POINT('Ctrl Pts',(6.48385244888632,-22.587375526442,5.33548754082332));
#11339=CARTESIAN_POINT('Ctrl Pts',(7.12517942377867,-22.5480430338092,4.44289902482894));
#11340=CARTESIAN_POINT('Ctrl Pts',(8.01906609183926,-22.4655737864135,2.48107344249377));
#11341=CARTESIAN_POINT('Ctrl Pts',(8.27070775145324,-22.421555858589,1.43394982230191));
#11342=CARTESIAN_POINT('Ctrl Pts',(8.36689005008122,-22.3301593565971,-0.740242393655139));
#11343=CARTESIAN_POINT('Ctrl Pts',(8.19395271794373,-22.2836256801925,-1.84721207863885));
#11344=CARTESIAN_POINT('Ctrl Pts',(7.44127053091648,-22.1980621863545,-3.8826453634813));
#11345=CARTESIAN_POINT('Ctrl Pts',(6.88668076886145,-22.1611398532551,-4.79803083062937));
#11346=CARTESIAN_POINT('Ctrl Pts',(5.4511003404151,-22.0755137687582,-6.38537704461722));
#11347=CARTESIAN_POINT('Ctrl Pts',(4.57822428142744,-22.0300287619124,-7.03755803030118));
#11348=CARTESIAN_POINT('Ctrl Pts',(2.61110659379847,-21.9385536544961,-7.98253450427656));
#11349=CARTESIAN_POINT('Ctrl Pts',(1.53179329320156,-21.8934735716324,-8.25789057277571));
#11350=CARTESIAN_POINT('Ctrl Pts',(0.286737659835875,-21.8467934011162,
-8.32230009878138));
#11351=CARTESIAN_POINT('Ctrl Pts',(0.143308012216421,-21.8414940635969,
-8.326));
#11352=CARTESIAN_POINT('Ctrl Pts',(3.32268934588598E-13,-21.836276920587,
-8.326));
#11353=CARTESIAN_POINT('Ctrl Pts',(-2.01505478969466E-13,-22.2372253046546,
-8.32600000000001));
#11354=CARTESIAN_POINT('Ctrl Pts',(0.926857554021544,-22.2709676497922,
-8.32600000000003));
#11355=CARTESIAN_POINT('Ctrl Pts',(1.84844442910887,-22.3077708387169,-8.17124471417512));
#11356=CARTESIAN_POINT('Ctrl Pts',(3.75781019274245,-22.3911906936277,-7.50948487280907));
#11357=CARTESIAN_POINT('Ctrl Pts',(4.7087912106428,-22.437512891261,-6.95275449859051));
#11358=CARTESIAN_POINT('Ctrl Pts',(6.31349671328978,-22.5258529063643,-5.52922044179108));
#11359=CARTESIAN_POINT('Ctrl Pts',(6.96175792246993,-22.5652067461283,-4.68679005226099));
#11360=CARTESIAN_POINT('Ctrl Pts',(7.93204417654554,-22.6461706110426,-2.76077536861622));
#11361=CARTESIAN_POINT('Ctrl Pts',(8.22760832882724,-22.6913177186374,-1.68679017480437));
#11362=CARTESIAN_POINT('Ctrl Pts',(8.38131717801809,-22.7828063553502,0.489593794539997));
#11363=CARTESIAN_POINT('Ctrl Pts',(8.24743933582676,-22.8282395216875,1.57038391718162));
#11364=CARTESIAN_POINT('Ctrl Pts',(7.58017435530881,-22.9137339484021,3.60417419382718));
#11365=CARTESIAN_POINT('Ctrl Pts',(7.05946358391859,-22.950652170909,4.54016153542568));
#11366=CARTESIAN_POINT('Ctrl Pts',(5.66405929039187,-23.0363904243803,6.2024315356574));
#11367=CARTESIAN_POINT('Ctrl Pts',(4.78867770309699,-23.0829359327552,6.9007284517633));
#11368=CARTESIAN_POINT('Ctrl Pts',(2.8535562941473,-23.1742635426255,7.89410659424699));
#11369=CARTESIAN_POINT('Ctrl Pts',(1.81988991642697,-23.2182057915544,8.19439056473317));
#11370=CARTESIAN_POINT('Ctrl Pts',(-0.328193483426126,-23.3005326623219,
8.39067826878061));
#11371=CARTESIAN_POINT('Ctrl Pts',(-1.42300337566758,-23.3400880033768,
8.27565797708005));
#11372=CARTESIAN_POINT('Ctrl Pts',(-3.51053754999324,-23.4296825252423,
7.62872186353711));
#11373=CARTESIAN_POINT('Ctrl Pts',(-4.48229778555067,-23.476142544793,7.1014249769915));
#11374=CARTESIAN_POINT('Ctrl Pts',(-6.13526565951377,-23.56521591143,5.72659302872137));
#11375=CARTESIAN_POINT('Ctrl Pts',(-6.81067217932797,-23.6060752175234,
4.90401607272714));
#11376=CARTESIAN_POINT('Ctrl Pts',(-7.8414195696069,-23.6857577215008,3.00848313525754));
#11377=CARTESIAN_POINT('Ctrl Pts',(-8.17051718871768,-23.7304848812186,
1.9444879015138));
#11378=CARTESIAN_POINT('Ctrl Pts',(-8.39290191134532,-23.8218544804352,
-0.229064335848684));
#11379=CARTESIAN_POINT('Ctrl Pts',(-8.29212825200708,-23.8675805364092,
-1.31682188453286));
#11380=CARTESIAN_POINT('Ctrl Pts',(-7.6869662415816,-23.9538538822449,-3.36914153432897));
#11381=CARTESIAN_POINT('Ctrl Pts',(-7.1974269872857,-23.9909416216189,-4.3171209688485));
#11382=CARTESIAN_POINT('Ctrl Pts',(-5.85575574791044,-24.0756285643245,
-6.02244098643312));
#11383=CARTESIAN_POINT('Ctrl Pts',(-4.99970398980033,-24.122085170087,-6.74998841649908));
#11384=CARTESIAN_POINT('Ctrl Pts',(-3.08989128939176,-24.2137880707544,
-7.80505779191651));
#11385=CARTESIAN_POINT('Ctrl Pts',(-2.06262619271256,-24.2581645704731,
-8.13708951824372));
#11386=CARTESIAN_POINT('Ctrl Pts',(-0.667929305579545,-24.3124874043931,
-8.30592887838815));
#11387=CARTESIAN_POINT('Ctrl Pts',(-0.333789202319721,-24.3250736742137,
-8.326));
#11388=CARTESIAN_POINT('Ctrl Pts',(-1.72639680329212E-13,-24.3372253046546,
-8.32600000000001));
#11389=CARTESIAN_POINT('Origin',(8.05147737193781,-7.025,-39.3455678841871));
#11390=CARTESIAN_POINT('',(6.45147737193779,-7.025,-36.5742865920769));
#11391=CARTESIAN_POINT('Origin',(8.05147737193781,-7.025,-39.3455678841871));
#11392=CARTESIAN_POINT('',(28.4485226280625,-7.025,-23.8742865920768));
#11393=CARTESIAN_POINT('',(6.4514773719378,-7.025,-36.5742865920769));
#11394=CARTESIAN_POINT('Origin',(30.0485226280625,-7.025,-26.645567884187));
#11395=CARTESIAN_POINT('Origin',(30.0485226280621,-7.025,26.6455678841874));
#11396=CARTESIAN_POINT('',(28.4485226280621,-7.025,23.8742865920772));
#11397=CARTESIAN_POINT('Origin',(30.0485226280621,-7.025,26.6455678841874));
#11398=CARTESIAN_POINT('',(6.45147737193728,-7.025,36.574286592077));
#11399=CARTESIAN_POINT('',(28.4485226280621,-7.025,23.8742865920772));
#11400=CARTESIAN_POINT('Origin',(8.05147737193726,-7.025,39.3455678841872));
#11401=CARTESIAN_POINT('Origin',(-38.1,-7.025,12.7));
#11402=CARTESIAN_POINT('',(-34.9,-7.025,12.7));
#11403=CARTESIAN_POINT('Origin',(-38.1,-7.025,12.7));
#11404=CARTESIAN_POINT('',(-34.9,-7.025,-12.7));
#11405=CARTESIAN_POINT('',(-34.9,-7.025,12.7));
#11406=CARTESIAN_POINT('Origin',(-38.1,-7.025,-12.7));
#11407=CARTESIAN_POINT('Origin',(0.,25.4,0.));
#11408=CARTESIAN_POINT('',(-2.33295215237571E-15,25.4,19.05));
#11409=CARTESIAN_POINT('',(-6.07314264709777,13.15,18.0560083736135));
#11410=CARTESIAN_POINT('',(-6.07314264709777,25.4,18.0560083736135));
#11411=CARTESIAN_POINT('',(-2.33295215237571E-15,13.15,19.05));
#11412=CARTESIAN_POINT('Origin',(0.,13.15,0.));
#11413=CARTESIAN_POINT('',(-2.33295215237571E-15,25.4,19.05));
#11414=CARTESIAN_POINT('',(18.6735332660427,13.15,3.76850837361377));
#11415=CARTESIAN_POINT('Origin',(0.,13.15,0.));
#11416=CARTESIAN_POINT('',(18.6735332660427,25.4,3.76850837361377));
#11417=CARTESIAN_POINT('',(-6.07314264709753,-23.4,-18.0560083736136));
#11418=CARTESIAN_POINT('',(-6.07314264709754,25.4,-18.0560083736136));
#11419=CARTESIAN_POINT('',(18.6735332660427,-23.4,-3.76850837361349));
#11420=CARTESIAN_POINT('Origin',(0.,-23.4,0.));
#11421=CARTESIAN_POINT('',(18.6735332660427,25.4,-3.76850837361349));
#11422=CARTESIAN_POINT('',(-12.6003906189451,13.15,14.2875));
#11423=CARTESIAN_POINT('',(-12.6003906189451,25.4,14.2875));
#11424=CARTESIAN_POINT('',(-12.6003906189451,13.15,-14.2875));
#11425=CARTESIAN_POINT('',(-12.6003906189451,25.4,-14.2875));
#11426=CARTESIAN_POINT('Origin',(0.,13.15,0.));
#11427=CARTESIAN_POINT('Origin',(0.,25.4,0.));
#11428=CARTESIAN_POINT('',(-9.525,25.4,5.49926131403119));
#11429=CARTESIAN_POINT('',(-1.73472347597681E-15,25.4,10.9985226280624));
#11430=CARTESIAN_POINT('Origin',(0.,25.4,0.));
#11431=CARTESIAN_POINT('',(9.525,25.4,5.49926131403118));
#11432=CARTESIAN_POINT('Origin',(0.,25.4,0.));
#11433=CARTESIAN_POINT('',(9.525,25.4,-5.49926131403119));
#11434=CARTESIAN_POINT('Origin',(0.,25.4,0.));
#11435=CARTESIAN_POINT('',(0.,25.4,-10.9985226280624));
#11436=CARTESIAN_POINT('Origin',(0.,25.4,0.));
#11437=CARTESIAN_POINT('',(-9.525,25.4,-5.49926131403119));
#11438=CARTESIAN_POINT('Origin',(0.,25.4,0.));
#11439=CARTESIAN_POINT('Origin',(0.,25.4,0.));
#11440=CARTESIAN_POINT('Origin',(-6.35,15.4,10.9985226280624));
#11441=CARTESIAN_POINT('',(-5.19529946162075,24.727212412536,10.9985226280624));
#11442=CARTESIAN_POINT('',(-5.19529946162075,16.4,10.9985226280624));
#11443=CARTESIAN_POINT('',(-5.19529946162075,15.4,10.9985226280624));
#11444=CARTESIAN_POINT('',(5.19529946162075,16.4,10.9985226280624));
#11445=CARTESIAN_POINT('',(5.19529946162075,16.4,10.9985226280624));
#11446=CARTESIAN_POINT('',(5.19529946162075,24.727212412536,10.9985226280624));
#11447=CARTESIAN_POINT('',(5.19529946162075,15.4,10.9985226280624));
#11448=CARTESIAN_POINT('Ctrl Pts',(5.19529946162091,24.7272124125359,10.9985226280624));
#11449=CARTESIAN_POINT('Ctrl Pts',(2.46696145927109,25.4,10.9985226280624));
#11450=CARTESIAN_POINT('Ctrl Pts',(-5.96292472080612E-15,25.4,10.9985226280624));
#11451=CARTESIAN_POINT('Ctrl Pts',(-5.96292472080612E-15,25.4,10.9985226280624));
#11452=CARTESIAN_POINT('Ctrl Pts',(-2.4669614592711,25.4,10.9985226280624));
#11453=CARTESIAN_POINT('Ctrl Pts',(-5.19529946162091,24.7272124125359,10.9985226280624));
#11454=CARTESIAN_POINT('Origin',(-12.7,15.4,3.66198162423638E-16));
#11455=CARTESIAN_POINT('',(-12.1226497308104,24.727212412536,0.999999999999998));
#11456=CARTESIAN_POINT('',(-12.1226497308104,16.4,0.999999999999999));
#11457=CARTESIAN_POINT('',(-12.1226497308104,15.4,0.999999999999999));
#11458=CARTESIAN_POINT('',(-6.92735026918963,16.4,9.99852262806237));
#11459=CARTESIAN_POINT('',(-6.92735026918962,16.4,9.99852262806237));
#11460=CARTESIAN_POINT('',(-6.92735026918963,24.727212412536,9.99852262806237));
#11461=CARTESIAN_POINT('',(-6.92735026918963,15.4,9.99852262806237));
#11462=CARTESIAN_POINT('Ctrl Pts',(-6.92735026918955,24.7272124125359,9.99852262806251));
#11463=CARTESIAN_POINT('Ctrl Pts',(-8.29151927036445,25.4,7.63571260791709));
#11464=CARTESIAN_POINT('Ctrl Pts',(-9.525,25.4,5.4992613140312));
#11465=CARTESIAN_POINT('Ctrl Pts',(-9.525,25.4,5.4992613140312));
#11466=CARTESIAN_POINT('Ctrl Pts',(-10.7584807296355,25.4,3.36281002014529));
#11467=CARTESIAN_POINT('Ctrl Pts',(-12.1226497308105,24.7272124125359,0.999999999999857));
#11468=CARTESIAN_POINT('Origin',(-6.35,15.4,-10.9985226280624));
#11469=CARTESIAN_POINT('',(-6.92735026918963,24.727212412536,-9.99852262806237));
#11470=CARTESIAN_POINT('',(-6.92735026918963,16.4,-9.99852262806237));
#11471=CARTESIAN_POINT('',(-6.92735026918963,15.4,-9.99852262806237));
#11472=CARTESIAN_POINT('',(-12.1226497308104,16.4,-1.));
#11473=CARTESIAN_POINT('',(-12.1226497308104,16.4,-0.999999999999998));
#11474=CARTESIAN_POINT('',(-12.1226497308104,24.727212412536,-1.));
#11475=CARTESIAN_POINT('',(-12.1226497308104,15.4,-1.));
#11476=CARTESIAN_POINT('Ctrl Pts',(-12.1226497308105,24.7272124125359,-0.99999999999986));
#11477=CARTESIAN_POINT('Ctrl Pts',(-10.7584807296355,25.4,-3.36281002014529));
#11478=CARTESIAN_POINT('Ctrl Pts',(-9.525,25.4,-5.4992613140312));
#11479=CARTESIAN_POINT('Ctrl Pts',(-9.525,25.4,-5.4992613140312));
#11480=CARTESIAN_POINT('Ctrl Pts',(-8.29151927036445,25.4,-7.63571260791709));
#11481=CARTESIAN_POINT('Ctrl Pts',(-6.92735026918955,24.7272124125359,-9.9985226280625));
#11482=CARTESIAN_POINT('Origin',(6.35,15.4,-10.9985226280624));
#11483=CARTESIAN_POINT('',(5.19529946162075,24.727212412536,-10.9985226280624));
#11484=CARTESIAN_POINT('',(5.19529946162075,16.4,-10.9985226280624));
#11485=CARTESIAN_POINT('',(5.19529946162075,15.4,-10.9985226280624));
#11486=CARTESIAN_POINT('',(-5.19529946162075,16.4,-10.9985226280624));
#11487=CARTESIAN_POINT('',(-5.19529946162075,16.4,-10.9985226280624));
#11488=CARTESIAN_POINT('',(-5.19529946162075,24.727212412536,-10.9985226280624));
#11489=CARTESIAN_POINT('',(-5.19529946162075,15.4,-10.9985226280624));
#11490=CARTESIAN_POINT('Ctrl Pts',(-5.19529946162091,24.7272124125359,-10.9985226280624));
#11491=CARTESIAN_POINT('Ctrl Pts',(-2.4669614592711,25.4,-10.9985226280624));
#11492=CARTESIAN_POINT('Ctrl Pts',(-5.96292472080612E-15,25.4,-10.9985226280624));
#11493=CARTESIAN_POINT('Ctrl Pts',(-5.96292472080612E-15,25.4,-10.9985226280624));
#11494=CARTESIAN_POINT('Ctrl Pts',(2.4669614592711,25.4,-10.9985226280624));
#11495=CARTESIAN_POINT('Ctrl Pts',(5.19529946162093,24.7272124125359,-10.9985226280624));
#11496=CARTESIAN_POINT('Origin',(12.7,15.4,-6.93499540769888E-15));
#11497=CARTESIAN_POINT('',(12.1226497308104,24.727212412536,-1.));
#11498=CARTESIAN_POINT('',(12.1226497308104,16.4,-1.00000000000001));
#11499=CARTESIAN_POINT('',(12.1226497308104,15.4,-1.00000000000001));
#11500=CARTESIAN_POINT('',(6.92735026918963,16.4,-9.99852262806237));
#11501=CARTESIAN_POINT('',(6.92735026918962,16.4,-9.99852262806237));
#11502=CARTESIAN_POINT('',(6.92735026918963,24.727212412536,-9.99852262806237));
#11503=CARTESIAN_POINT('',(6.92735026918963,15.4,-9.99852262806237));
#11504=CARTESIAN_POINT('Ctrl Pts',(6.92735026918955,24.7272124125359,-9.99852262806251));
#11505=CARTESIAN_POINT('Ctrl Pts',(8.29151927036445,25.4,-7.6357126079171));
#11506=CARTESIAN_POINT('Ctrl Pts',(9.52499999999999,25.4,-5.49926131403121));
#11507=CARTESIAN_POINT('Ctrl Pts',(9.52499999999999,25.4,-5.49926131403121));
#11508=CARTESIAN_POINT('Ctrl Pts',(10.7584807296355,25.4,-3.36281002014531));
#11509=CARTESIAN_POINT('Ctrl Pts',(12.1226497308104,24.7272124125359,-0.999999999999882));
#11510=CARTESIAN_POINT('Origin',(6.35,15.4,10.9985226280624));
#11511=CARTESIAN_POINT('',(6.92735026918962,24.727212412536,9.99852262806237));
#11512=CARTESIAN_POINT('',(6.92735026918962,16.4,9.99852262806237));
#11513=CARTESIAN_POINT('',(6.92735026918962,15.4,9.99852262806237));
#11514=CARTESIAN_POINT('',(12.1226497308104,16.4,0.999999999999996));
#11515=CARTESIAN_POINT('',(12.1226497308104,16.4,0.999999999999996));
#11516=CARTESIAN_POINT('',(12.1226497308104,24.727212412536,0.999999999999994));
#11517=CARTESIAN_POINT('',(12.1226497308104,15.4,0.999999999999996));
#11518=CARTESIAN_POINT('Ctrl Pts',(12.1226497308105,24.7272124125359,0.999999999999861));
#11519=CARTESIAN_POINT('Ctrl Pts',(10.7584807296355,25.4,3.36281002014528));
#11520=CARTESIAN_POINT('Ctrl Pts',(9.525,25.4,5.49926131403118));
#11521=CARTESIAN_POINT('Ctrl Pts',(9.525,25.4,5.49926131403118));
#11522=CARTESIAN_POINT('Ctrl Pts',(8.29151927036445,25.4,7.63571260791708));
#11523=CARTESIAN_POINT('Ctrl Pts',(6.92735026918955,24.7272124125359,9.9985226280625));
#11524=CARTESIAN_POINT('Origin',(0.,-25.4,0.));
#11525=CARTESIAN_POINT('',(5.8718173029053,-25.4,-8.00113003034161));
#11526=CARTESIAN_POINT('',(6.22809017016564,-25.4,6.25373239212283));
#11527=CARTESIAN_POINT('Ctrl Pts',(5.87181730290515,-25.4,-8.00113003034174));
#11528=CARTESIAN_POINT('Ctrl Pts',(6.41997597897823,-25.4,-7.53910516553241));
#11529=CARTESIAN_POINT('Ctrl Pts',(6.91671183935199,-25.4,-7.01935260004522));
#11530=CARTESIAN_POINT('Ctrl Pts',(7.8176532996952,-25.4,-5.84670254590401));
#11531=CARTESIAN_POINT('Ctrl Pts',(8.21489293449085,-25.3999999996063,-5.18646211216675));
#11532=CARTESIAN_POINT('Ctrl Pts',(9.03044928377891,-25.3999999996063,-3.37939524432784));
#11533=CARTESIAN_POINT('Ctrl Pts',(9.30940044368467,-25.4,-2.17127523394385));
#11534=CARTESIAN_POINT('Ctrl Pts',(9.38117787326285,-25.4,0.257055530030207));
#11535=CARTESIAN_POINT('Ctrl Pts',(9.1837385826432,-25.4,1.45330461325936));
#11536=CARTESIAN_POINT('Ctrl Pts',(8.43719385355252,-25.4,3.45684341944329));
#11537=CARTESIAN_POINT('Ctrl Pts',(8.03460625325573,-25.4,4.1345974411627));
#11538=CARTESIAN_POINT('Ctrl Pts',(7.28968847710234,-25.4,5.21524977190067));
#11539=CARTESIAN_POINT('Ctrl Pts',(6.7912859412746,-25.4,5.76979234178763));
#11540=CARTESIAN_POINT('Ctrl Pts',(6.22809017016566,-25.4,6.25373239212283));
#11541=CARTESIAN_POINT('',(-7.7648517191704,-25.4,-4.1958734226972));
#11542=CARTESIAN_POINT('Ctrl Pts',(-7.76485171917045,-25.4,-4.19587342269709));
#11543=CARTESIAN_POINT('Ctrl Pts',(-7.5153669902019,-25.4,-4.74202422930472));
#11544=CARTESIAN_POINT('Ctrl Pts',(-7.11824932711354,-25.4,-5.46216308143309));
#11545=CARTESIAN_POINT('Ctrl Pts',(-6.02425805366761,-25.4,-6.78618608402815));
#11546=CARTESIAN_POINT('Ctrl Pts',(-5.47681493420003,-25.4,-7.30383758510192));
#11547=CARTESIAN_POINT('Ctrl Pts',(-3.95926137314159,-25.4,-8.42099215986769));
#11548=CARTESIAN_POINT('Ctrl Pts',(-2.92934762161546,-25.4000000000001,
-8.91762230918457));
#11549=CARTESIAN_POINT('Ctrl Pts',(-0.398296561048911,-25.4000000000001,
-9.60246458995361));
#11550=CARTESIAN_POINT('Ctrl Pts',(0.902188672117903,-25.4,-9.57961545600489));
#11551=CARTESIAN_POINT('Ctrl Pts',(2.60403764477334,-25.4,-9.3536353399083));
#11552=CARTESIAN_POINT('Ctrl Pts',(3.2999578043234,-25.4,-9.18265881085097));
#11553=CARTESIAN_POINT('Ctrl Pts',(4.63664497571866,-25.4,-8.69493921576204));
#11554=CARTESIAN_POINT('Ctrl Pts',(5.27387123787004,-25.4,-8.38091270986061));
#11555=CARTESIAN_POINT('Ctrl Pts',(5.87181730290536,-25.4,-8.00113003034165));
#11556=CARTESIAN_POINT('Origin',(0.,-25.4,0.));
#11557=CARTESIAN_POINT('Origin',(0.,-25.4,0.));
#11558=CARTESIAN_POINT('',(8.29083424217445,-24.9756402675196,1.3600098358447));
#11559=CARTESIAN_POINT('Ctrl Pts',(8.27736571547514,-24.8999999999998,0.898606038414263));
#11560=CARTESIAN_POINT('Ctrl Pts',(8.27792777712598,-24.9005058876881,0.898115980561187));
#11561=CARTESIAN_POINT('Ctrl Pts',(8.27851833941179,-24.9010467821481,0.897687233867645));
#11562=CARTESIAN_POINT('Ctrl Pts',(8.27968811062583,-24.9021422632964,0.897061021095975));
#11563=CARTESIAN_POINT('Ctrl Pts',(8.28025936483844,-24.9026872898312,0.896848287015314));
#11564=CARTESIAN_POINT('Ctrl Pts',(8.28167137333571,-24.9040642904923,0.896599354755583));
#11565=CARTESIAN_POINT('Ctrl Pts',(8.28247701078594,-24.9048744754402,0.896685085175965));
#11566=CARTESIAN_POINT('Ctrl Pts',(8.28424370644011,-24.9067065626039,0.897387848768569));
#11567=CARTESIAN_POINT('Ctrl Pts',(8.28512484299656,-24.9076604489329,0.898111048931224));
#11568=CARTESIAN_POINT('Ctrl Pts',(8.28727633454631,-24.9100640801295,0.900564978387333));
#11569=CARTESIAN_POINT('Ctrl Pts',(8.28841257360746,-24.9114278355422,0.902731407094527));
#11570=CARTESIAN_POINT('Ctrl Pts',(8.29319510537141,-24.9174019317703,0.913972293170574));
#11571=CARTESIAN_POINT('Ctrl Pts',(8.29589583640989,-24.9217968036879,0.929557055849718));
#11572=CARTESIAN_POINT('Ctrl Pts',(8.30405884437143,-24.9378851382505,1.00000457409689));
#11573=CARTESIAN_POINT('Ctrl Pts',(8.30347691095396,-24.947772881011,1.08337191045941));
#11574=CARTESIAN_POINT('Ctrl Pts',(8.30147063765394,-24.96111035307,1.19797632784268));
#11575=CARTESIAN_POINT('Ctrl Pts',(8.29692634943919,-24.9688790701265,1.28110320078678));
#11576=CARTESIAN_POINT('Ctrl Pts',(8.29083424217439,-24.9756402675196,1.36000983584488));
#11577=CARTESIAN_POINT('Ctrl Pts',(8.29083424217443,-24.9756402675196,1.36000983584492));
#11578=CARTESIAN_POINT('Ctrl Pts',(8.22153300492422,-25.0525527912602,2.25761836423918));
#11579=CARTESIAN_POINT('Ctrl Pts',(8.00586925271954,-25.1258907620308,3.13818145654568));
#11580=CARTESIAN_POINT('Ctrl Pts',(7.35437567063969,-25.2503896474066,4.66543782159151));
#11581=CARTESIAN_POINT('Ctrl Pts',(6.89843763491226,-25.3178303686065,5.47016614476703));
#11582=CARTESIAN_POINT('Ctrl Pts',(6.22809017016576,-25.4,6.25373239212268));
#11583=CARTESIAN_POINT('',(-1.22646583495775,-24.9756402675196,8.31163887211714));
#11584=CARTESIAN_POINT('Ctrl Pts',(-7.76485171917038,-25.4,-4.19587342269725));
#11585=CARTESIAN_POINT('Ctrl Pts',(-8.1625641051082,-25.3799542890918,-3.41770382146533));
#11586=CARTESIAN_POINT('Ctrl Pts',(-8.44096609023593,-25.3583447746017,
-2.58416658384216));
#11587=CARTESIAN_POINT('Ctrl Pts',(-8.73067322640372,-25.3148141240392,
-0.918583409896716));
#11588=CARTESIAN_POINT('Ctrl Pts',(-8.75681063341049,-25.2932206376699,
-0.0982451433149351));
#11589=CARTESIAN_POINT('Ctrl Pts',(-8.55253607540217,-25.2434905757203,
1.7768193962029));
#11590=CARTESIAN_POINT('Ctrl Pts',(-8.24197358540638,-25.2158150895935,
2.80962671360843));
#11591=CARTESIAN_POINT('Ctrl Pts',(-7.49207553268971,-25.1764653617559,
4.26541248529107));
#11592=CARTESIAN_POINT('Ctrl Pts',(-7.18187287266752,-25.1634972947921,
4.7463215114945));
#11593=CARTESIAN_POINT('Ctrl Pts',(-6.17167919809883,-25.1235000651364,
6.0077427917133));
#11594=CARTESIAN_POINT('Ctrl Pts',(-5.3745473042224,-25.0957922580711,6.69504056537595));
#11595=CARTESIAN_POINT('Ctrl Pts',(-3.98322276197756,-25.0521915511955,
7.5056283585964));
#11596=CARTESIAN_POINT('Ctrl Pts',(-3.46631461954251,-25.0367984221239,
7.74108627138892));
#11597=CARTESIAN_POINT('Ctrl Pts',(-2.37691369428902,-25.0059102608247,
8.11098499338516));
#11598=CARTESIAN_POINT('Ctrl Pts',(-1.80610835590355,-24.9905087719593,
8.2411362995407));
#11599=CARTESIAN_POINT('Ctrl Pts',(-1.22646583495779,-24.9756402675196,
8.31163887211713));
#11600=CARTESIAN_POINT('Ctrl Pts',(-1.22646583495773,-24.9756402675196,
8.31163887211714));
#11601=CARTESIAN_POINT('Ctrl Pts',(-0.655124605969128,-24.9609847008681,
8.38113174920447));
#11602=CARTESIAN_POINT('Ctrl Pts',(-0.0736308671996442,-24.9483146439235,
8.39393002745997));
#11603=CARTESIAN_POINT('Ctrl Pts',(1.0776057392628,-24.9235712832695,8.29979327199434));
#11604=CARTESIAN_POINT('Ctrl Pts',(1.64605625058501,-24.911464890879,8.19367679821349));
#11605=CARTESIAN_POINT('Ctrl Pts',(2.19919404320639,-24.9,8.03030644249182));
#11606=CARTESIAN_POINT('Origin',(-48.,-7.90000000000001,12.7));
#11607=CARTESIAN_POINT('',(-48.,-7.90000000000001,12.7));
#11608=CARTESIAN_POINT('',(-48.,-21.9,12.7));
#11609=CARTESIAN_POINT('',(-48.,-7.90000000000001,12.7));
#11610=CARTESIAN_POINT('',(-16.8005208252602,-21.9,12.7));
#11611=CARTESIAN_POINT('',(-48.,-21.9,12.7));
#11612=CARTESIAN_POINT('',(-16.8005208252602,7.75488674445212,12.7));
#11613=CARTESIAN_POINT('',(-16.8005208252602,12.65,12.7));
#11614=CARTESIAN_POINT('',(-17.9697662756086,7.65,12.7));
#11615=CARTESIAN_POINT('Origin',(-24.2765469920838,163.404688042985,12.7));
#11616=CARTESIAN_POINT('',(-34.1050004454305,7.65,12.7));
#11617=CARTESIAN_POINT('',(-48.,7.65,12.7));
#11618=CARTESIAN_POINT('',(-48.,-7.90000000000001,12.7));
#11619=CARTESIAN_POINT('Origin',(-48.,-7.90000000000001,-12.7));
#11620=CARTESIAN_POINT('',(-16.8005208252602,7.75488674445212,-12.7));
#11621=CARTESIAN_POINT('',(-16.8005208252602,-21.9,-12.7));
#11622=CARTESIAN_POINT('',(-16.8005208252602,-7.90000000000001,-12.7));
#11623=CARTESIAN_POINT('',(-48.,-21.9,-12.7));
#11624=CARTESIAN_POINT('',(-48.,-21.9,-12.7));
#11625=CARTESIAN_POINT('',(-48.,-7.90000000000001,-12.7));
#11626=CARTESIAN_POINT('',(-48.,-7.90000000000001,-12.7));
#11627=CARTESIAN_POINT('',(-34.1050004454305,7.65,-12.7));
#11628=CARTESIAN_POINT('',(-33.5086522928671,8.31737776679611,-12.7));
#11629=CARTESIAN_POINT('',(-17.9697662756086,7.65,-12.7));
#11630=CARTESIAN_POINT('',(-16.8005208252602,7.65,-12.7));
#11631=CARTESIAN_POINT('Origin',(-24.2765469720169,163.404687367871,-12.7));
#11632=CARTESIAN_POINT('Origin',(-35.,12.65,12.7));
#11633=CARTESIAN_POINT('',(-35.,12.65,7.7));
#11634=CARTESIAN_POINT('',(-35.,12.65,-7.7));
#11635=CARTESIAN_POINT('',(-35.,12.65,12.7));
#11636=CARTESIAN_POINT('',(-17.9697662756086,12.65,7.7));
#11637=CARTESIAN_POINT('',(-35.,12.65,7.7));
#11638=CARTESIAN_POINT('',(-17.9697662756086,12.65,-7.7));
#11639=CARTESIAN_POINT('Origin',(0.,12.65,0.));
#11640=CARTESIAN_POINT('',(-35.,12.65,-7.7));
#11641=CARTESIAN_POINT('Origin',(-35.,9.65,12.7));
#11642=CARTESIAN_POINT('',(-37.2370215606994,11.6489333498058,7.7));
#11643=CARTESIAN_POINT('',(-37.2370215606994,11.6489333498058,-7.7));
#11644=CARTESIAN_POINT('',(-37.2370215606994,11.6489333498058,12.7));
#11645=CARTESIAN_POINT('Origin',(-35.,9.65,7.7));
#11646=CARTESIAN_POINT('Origin',(-35.,9.65,-7.7));
#11647=CARTESIAN_POINT('Origin',(-51.7283692678324,-4.56844441699029,12.7));
#11648=CARTESIAN_POINT('',(-51.7283692678324,-4.56844441699029,7.7));
#11649=CARTESIAN_POINT('',(-51.7283692678324,-4.56844441699029,-7.7));
#11650=CARTESIAN_POINT('',(-51.7283692678324,-4.56844441699029,12.7));
#11651=CARTESIAN_POINT('',(-51.7283692678324,-4.56844441699029,7.7));
#11652=CARTESIAN_POINT('',(-51.7283692678324,-4.56844441699029,-7.7));
#11653=CARTESIAN_POINT('Origin',(-48.,-7.90000000000001,12.7));
#11654=CARTESIAN_POINT('',(-53.,-7.90000000000001,7.7));
#11655=CARTESIAN_POINT('',(-53.,-7.90000000000001,-7.7));
#11656=CARTESIAN_POINT('',(-53.,-7.90000000000001,12.7));
#11657=CARTESIAN_POINT('Origin',(-48.,-7.90000000000001,7.7));
#11658=CARTESIAN_POINT('Origin',(-48.,-7.90000000000001,-7.7));
#11659=CARTESIAN_POINT('Origin',(-53.,-22.9,12.7));
#11660=CARTESIAN_POINT('',(-53.,-21.9,-7.7));
#11661=CARTESIAN_POINT('',(-53.,-22.9,-7.7));
#11662=CARTESIAN_POINT('',(-53.,-21.9,7.7));
#11663=CARTESIAN_POINT('',(-53.,-21.9,12.7));
#11664=CARTESIAN_POINT('',(-53.,-22.9,7.7));
#11665=CARTESIAN_POINT('Origin',(4.35361937096884E-15,-22.9,12.7));
#11666=CARTESIAN_POINT('',(-16.8005208252602,-22.9,11.7));
#11667=CARTESIAN_POINT('Origin',(-16.8005208252602,-22.9,19.05));
#11668=CARTESIAN_POINT('',(-48.,-22.9,11.7));
#11669=CARTESIAN_POINT('',(4.35361937096884E-15,-22.9,11.7));
#11670=CARTESIAN_POINT('',(-52.,-22.9,7.7));
#11671=CARTESIAN_POINT('Origin',(-48.,-22.9,7.7));
#11672=CARTESIAN_POINT('',(-52.,-22.9,-7.7));
#11673=CARTESIAN_POINT('',(-52.,-22.9,12.7));
#11674=CARTESIAN_POINT('',(-48.,-22.9,-11.7));
#11675=CARTESIAN_POINT('Origin',(-48.,-22.9,-7.7));
#11676=CARTESIAN_POINT('',(-16.8005208252602,-22.9,-11.7));
#11677=CARTESIAN_POINT('',(-16.8005208252602,-22.9,-11.7));
#11678=CARTESIAN_POINT('Origin',(-16.8005208252602,-22.9,-19.05));
#11679=CARTESIAN_POINT('Origin',(34.998522628062,-7.90000000000001,35.2192193816534));
#11680=CARTESIAN_POINT('',(34.998522628062,-7.9,35.2192193816534));
#11681=CARTESIAN_POINT('',(34.998522628062,-21.9,35.2192193816534));
#11682=CARTESIAN_POINT('',(34.998522628062,-7.90000000000001,35.2192193816534));
#11683=CARTESIAN_POINT('',(19.3987830406924,-21.9,8.19967783148497));
#11684=CARTESIAN_POINT('',(34.998522628062,-21.9,35.2192193816534));
#11685=CARTESIAN_POINT('',(19.3987830406924,7.75488674445212,8.19967783148497));
#11686=CARTESIAN_POINT('',(19.3987830406924,12.65,8.19967783148497));
#11687=CARTESIAN_POINT('',(19.9834057658666,7.65,9.21227409474611));
#11688=CARTESIAN_POINT('Origin',(23.1367961164486,163.404687557813,14.6741063980318));
#11689=CARTESIAN_POINT('',(28.0510228507774,7.65,23.1857967818227));
#11690=CARTESIAN_POINT('',(34.998522628062,7.65,35.2192193816534));
#11691=CARTESIAN_POINT('',(34.998522628062,-7.9,35.2192193816534));
#11692=CARTESIAN_POINT('Origin',(28.4985226280621,12.65,23.9608891324556));
#11693=CARTESIAN_POINT('',(24.1683956091399,12.65,26.4608891324556));
#11694=CARTESIAN_POINT('',(10.8316043908595,12.65,34.1608891324555));
#11695=CARTESIAN_POINT('',(28.4985226280621,12.65,23.9608891324556));
#11696=CARTESIAN_POINT('',(15.6532787469444,12.65,11.7122740947461));
#11697=CARTESIAN_POINT('',(24.1683956091399,12.65,26.4608891324556));
#11698=CARTESIAN_POINT('',(2.31648752866395,12.65,19.4122740947459));
#11699=CARTESIAN_POINT('Origin',(0.,12.65,0.));
#11700=CARTESIAN_POINT('',(10.8316043908595,12.65,34.1608891324555));
#11701=CARTESIAN_POINT('Origin',(28.4985226280621,9.65,23.9608891324556));
#11702=CARTESIAN_POINT('Origin',(10.8316043908595,9.65,34.1608891324555));
#11703=CARTESIAN_POINT('',(25.2869063894896,11.6489333498058,28.3982066328348));
#11704=CARTESIAN_POINT('',(29.6170334084118,11.6489333498058,25.8982066328348));
#11705=CARTESIAN_POINT('Origin',(24.1683956091399,9.65,26.4608891324556));
#11706=CARTESIAN_POINT('Origin',(36.8627072619782,-4.56844441699029,38.4480818822854));
#11707=CARTESIAN_POINT('',(32.532580243056,-4.56844441699029,40.9480818822854));
#11708=CARTESIAN_POINT('',(36.8627072619782,-4.56844441699029,38.4480818822854));
#11709=CARTESIAN_POINT('',(32.532580243056,-4.56844441699029,40.9480818822854));
#11710=CARTESIAN_POINT('Origin',(34.998522628062,-7.90000000000001,35.2192193816534));
#11711=CARTESIAN_POINT('Origin',(17.3316043908594,-7.90000000000001,45.4192193816532));
#11712=CARTESIAN_POINT('',(33.1683956091398,-7.90000000000001,42.0493464005755));
#11713=CARTESIAN_POINT('',(37.498522628062,-7.90000000000001,39.5493464005756));
#11714=CARTESIAN_POINT('Origin',(30.6683956091398,-7.90000000000001,37.7192193816533));
#11715=CARTESIAN_POINT('Origin',(37.498522628062,-22.9,39.5493464005756));
#11716=CARTESIAN_POINT('',(33.1683956091398,-21.9,42.0493464005755));
#11717=CARTESIAN_POINT('',(37.498522628062,-21.9,39.5493464005756));
#11718=CARTESIAN_POINT('',(33.1683956091398,-22.9,42.0493464005755));
#11719=CARTESIAN_POINT('Origin',(10.9985226280624,-22.9,-6.3499999999999));
#11720=CARTESIAN_POINT('',(18.5327576369079,-22.9,8.69967783148497));
#11721=CARTESIAN_POINT('Origin',(24.8980443547236,-22.9,5.02467783148503));
#11722=CARTESIAN_POINT('',(34.1324972242776,-22.9,35.7192193816534));
#11723=CARTESIAN_POINT('',(10.132497224278,-22.9,-5.84999999999991));
#11724=CARTESIAN_POINT('',(32.6683956091398,-22.9,41.1833209967911));
#11725=CARTESIAN_POINT('Origin',(30.6683956091398,-22.9,37.7192193816533));
#11726=CARTESIAN_POINT('',(36.998522628062,-22.9,38.6833209967911));
#11727=CARTESIAN_POINT('',(-1.73223681164803,-22.9,20.3996778314848));
#11728=CARTESIAN_POINT('',(-1.73223681164803,-22.9,20.3996778314848));
#11729=CARTESIAN_POINT('Origin',(-8.09752352946369,-22.9,24.0746778314847));
#11730=CARTESIAN_POINT('Origin',(13.0014773719372,-7.90000000000001,47.9192193816532));
#11731=CARTESIAN_POINT('',(-2.59826221543248,7.75488674445211,20.8996778314848));
#11732=CARTESIAN_POINT('',(-2.59826221543248,-21.9,20.8996778314848));
#11733=CARTESIAN_POINT('',(-2.59826221543248,-7.90000000000001,20.8996778314848));
#11734=CARTESIAN_POINT('',(13.0014773719372,-21.9,47.9192193816532));
#11735=CARTESIAN_POINT('',(-2.01363949025827,7.65,21.9122740947459));
#11736=CARTESIAN_POINT('',(-2.59826221543248,7.65,20.8996778314848));
#11737=CARTESIAN_POINT('Origin',(1.13975086201663,163.404687845728,27.3741064009758));
#11738=CARTESIAN_POINT('Origin',(13.0014773719379,-7.90000000000001,-47.919219381653));
#11739=CARTESIAN_POINT('',(-2.5982622154322,-21.9,-20.8996778314848));
#11740=CARTESIAN_POINT('',(13.0014773719379,-21.9,-47.919219381653));
#11741=CARTESIAN_POINT('',(-2.5982622154322,7.75488674445212,-20.8996778314848));
#11742=CARTESIAN_POINT('',(-2.5982622154322,12.65,-20.8996778314848));
#11743=CARTESIAN_POINT('',(-2.01363949025797,7.65,-21.9122740947459));
#11744=CARTESIAN_POINT('Origin',(1.13975086881472,163.404688086806,-27.3741064127498));
#11745=CARTESIAN_POINT('',(13.0014773719379,7.65,-47.919219381653));
#11746=CARTESIAN_POINT('Origin',(6.5014773719378,12.65,-36.6608891324553));
#11747=CARTESIAN_POINT('',(10.83160439086,12.65,-34.1608891324553));
#11748=CARTESIAN_POINT('',(24.1683956091403,12.65,-26.4608891324553));
#11749=CARTESIAN_POINT('',(6.5014773719378,12.65,-36.6608891324553));
#11750=CARTESIAN_POINT('',(10.83160439086,12.65,-34.1608891324553));
#11751=CARTESIAN_POINT('',(24.1683956091403,12.65,-26.4608891324553));
#11752=CARTESIAN_POINT('Origin',(6.5014773719378,9.65,-36.6608891324553));
#11753=CARTESIAN_POINT('',(25.28690638949,11.6489333498058,-28.3982066328344));
#11754=CARTESIAN_POINT('Origin',(24.1683956091403,9.65,-26.4608891324553));
#11755=CARTESIAN_POINT('',(7.61998815228752,11.6489333498058,-38.5982066328345));
#11756=CARTESIAN_POINT('Origin',(10.83160439086,9.65,-34.1608891324553));
#11757=CARTESIAN_POINT('Origin',(14.8656620058541,-4.56844441699029,-51.148081882285));
#11758=CARTESIAN_POINT('',(32.5325802430566,-4.56844441699029,-40.9480818822849));
#11759=CARTESIAN_POINT('',(32.5325802430566,-4.56844441699029,-40.9480818822849));
#11760=CARTESIAN_POINT('',(14.865662005854,-4.56844441699029,-51.148081882285));
#11761=CARTESIAN_POINT('Origin',(13.0014773719379,-7.90000000000001,-47.919219381653));
#11762=CARTESIAN_POINT('',(33.1683956091404,-7.90000000000001,-42.0493464005751));
#11763=CARTESIAN_POINT('Origin',(30.6683956091404,-7.90000000000001,-37.7192193816529));
#11764=CARTESIAN_POINT('',(15.5014773719379,-7.90000000000001,-52.2493464005752));
#11765=CARTESIAN_POINT('Origin',(17.33160439086,-7.90000000000001,-45.419219381653));
#11766=CARTESIAN_POINT('Origin',(15.5014773719379,-22.9,-52.2493464005752));
#11767=CARTESIAN_POINT('',(33.1683956091404,-21.9,-42.0493464005751));
#11768=CARTESIAN_POINT('',(33.1683956091404,-22.9,-42.0493464005751));
#11769=CARTESIAN_POINT('',(15.5014773719379,-21.9,-52.2493464005752));
#11770=CARTESIAN_POINT('Origin',(-10.9985226280623,-22.9,-6.35000000000005));
#11771=CARTESIAN_POINT('',(18.0131895824795,-22.9,-7.59786161137808));
#11772=CARTESIAN_POINT('',(-2.42665362134758,-22.9,-19.3988105873015));
#11773=CARTESIAN_POINT('Origin',(4.9095947433306E-17,-22.9,-8.50366754002159E-17));
#11774=CARTESIAN_POINT('',(-1.73223681164776,-22.9,-20.3996778314848));
#11775=CARTESIAN_POINT('Origin',(-8.09752352946338,-22.9,-24.0746778314848));
#11776=CARTESIAN_POINT('',(13.8675027757223,-22.9,-47.419219381653));
#11777=CARTESIAN_POINT('',(-10.1324972242779,-22.9,-5.85000000000004));
#11778=CARTESIAN_POINT('',(19.3316043908601,-22.9,-48.8833209967907));
#11779=CARTESIAN_POINT('Origin',(17.33160439086,-22.9,-45.419219381653));
#11780=CARTESIAN_POINT('',(32.6683956091404,-22.9,-41.1833209967907));
#11781=CARTESIAN_POINT('',(15.0014773719379,-22.9,-51.3833209967907));
#11782=CARTESIAN_POINT('',(34.1324972242781,-22.9,-35.7192193816529));
#11783=CARTESIAN_POINT('Origin',(30.6683956091404,-22.9,-37.7192193816529));
#11784=CARTESIAN_POINT('',(18.532757636908,-22.9,-8.6996778314847));
#11785=CARTESIAN_POINT('',(18.532757636908,-22.9,-8.6996778314847));
#11786=CARTESIAN_POINT('Origin',(24.8980443547237,-22.9,-5.02467783148466));
#11787=CARTESIAN_POINT('Origin',(34.9985226280625,-7.90000000000001,-35.2192193816529));
#11788=CARTESIAN_POINT('',(19.3987830406925,7.75488674445212,-8.19967783148469));
#11789=CARTESIAN_POINT('',(19.3987830406925,-21.9,-8.19967783148469));
#11790=CARTESIAN_POINT('',(19.3987830406925,-7.90000000000001,-8.19967783148469));
#11791=CARTESIAN_POINT('',(34.9985226280625,-21.9,-35.2192193816529));
#11792=CARTESIAN_POINT('',(34.9985226280625,-21.9,-35.2192193816529));
#11793=CARTESIAN_POINT('',(34.9985226280625,-7.90000000000001,-35.2192193816529));
#11794=CARTESIAN_POINT('',(34.9985226280625,-7.90000000000001,-35.2192193816529));
#11795=CARTESIAN_POINT('',(28.0510228507777,7.65,-23.1857967818223));
#11796=CARTESIAN_POINT('',(27.752848774496,8.31737776679612,-22.6693441322024));
#11797=CARTESIAN_POINT('',(19.9834057658667,7.65,-9.21227409474582));
#11798=CARTESIAN_POINT('',(19.3987830406925,7.65,-8.19967783148468));
#11799=CARTESIAN_POINT('Origin',(23.136796101799,163.404686601979,-14.6741063726841));
#11800=CARTESIAN_POINT('Origin',(-16.8005208252602,25.4,-19.05));
#11801=CARTESIAN_POINT('',(-15.7517039698567,-21.9,-12.7872144213759));
#11802=CARTESIAN_POINT('Ctrl Pts',(-12.6003906189451,-23.4,-14.2875));
#11803=CARTESIAN_POINT('Ctrl Pts',(-12.7170023297541,-23.3035563482058,
-14.1846581377472));
#11804=CARTESIAN_POINT('Ctrl Pts',(-12.8375066038114,-23.2068396386061,
-14.0859034998214));
#11805=CARTESIAN_POINT('Ctrl Pts',(-12.9620390251358,-23.1112816986106,
-13.9913525639123));
#11806=CARTESIAN_POINT('Ctrl Pts',(-13.0797099390072,-23.0209888254186,
-13.902011210733));
#11807=CARTESIAN_POINT('Ctrl Pts',(-13.2009776026165,-22.931728890007,-13.8164231666886));
#11808=CARTESIAN_POINT('Ctrl Pts',(-13.3259828864208,-22.8447237861406,
-13.7347186102794));
#11809=CARTESIAN_POINT('Ctrl Pts',(-13.4398977695664,-22.7654377276767,
-13.6602628375907));
#11810=CARTESIAN_POINT('Ctrl Pts',(-13.5569167566412,-22.6880233923778,
-13.5890322851068));
#11811=CARTESIAN_POINT('Ctrl Pts',(-13.6771653733519,-22.613433061264,-13.5211502011406));
#11812=CARTESIAN_POINT('Ctrl Pts',(-13.780395816837,-22.5493991191596,-13.46287512219));
#11813=CARTESIAN_POINT('Ctrl Pts',(-13.8860066956812,-22.4874464632126,
-13.4070681378658));
#11814=CARTESIAN_POINT('Ctrl Pts',(-13.994088488402,-22.428202217372,-13.3538221960299));
#11815=CARTESIAN_POINT('Ctrl Pts',(-13.9996382379135,-22.4251601626824,
-13.3510881403462));
#11816=CARTESIAN_POINT('Ctrl Pts',(-14.0051944007122,-22.4221253454026,
-13.3483608913321));
#11817=CARTESIAN_POINT('Ctrl Pts',(-14.0107569982363,-22.4190978469187,
-13.345640457389));
#11818=CARTESIAN_POINT('Ctrl Pts',(-14.1078577207225,-22.3662498224408,
-13.2981525526451));
#11819=CARTESIAN_POINT('Ctrl Pts',(-14.2071599870361,-22.3154805383895,
-13.2526249539681));
#11820=CARTESIAN_POINT('Ctrl Pts',(-14.3089608526168,-22.2675991945199,
-13.2091881241018));
#11821=CARTESIAN_POINT('Ctrl Pts',(-14.4029294513603,-22.2234017040201,
-13.1690931994357));
#11822=CARTESIAN_POINT('Ctrl Pts',(-14.4990269678438,-22.1816645410303,
-13.1307798082167));
#11823=CARTESIAN_POINT('Ctrl Pts',(-14.5975040224041,-22.1430604940455,
-13.0943671154366));
#11824=CARTESIAN_POINT('Ctrl Pts',(-14.6716472726562,-22.1139955557294,
-13.0669520449392));
#11825=CARTESIAN_POINT('Ctrl Pts',(-14.7471396830704,-22.0867072848311,
-13.0406147104802));
#11826=CARTESIAN_POINT('Ctrl Pts',(-14.8240955566372,-22.0614998943554,
-13.0154125395925));
#11827=CARTESIAN_POINT('Ctrl Pts',(-14.8293099770775,-22.0597918774614,
-13.0137048763704));
#11828=CARTESIAN_POINT('Ctrl Pts',(-14.8345302483747,-22.0580937292925,
-13.0120027124143));
#11829=CARTESIAN_POINT('Ctrl Pts',(-14.8397564046443,-22.056405537151,-13.0103060600109));
#11830=CARTESIAN_POINT('Ctrl Pts',(-14.9357824134385,-22.0253864965673,
-12.9791315695807));
#11831=CARTESIAN_POINT('Ctrl Pts',(-15.032901952619,-21.9978800256288,-12.9500987220667));
#11832=CARTESIAN_POINT('Ctrl Pts',(-15.1313475446627,-21.9749039650076,
-12.9232625229759));
#11833=CARTESIAN_POINT('Ctrl Pts',(-15.2241318069018,-21.9532491931723,
-12.8979695984045));
#11834=CARTESIAN_POINT('Ctrl Pts',(-15.3180939370895,-21.9356181609241,
-12.8746280167693));
#11835=CARTESIAN_POINT('Ctrl Pts',(-15.4134375927924,-21.9229055030944,
-12.8532981171489));
#11836=CARTESIAN_POINT('Ctrl Pts',(-15.5029064118453,-21.9109761673178,
-12.8332825123823));
#11837=CARTESIAN_POINT('Ctrl Pts',(-15.5935917299168,-21.9033774739699,
-12.8150383915244));
#11838=CARTESIAN_POINT('Ctrl Pts',(-15.6856704705524,-21.9008931019107,
-12.7986275193415));
#11839=CARTESIAN_POINT('Ctrl Pts',(-15.7076017238433,-21.9003013758236,
-12.7947187887042));
#11840=CARTESIAN_POINT('Ctrl Pts',(-15.7296120665973,-21.9000000019656,
-12.7909141106301));
#11841=CARTESIAN_POINT('Ctrl Pts',(-15.7517039698567,-21.9,-12.7872144213759));
#11842=CARTESIAN_POINT('Origin',(-16.8005208252602,-21.9,-19.05));
#11843=CARTESIAN_POINT('Ctrl Pts',(-16.8005208252602,7.75488674445212,-12.7));
#11844=CARTESIAN_POINT('Ctrl Pts',(-16.7349414235869,7.77600035063442,-12.7));
#11845=CARTESIAN_POINT('Ctrl Pts',(-16.6708099716639,7.79969631458978,-12.7010053967542));
#11846=CARTESIAN_POINT('Ctrl Pts',(-16.6079679401019,7.8256484538807,-12.7029063991874));
#11847=CARTESIAN_POINT('Ctrl Pts',(-16.5435673523868,7.85224423669134,-12.7048545487126));
#11848=CARTESIAN_POINT('Ctrl Pts',(-16.4805209961261,7.88120973563962,-12.7077433417563));
#11849=CARTESIAN_POINT('Ctrl Pts',(-16.4186711504242,7.91224591462863,-12.711471286032));
#11850=CARTESIAN_POINT('Ctrl Pts',(-16.3543372897761,7.94452856936239,-12.7153489520926));
#11851=CARTESIAN_POINT('Ctrl Pts',(-16.2912980137447,7.97905171373885,-12.7201345556429));
#11852=CARTESIAN_POINT('Ctrl Pts',(-16.2293889115104,8.01553158395874,-12.7257310395034));
#11853=CARTESIAN_POINT('Ctrl Pts',(-16.1958378593221,8.0353015044615,-12.7287640009792));
#11854=CARTESIAN_POINT('Ctrl Pts',(-16.1626189581162,8.05564699923813,-12.7320354070764));
#11855=CARTESIAN_POINT('Ctrl Pts',(-16.1297074857929,8.07652873453458,-12.7355317354578));
#11856=CARTESIAN_POINT('Ctrl Pts',(-16.0866738196167,8.10383281917404,-12.7401033883735));
#11857=CARTESIAN_POINT('Ctrl Pts',(-16.0441679035951,8.13206076164089,-12.7450610080348));
#11858=CARTESIAN_POINT('Ctrl Pts',(-16.002143104575,8.16115913750229,-12.7503845705938));
#11859=CARTESIAN_POINT('Ctrl Pts',(-15.9276085615548,8.21276757342653,-12.7598263600091));
#11860=CARTESIAN_POINT('Ctrl Pts',(-15.8548776335165,8.26690043733163,-12.7703819477842));
#11861=CARTESIAN_POINT('Ctrl Pts',(-15.7838082658192,8.32314897453989,-12.7819107053312));
#11862=CARTESIAN_POINT('Ctrl Pts',(-15.7107906519688,8.38093946997536,-12.7937555042089));
#11863=CARTESIAN_POINT('Ctrl Pts',(-15.6395269896275,8.44096333239077,-12.8066275852114));
#11864=CARTESIAN_POINT('Ctrl Pts',(-15.5698762835546,8.50282830727392,-12.8203902527625));
#11865=CARTESIAN_POINT('Ctrl Pts',(-15.5466981609681,8.52341552099364,-12.8249701459697));
#11866=CARTESIAN_POINT('Ctrl Pts',(-15.5236987594059,8.5442070222161,-12.8296487881716));
#11867=CARTESIAN_POINT('Ctrl Pts',(-15.5008731781905,8.56518952756248,-12.8344215077166));
#11868=CARTESIAN_POINT('Ctrl Pts',(-15.4385988825786,8.62243541884092,-12.8474427642187));
#11869=CARTESIAN_POINT('Ctrl Pts',(-15.3777011585566,8.68106595956029,-12.8611612425515));
#11870=CARTESIAN_POINT('Ctrl Pts',(-15.3182018865546,8.74069382312877,-12.8754501442092));
#11871=CARTESIAN_POINT('Ctrl Pts',(-15.2564420923887,8.80258709436762,-12.8902819160199));
#11872=CARTESIAN_POINT('Ctrl Pts',(-15.1960523906305,8.86568736323019,-12.9057609205674));
#11873=CARTESIAN_POINT('Ctrl Pts',(-15.1370245917722,8.92967013781512,-12.9217807326603));
#11874=CARTESIAN_POINT('Ctrl Pts',(-15.0751539679737,8.99673437284488,-12.9385720714277));
#11875=CARTESIAN_POINT('Ctrl Pts',(-15.0147794430409,9.06476837724042,-12.955957604799));
#11876=CARTESIAN_POINT('Ctrl Pts',(-14.9558876408858,9.13345255195956,-12.973832558441));
#11877=CARTESIAN_POINT('Ctrl Pts',(-14.941745213388,9.14994654476789,-12.9781250953759));
#11878=CARTESIAN_POINT('Ctrl Pts',(-14.9276882808297,9.16647825760667,-12.9824459317766));
#11879=CARTESIAN_POINT('Ctrl Pts',(-14.9137166409377,9.18304367617656,-12.9867937549488));
#11880=CARTESIAN_POINT('Ctrl Pts',(-14.8443822685258,9.26524969559609,-13.0083698614999));
#11881=CARTESIAN_POINT('Ctrl Pts',(-14.7769243288711,9.34848879466141,-13.0306551587621));
#11882=CARTESIAN_POINT('Ctrl Pts',(-14.7110830067531,9.43264075175323,-13.0535945525926));
#11883=CARTESIAN_POINT('Ctrl Pts',(-14.6419151645199,9.52104434245437,-13.0776929200364));
#11884=CARTESIAN_POINT('Ctrl Pts',(-14.574531492047,9.61045552746631,-13.1025131517201));
#11885=CARTESIAN_POINT('Ctrl Pts',(-14.508658780167,9.7007827075362,-13.1280111392882));
#11886=CARTESIAN_POINT('Ctrl Pts',(-14.464101115013,9.76188188091148,-13.1452585056063));
#11887=CARTESIAN_POINT('Ctrl Pts',(-14.4202353698703,9.82340116495587,-13.1628163911151));
#11888=CARTESIAN_POINT('Ctrl Pts',(-14.376983382446,9.88532296597228,-13.180675825673));
#11889=CARTESIAN_POINT('Ctrl Pts',(-14.3247407934093,9.96011618116435,-13.2022476228458));
#11890=CARTESIAN_POINT('Ctrl Pts',(-14.2733952776958,10.0354996811099,-13.2242602480238));
#11891=CARTESIAN_POINT('Ctrl Pts',(-14.2228316908371,10.111478019192,-13.2467171132975));
#11892=CARTESIAN_POINT('Ctrl Pts',(-14.1455756462056,10.2275652321953,-13.2810289312213));
#11893=CARTESIAN_POINT('Ctrl Pts',(-14.070305718922,10.3447938290241,-13.3163058267544));
#11894=CARTESIAN_POINT('Ctrl Pts',(-13.9967407810488,10.4630236267724,-13.3525118459524));
#11895=CARTESIAN_POINT('Ctrl Pts',(-13.9578439948862,10.5255365479276,-13.3716554465217));
#11896=CARTESIAN_POINT('Ctrl Pts',(-13.9194243133811,10.5883301347506,-13.3910591092213));
#11897=CARTESIAN_POINT('Ctrl Pts',(-13.8814429470248,10.6513883422587,-13.4107195192154));
#11898=CARTESIAN_POINT('Ctrl Pts',(-13.8087592766334,10.7720607247897,-13.4483429882175));
#11899=CARTESIAN_POINT('Ctrl Pts',(-13.7376959033737,10.8936995222114,-13.4869103870559));
#11900=CARTESIAN_POINT('Ctrl Pts',(-13.6681560963966,11.015983366519,-13.526345490624));
#11901=CARTESIAN_POINT('Ctrl Pts',(-13.592500863716,11.1490210192869,-13.5692485711174));
#11902=CARTESIAN_POINT('Ctrl Pts',(-13.5186486051634,11.282822820578,-13.6131786525212));
#11903=CARTESIAN_POINT('Ctrl Pts',(-13.4464916370684,11.4170275975458,-13.6580628050807));
#11904=CARTESIAN_POINT('Ctrl Pts',(-13.4381590557207,11.4325253692907,-13.6632459615006));
#11905=CARTESIAN_POINT('Ctrl Pts',(-13.4298491021049,11.448028560653,-13.6684418663174));
#11906=CARTESIAN_POINT('Ctrl Pts',(-13.4215616267315,11.4635366486352,-13.6736504266539));
#11907=CARTESIAN_POINT('Ctrl Pts',(-13.3957800509804,11.5117808879307,-13.6898537801265));
#11908=CARTESIAN_POINT('Ctrl Pts',(-13.3701991365705,11.560096143354,-13.706184919204));
#11909=CARTESIAN_POINT('Ctrl Pts',(-13.3448076869915,11.6084844905147,-13.7226484987598));
#11910=CARTESIAN_POINT('Ctrl Pts',(-13.2498225662632,11.7894971177225,-13.7842359668902));
#11911=CARTESIAN_POINT('Ctrl Pts',(-13.1575527637327,11.9714205682347,-13.8476343858048));
#11912=CARTESIAN_POINT('Ctrl Pts',(-13.0676927983035,12.1538289736455,-13.912913228778));
#11913=CARTESIAN_POINT('Ctrl Pts',(-13.0310870527492,12.2281356534171,-13.9395055015942));
#11914=CARTESIAN_POINT('Ctrl Pts',(-12.9948815747046,12.3025233034365,-13.9664097879093));
#11915=CARTESIAN_POINT('Ctrl Pts',(-12.9590571742035,12.3769650887378,-13.9936305724574));
#11916=CARTESIAN_POINT('Ctrl Pts',(-12.8917900984241,12.5167435956483,-14.0447427348763));
#11917=CARTESIAN_POINT('Ctrl Pts',(-12.8256706149678,12.6571275035442,-14.0971253811225));
#11918=CARTESIAN_POINT('Ctrl Pts',(-12.7608591759401,12.7973698710114,-14.1505956618139));
#11919=CARTESIAN_POINT('Ctrl Pts',(-12.7064224840691,12.915162820213,-14.1955066410781));
#11920=CARTESIAN_POINT('Ctrl Pts',(-12.6529076763499,13.0328551936126,-14.2411843088393));
#11921=CARTESIAN_POINT('Ctrl Pts',(-12.6003906189451,13.15,-14.2875));
#11922=CARTESIAN_POINT('Origin',(-8.09752352946338,25.4,-24.0746778314848));
#11923=CARTESIAN_POINT('',(-3.19820054762184,-21.9,-20.0349830014761));
#11924=CARTESIAN_POINT('Origin',(-8.09752352946338,-21.9,-24.0746778314848));
#11925=CARTESIAN_POINT('Ctrl Pts',(-3.19820054762184,-21.9,-20.0349830014761));
#11926=CARTESIAN_POINT('Ctrl Pts',(-3.25878664769386,-21.9000000083571,
-19.961504462885));
#11927=CARTESIAN_POINT('Ctrl Pts',(-3.32027867353187,-21.9054435048663,
-19.8902504786465));
#11928=CARTESIAN_POINT('Ctrl Pts',(-3.38271157237758,-21.9155046710484,
-19.8210264481285));
#11929=CARTESIAN_POINT('Ctrl Pts',(-3.44795761695358,-21.926019180375,-19.7486832722642));
#11930=CARTESIAN_POINT('Ctrl Pts',(-3.51423117414105,-21.9415773497121,
-19.6785571332404));
#11931=CARTESIAN_POINT('Ctrl Pts',(-3.5815792215889,-21.9612924550953,-19.6104423872282));
#11932=CARTESIAN_POINT('Ctrl Pts',(-3.65454948264978,-21.9826533770696,
-19.5366414236227));
#11933=CARTESIAN_POINT('Ctrl Pts',(-3.72878097791152,-22.0088947211577,
-19.4652016366644));
#11934=CARTESIAN_POINT('Ctrl Pts',(-3.80434326748668,-22.0389456239223,
-19.3958807427751));
#11935=CARTESIAN_POINT('Ctrl Pts',(-3.81864012116223,-22.0446314410417,
-19.3827647998601));
#11936=CARTESIAN_POINT('Ctrl Pts',(-3.83298464569427,-22.0504537744497,
-19.3697247637157));
#11937=CARTESIAN_POINT('Ctrl Pts',(-3.84737735413469,-22.056405549946,-19.3567590646729));
#11938=CARTESIAN_POINT('Ctrl Pts',(-3.85146313648624,-22.0580951318189,
-19.3530783797939));
#11939=CARTESIAN_POINT('Ctrl Pts',(-3.85555075261669,-22.0597946861621,
-19.3494055600629));
#11940=CARTESIAN_POINT('Ctrl Pts',(-3.85964020896223,-22.0615041254605,
-19.3457405697024));
#11941=CARTESIAN_POINT('Ctrl Pts',(-3.93897962430439,-22.0946689041092,
-19.2746362057315));
#11942=CARTESIAN_POINT('Ctrl Pts',(-4.01875388994255,-22.1314339084887,
-19.2067072527322));
#11943=CARTESIAN_POINT('Ctrl Pts',(-4.09898053060866,-22.1711120177018,
-19.1416659844961));
#11944=CARTESIAN_POINT('Ctrl Pts',(-4.18540780668146,-22.2138568075937,
-19.0715977428336));
#11945=CARTESIAN_POINT('Ctrl Pts',(-4.2723599814154,-22.2599827034751,-19.0048807754165));
#11946=CARTESIAN_POINT('Ctrl Pts',(-4.35986578198443,-22.3086850460383,
-18.9411866314663));
#11947=CARTESIAN_POINT('Ctrl Pts',(-4.42370622049564,-22.3442161638104,
-18.8947181453324));
#11948=CARTESIAN_POINT('Ctrl Pts',(-4.48784147647386,-22.3811198321359,
-18.8498592500996));
#11949=CARTESIAN_POINT('Ctrl Pts',(-4.55228515966479,-22.4190978671498,
-18.806491720188));
#11950=CARTESIAN_POINT('Ctrl Pts',(-4.55742937494407,-22.4221294627744,
-18.803029908278));
#11951=CARTESIAN_POINT('Ctrl Pts',(-4.56257628221482,-22.4251683970662,
-18.7995771008193));
#11952=CARTESIAN_POINT('Ctrl Pts',(-4.56772588494067,-22.4282145883129,
-18.7961332749495));
#11953=CARTESIAN_POINT('Ctrl Pts',(-4.71481038542885,-22.5152208180672,
-18.6977696856022));
#11954=CARTESIAN_POINT('Ctrl Pts',(-4.86420124525512,-22.6081793599833,
-18.6066604878163));
#11955=CARTESIAN_POINT('Ctrl Pts',(-5.01562596722791,-22.7050300051394,
-18.5225574277292));
#11956=CARTESIAN_POINT('Ctrl Pts',(-5.16862236887894,-22.8028858903173,
-18.4375814383826));
#11957=CARTESIAN_POINT('Ctrl Pts',(-5.32369490141207,-22.9047152085253,
-18.359757839249));
#11958=CARTESIAN_POINT('Ctrl Pts',(-5.48057109348493,-23.0084452512491,
-18.288838145327));
#11959=CARTESIAN_POINT('Ctrl Pts',(-5.64018244583602,-23.1139838430508,
-18.2166819557506));
#11960=CARTESIAN_POINT('Ctrl Pts',(-5.80166083081389,-23.221490118629,-18.1516724956205));
#11961=CARTESIAN_POINT('Ctrl Pts',(-5.96472994459809,-23.3288332572481,
-18.093555430662));
#11962=CARTESIAN_POINT('Ctrl Pts',(-6.00079065213521,-23.3525708580606,
-18.0807035641512));
#11963=CARTESIAN_POINT('Ctrl Pts',(-6.03692919164292,-23.3763006768841,
-18.0681887778408));
#11964=CARTESIAN_POINT('Ctrl Pts',(-6.07314264709753,-23.4,-18.0560083736136));
#11965=CARTESIAN_POINT('Ctrl Pts',(-6.07314264709754,13.15,-18.0560083736136));
#11966=CARTESIAN_POINT('Ctrl Pts',(-5.97181996734248,12.9711603486608,-18.0900882806898));
#11967=CARTESIAN_POINT('Ctrl Pts',(-5.87130801630144,12.7922384032894,-18.1267220226218));
#11968=CARTESIAN_POINT('Ctrl Pts',(-5.77140203340685,12.6135684723799,-18.1660441169748));
#11969=CARTESIAN_POINT('Ctrl Pts',(-5.67731388552087,12.4453030452741,-18.2030763639081));
#11970=CARTESIAN_POINT('Ctrl Pts',(-5.58376322164663,12.2772593406106,-18.2424932633217));
#11971=CARTESIAN_POINT('Ctrl Pts',(-5.49059061374234,12.10972986541,-18.2844480350073));
#11972=CARTESIAN_POINT('Ctrl Pts',(-5.40407677968078,11.9541732319324,-18.3234044218395));
#11973=CARTESIAN_POINT('Ctrl Pts',(-5.31788895518178,11.7990589449033,-18.364549187312));
#11974=CARTESIAN_POINT('Ctrl Pts',(-5.23190911158772,11.6446517025337,-18.4080371962308));
#11975=CARTESIAN_POINT('Ctrl Pts',(-5.22529143778171,11.6327673268408,-18.4113843697714));
#11976=CARTESIAN_POINT('Ctrl Pts',(-5.21867500086194,11.6208871598949,-18.4147454404937));
#11977=CARTESIAN_POINT('Ctrl Pts',(-5.21205974944158,11.6090113330872,-18.4181204869383));
#11978=CARTESIAN_POINT('Ctrl Pts',(-5.1848316235959,11.5601308769573,-18.4320120510659));
#11979=CARTESIAN_POINT('Ctrl Pts',(-5.1576259896201,11.511329719366,-18.4461391252805));
#11980=CARTESIAN_POINT('Ctrl Pts',(-5.13043998234374,11.4626185033488,-18.4605069020915));
#11981=CARTESIAN_POINT('Ctrl Pts',(-5.04825349547858,11.3153587871761,-18.503942375648));
#11982=CARTESIAN_POINT('Ctrl Pts',(-4.96623254825319,11.1688712789634,-18.5495431771531));
#11983=CARTESIAN_POINT('Ctrl Pts',(-4.88422351176766,11.023341194086,-18.5976181451075));
#11984=CARTESIAN_POINT('Ctrl Pts',(-4.80536483798301,10.8834016218021,-18.6438463216304));
#11985=CARTESIAN_POINT('Ctrl Pts',(-4.72651736403294,10.7443469551293,-18.6923620873245));
#11986=CARTESIAN_POINT('Ctrl Pts',(-4.6475479022612,10.6063775970585,-18.7434712498276));
#11987=CARTESIAN_POINT('Ctrl Pts',(-4.57238550279757,10.475059644873,-18.7921164754899));
#11988=CARTESIAN_POINT('Ctrl Pts',(-4.49711275367302,10.344724674812,-18.8431110048543));
#11989=CARTESIAN_POINT('Ctrl Pts',(-4.42161551358169,10.2155824305894,-18.8967487338862));
#11990=CARTESIAN_POINT('Ctrl Pts',(-4.40218914607156,10.1823525443801,-18.9105503806129));
#11991=CARTESIAN_POINT('Ctrl Pts',(-4.38274791199463,10.1492018354882,-18.9245271982718));
#11992=CARTESIAN_POINT('Ctrl Pts',(-4.36328985471379,10.116134325549,-18.9386845498513));
#11993=CARTESIAN_POINT('Ctrl Pts',(-4.31906701210315,10.0409809190982,-18.9708603380942));
#11994=CARTESIAN_POINT('Ctrl Pts',(-4.27475033656031,9.96626705526661,-19.0039731983406));
#11995=CARTESIAN_POINT('Ctrl Pts',(-4.23030242157944,9.89202045142478,-19.038101523747));
#11996=CARTESIAN_POINT('Ctrl Pts',(-4.17007877614573,9.7914217811305,-19.0843428866863));
#11997=CARTESIAN_POINT('Ctrl Pts',(-4.10961908431761,9.69169193896628,-19.1324643246693));
#11998=CARTESIAN_POINT('Ctrl Pts',(-4.04884198562672,9.59300570028752,-19.1827615424047));
#11999=CARTESIAN_POINT('Ctrl Pts',(-4.01019530923867,9.53025352533475,-19.2147443178072));
#12000=CARTESIAN_POINT('Ctrl Pts',(-3.97142032686885,9.46792401681482,-19.2476074389096));
#12001=CARTESIAN_POINT('Ctrl Pts',(-3.93249626019989,9.40607058542615,-19.2814341079721));
#12002=CARTESIAN_POINT('Ctrl Pts',(-3.88593531573127,9.3320815490653,-19.3218975485774));
#12003=CARTESIAN_POINT('Ctrl Pts',(-3.83914319459572,9.25875668204225,-19.3637545119824));
#12004=CARTESIAN_POINT('Ctrl Pts',(-3.79206853549414,9.18618721050011,-19.4071777195395));
#12005=CARTESIAN_POINT('Ctrl Pts',(-3.7419706788984,9.10895723055056,-19.4533896234946));
#12006=CARTESIAN_POINT('Ctrl Pts',(-3.69180314879746,9.03297713417334,-19.501153477267));
#12007=CARTESIAN_POINT('Ctrl Pts',(-3.64157577202708,8.95848778471708,-19.5506232829686));
#12008=CARTESIAN_POINT('Ctrl Pts',(-3.591700633242,8.88452081926863,-19.5997461634312));
#12009=CARTESIAN_POINT('Ctrl Pts',(-3.54176640274007,8.81202334048803,-19.6505510647792));
#12010=CARTESIAN_POINT('Ctrl Pts',(-3.49179225292663,8.74127840230459,-19.703205021262));
#12011=CARTESIAN_POINT('Ctrl Pts',(-3.45031120448795,8.68255655874079,-19.7469104435154));
#12012=CARTESIAN_POINT('Ctrl Pts',(-3.40878815829155,8.62503122998402,-19.791904833991));
#12013=CARTESIAN_POINT('Ctrl Pts',(-3.36721112089652,8.56885520307109,-19.8383298148915));
#12014=CARTESIAN_POINT('Ctrl Pts',(-3.32614372687987,8.51336777115995,-19.8841857272487));
#12015=CARTESIAN_POINT('Ctrl Pts',(-3.28499911832725,8.45914957374367,-19.9314552410215));
#12016=CARTESIAN_POINT('Ctrl Pts',(-3.24375684075465,8.40640557245158,-19.9803399318371));
#12017=CARTESIAN_POINT('Ctrl Pts',(-3.20424421247424,8.35587358829024,-20.0271744601533));
#12018=CARTESIAN_POINT('Ctrl Pts',(-3.16464194043481,8.30669462479412,-20.075491474184));
#12019=CARTESIAN_POINT('Ctrl Pts',(-3.12493769096898,8.25909114270198,-20.12548869821));
#12020=CARTESIAN_POINT('Ctrl Pts',(-3.09875754613535,8.22770241044979,-20.1584558134153));
#12021=CARTESIAN_POINT('Ctrl Pts',(-3.07253317739119,8.19699952044321,-20.1921538645661));
#12022=CARTESIAN_POINT('Ctrl Pts',(-3.04626248231991,8.16705743584219,-20.2266449579396));
#12023=CARTESIAN_POINT('Ctrl Pts',(-3.01950180981585,8.13655689834508,-20.2617793482392));
#12024=CARTESIAN_POINT('Ctrl Pts',(-2.99270944889829,8.10686980879576,-20.2977147377636));
#12025=CARTESIAN_POINT('Ctrl Pts',(-2.96586636824719,8.07806532466685,-20.334544841819));
#12026=CARTESIAN_POINT('Ctrl Pts',(-2.93487296250628,8.04480725435189,-20.377069407956));
#12027=CARTESIAN_POINT('Ctrl Pts',(-2.90383026540122,8.01279246823105,-20.4208041851031));
#12028=CARTESIAN_POINT('Ctrl Pts',(-2.87280600557641,7.98223072787833,-20.465746960996));
#12029=CARTESIAN_POINT('Ctrl Pts',(-2.84276929780852,7.9526418168443,-20.5092591360937));
#12030=CARTESIAN_POINT('Ctrl Pts',(-2.81274971365855,7.92441470275159,-20.5539038580238));
#12031=CARTESIAN_POINT('Ctrl Pts',(-2.78282604631469,7.89778233068622,-20.5996722896361));
#12032=CARTESIAN_POINT('Ctrl Pts',(-2.75380560115464,7.87195383566507,-20.6440592374124));
#12033=CARTESIAN_POINT('Ctrl Pts',(-2.72487522323847,7.84762505828801,-20.6895032879898));
#12034=CARTESIAN_POINT('Ctrl Pts',(-2.69612555324366,7.82505223561181,-20.7359867177464));
#12035=CARTESIAN_POINT('Ctrl Pts',(-2.6685106150068,7.80337034833633,-20.7806354751755));
#12036=CARTESIAN_POINT('Ctrl Pts',(-2.64106230558355,7.78330843075126,-20.8262433432298));
#12037=CARTESIAN_POINT('Ctrl Pts',(-2.61388021809145,7.76513667663637,-20.8727829774746));
#12038=CARTESIAN_POINT('Ctrl Pts',(-2.60866408756246,7.76164959193651,-20.881713741422));
#12039=CARTESIAN_POINT('Ctrl Pts',(-2.60345782197805,7.75823224576018,-20.8906787769713));
#12040=CARTESIAN_POINT('Ctrl Pts',(-2.59826221543221,7.75488674445212,-20.8996778314848));
#12041=CARTESIAN_POINT('Origin',(24.8980443547237,25.4,-5.02467783148466));
#12042=CARTESIAN_POINT('',(18.9499045174787,-21.9,-7.24776858010006));
#12043=CARTESIAN_POINT('Ctrl Pts',(18.6735332660427,-23.4,-3.76850837361349));
#12044=CARTESIAN_POINT('Ctrl Pts',(18.6427754562218,-23.3035563483767,-3.92091800839177));
#12045=CARTESIAN_POINT('Ctrl Pts',(18.6175035681029,-23.2068396389513,-4.07465508966213));
#12046=CARTESIAN_POINT('Ctrl Pts',(18.597886266332,-23.1112816991265,-4.22977879778428));
#12047=CARTESIAN_POINT('Ctrl Pts',(18.5793498417064,-23.0209888255381,-4.37635547570033));
#12048=CARTESIAN_POINT('Ctrl Pts',(18.5658622530517,-22.9317288897395,-4.52417037570528));
#12049=CARTESIAN_POINT('Ctrl Pts',(18.5576066734871,-22.8447237855104,-4.67328040594355));
#12050=CARTESIAN_POINT('Ctrl Pts',(18.550083524438,-22.7654377266669,-4.80916147563916));
#12051=CARTESIAN_POINT('Ctrl Pts',(18.5469055500268,-22.688023391011,-4.94611816810261));
#12052=CARTESIAN_POINT('Ctrl Pts',(18.5482422492798,-22.6134330595748,-5.08419756762781));
#12053=CARTESIAN_POINT('Ctrl Pts',(18.5493897722915,-22.5493991180712,-5.20273529258207));
#12054=CARTESIAN_POINT('Ctrl Pts',(18.5538649455709,-22.4874464626935,-5.32210048770187));
#12055=CARTESIAN_POINT('Ctrl Pts',(18.5617935035834,-22.4282022173725,-5.4423250357486));
#12056=CARTESIAN_POINT('Ctrl Pts',(18.5622006166617,-22.4251601626828,-5.44849828765209));
#12057=CARTESIAN_POINT('Ctrl Pts',(18.5626168311325,-22.4221253454031,-5.45467369029037));
#12058=CARTESIAN_POINT('Ctrl Pts',(18.5630421649904,-22.4190978469191,-5.46085125802884));
#12059=CARTESIAN_POINT('Ctrl Pts',(18.5704667943542,-22.3662498224316,-5.56868690281898));
#12060=CARTESIAN_POINT('Ctrl Pts',(18.5806898704857,-22.3154805383714,-5.67744898745817));
#12061=CARTESIAN_POINT('Ctrl Pts',(18.5939729051555,-22.2675991944941,-5.78732953813166));
#12062=CARTESIAN_POINT('Ctrl Pts',(18.6062339812058,-22.2234017039909,-5.88875619414482));
#12063=CARTESIAN_POINT('Ctrl Pts',(18.6211023693495,-22.1816645409984,-5.9911357802801));
#12064=CARTESIAN_POINT('Ctrl Pts',(18.6388065796653,-22.1430604940117,-6.09462575761987));
#12065=CARTESIAN_POINT('Ctrl Pts',(18.6521360572901,-22.1139955557083,-6.17254323107633));
#12066=CARTESIAN_POINT('Ctrl Pts',(18.6670734617826,-22.0867072848215,-6.25109024348722));
#12067=CARTESIAN_POINT('Ctrl Pts',(18.6837256783403,-22.0614998943556,-6.33033707037954));
#12068=CARTESIAN_POINT('Ctrl Pts',(18.684854008829,-22.0597918774616,-6.3357067225579));
#12069=CARTESIAN_POINT('Ctrl Pts',(18.6859900272502,-22.0580937292927,-6.34107869209401));
#12070=CARTESIAN_POINT('Ctrl Pts',(18.6871337613023,-22.0564055371513,-6.34645300238936));
#12071=CARTESIAN_POINT('Ctrl Pts',(18.708148865036,-22.0253864965688,-6.44520121064056));
#12072=CARTESIAN_POINT('Ctrl Pts',(18.731565451134,-21.9978800256313,-6.54382562252798));
#12073=CARTESIAN_POINT('Ctrl Pts',(18.757547417001,-21.9749039650105,-6.64250010567014));
#12074=CARTESIAN_POINT('Ctrl Pts',(18.7820352329043,-21.9532491931759,-6.73550009612159));
#12075=CARTESIAN_POINT('Ctrl Pts',(18.8088018953359,-21.9356181609281,-6.82854447867061));
#12076=CARTESIAN_POINT('Ctrl Pts',(18.838001488254,-21.922905503098,-6.92177945640448));
#12077=CARTESIAN_POINT('Ctrl Pts',(18.8654018755781,-21.9109761673213,-7.00926952892805));
#12078=CARTESIAN_POINT('Ctrl Pts',(18.8949446624786,-21.9033774739727,-7.09692737855105));
#12079=CARTESIAN_POINT('Ctrl Pts',(18.9267718005847,-21.9008931019119,-7.18487534317515));
#12080=CARTESIAN_POINT('Ctrl Pts',(18.9343523672068,-21.900301375824,-7.20582273099513));
#12081=CARTESIAN_POINT('Ctrl Pts',(18.9420625907237,-21.9000000019656,-7.22678658601776));
#12082=CARTESIAN_POINT('Ctrl Pts',(18.9499045174787,-21.9,-7.24776858010006));
#12083=CARTESIAN_POINT('Origin',(24.8980443547237,-21.9,-5.02467783148466));
#12084=CARTESIAN_POINT('Ctrl Pts',(19.3987830406925,7.75488674445212,-8.19967783148469));
#12085=CARTESIAN_POINT('Ctrl Pts',(19.3659933398565,7.77600035063379,-8.14288440367171));
#12086=CARTESIAN_POINT('Ctrl Pts',(19.3347983130256,7.79969631458858,-8.08684223874884));
#12087=CARTESIAN_POINT('Ctrl Pts',(19.3050236136449,7.82564845387891,-8.03146894177519));
#12088=CARTESIAN_POINT('Ctrl Pts',(19.274510466767,7.85224423668899,-7.97472232203361));
#12089=CARTESIAN_POINT('Ctrl Pts',(19.2454890567992,7.88120973563673,-7.91867817937499));
#12090=CARTESIAN_POINT('Ctrl Pts',(19.2177926283953,7.91224591462514,-7.86325066964015));
#12091=CARTESIAN_POINT('Ctrl Pts',(19.1889838553875,7.9445285693584,-7.80559707896577));
#12092=CARTESIAN_POINT('Ctrl Pts',(19.1616086716191,7.97905171373433,-7.74861066271193));
#12093=CARTESIAN_POINT('Ctrl Pts',(19.1355008176972,8.01553158395357,-7.69219756552196));
#12094=CARTESIAN_POINT('Ctrl Pts',(19.1213519132884,8.03530150445801,-7.66162502126256));
#12095=CARTESIAN_POINT('Ctrl Pts',(19.1075755834705,8.05564699923641,-7.63122090588109));
#12096=CARTESIAN_POINT('Ctrl Pts',(19.0941477565058,8.07652873453469,-7.60097057057968));
#12097=CARTESIAN_POINT('Ctrl Pts',(19.0765900909801,8.10383281917408,-7.56141649599528));
#12098=CARTESIAN_POINT('Ctrl Pts',(19.0596305575383,8.1320607616409,-7.52212648307875));
#12099=CARTESIAN_POINT('Ctrl Pts',(19.0432284984429,8.16115913750229,-7.48307015825894));
#12100=CARTESIAN_POINT('Ctrl Pts',(19.0141380564244,8.21276757342507,-7.41380045583827));
#12101=CARTESIAN_POINT('Ctrl Pts',(18.9869139995712,8.26690043732857,-7.34553583063077));
#12102=CARTESIAN_POINT('Ctrl Pts',(18.9613635126329,8.32314897453513,-7.27822357400233));
#12103=CARTESIAN_POINT('Ctrl Pts',(18.9351126024384,8.3809394699705,-7.20906606604536));
#12104=CARTESIAN_POINT('Ctrl Pts',(18.9106283204154,8.44096333238581,-7.14091388358974));
#12105=CARTESIAN_POINT('Ctrl Pts',(18.887721787102,8.50282830726884,-7.07371326896348));
#12106=CARTESIAN_POINT('Ctrl Pts',(18.8800990296721,8.52341552099025,-7.05135047938608));
#12107=CARTESIAN_POINT('Ctrl Pts',(18.8726511518925,8.54420702221443,-7.02909309225845));
#12108=CARTESIAN_POINT('Ctrl Pts',(18.8653716576552,8.56518952756256,-7.00693919929548));
#12109=CARTESIAN_POINT('Ctrl Pts',(18.8455112487693,8.62243541884095,-6.94649744904164));
#12110=CARTESIAN_POINT('Ctrl Pts',(18.8269429374958,8.68106595956028,-6.88689923383952));
#12111=CARTESIAN_POINT('Ctrl Pts',(18.8095678533225,8.74069382312873,-6.82822690195023));
#12112=CARTESIAN_POINT('Ctrl Pts',(18.7915326474107,8.8025870943678,-6.76732546536456));
#12113=CARTESIAN_POINT('Ctrl Pts',(18.774743007695,8.8656873632306,-6.70728694724099));
#12114=CARTESIAN_POINT('Ctrl Pts',(18.7591026725021,8.92967013781577,-6.64815746785353));
#12115=CARTESIAN_POINT('Ctrl Pts',(18.742709086539,8.9967343728454,-6.58618026651254));
#12116=CARTESIAN_POINT('Ctrl Pts',(18.7275781376305,9.06476837724079,-6.52520162749384));
#12117=CARTESIAN_POINT('Ctrl Pts',(18.7136124004985,9.13345255195979,-6.46526235393202));
#12118=CARTESIAN_POINT('Ctrl Pts',(18.7102586327819,9.14994654476804,-6.45086838398035));
#12119=CARTESIAN_POINT('Ctrl Pts',(18.7069721205914,9.16647825760674,-6.4365343050853));
#12120=CARTESIAN_POINT('Ctrl Pts',(18.7037516259637,9.18304367617655,-6.42226059842027));
#12121=CARTESIAN_POINT('Ctrl Pts',(18.687769896146,9.26524969559492,-6.35142721728163));
#12122=CARTESIAN_POINT('Ctrl Pts',(18.6733405598788,9.3484887946591,-6.28186427922348));
#12123=CARTESIAN_POINT('Ctrl Pts',(18.6602859966245,9.43264075174974,-6.21337432473624));
#12124=CARTESIAN_POINT('Ctrl Pts',(18.646571873904,9.5210443424501,-6.14142403251602));
#12125=CARTESIAN_POINT('Ctrl Pts',(18.6343749888335,9.61045552746124,-6.07065794451291));
#12126=CARTESIAN_POINT('Ctrl Pts',(18.6235205378729,9.70078270753026,-6.00086150882515));
#12127=CARTESIAN_POINT('Ctrl Pts',(18.6161783626755,9.76188188090751,-5.95364975570785));
#12128=CARTESIAN_POINT('Ctrl Pts',(18.6094510649912,9.82340116495387,-5.90688196330237));
#12129=CARTESIAN_POINT('Ctrl Pts',(18.6032917953032,9.88532296597222,-5.86049492614831));
#12130=CARTESIAN_POINT('Ctrl Pts',(18.5958522251418,9.96011618116425,-5.80446561829669));
#12131=CARTESIAN_POINT('Ctrl Pts',(18.5892429598932,10.0354996811098,-5.74899278472943));
#12132=CARTESIAN_POINT('Ctrl Pts',(18.5834093822803,10.1114780191919,-5.69397500136636));
#12133=CARTESIAN_POINT('Ctrl Pts',(18.5744962659343,10.227565232225,-5.60991339513627));
#12134=CARTESIAN_POINT('Ctrl Pts',(18.5674119899894,10.3447938290842,-5.52708927818022));
#12135=CARTESIAN_POINT('Ctrl Pts',(18.5619848534477,10.4630236268635,-5.44527716353466));
#12136=CARTESIAN_POINT('Ctrl Pts',(18.5591153047811,10.5255365479887,-5.40201975832896));
#12137=CARTESIAN_POINT('Ctrl Pts',(18.5567095288543,10.5883301347813,-5.35904550681142));
#12138=CARTESIAN_POINT('Ctrl Pts',(18.5547452601808,10.6513883422589,-5.31632247370023));
#12139=CARTESIAN_POINT('Ctrl Pts',(18.550986304919,10.7720607248062,-5.23456483418908));
#12140=CARTESIAN_POINT('Ctrl Pts',(18.5488549654409,10.8936995222446,-5.15373844823809));
#12141=CARTESIAN_POINT('Ctrl Pts',(18.5482368634436,11.015983366569,-5.07379765702776));
#12142=CARTESIAN_POINT('Ctrl Pts',(18.5475644047114,11.1490210193612,-4.98682676333589));
#12143=CARTESIAN_POINT('Ctrl Pts',(18.548682841922,11.2828228206765,-4.90090379058647));
#12144=CARTESIAN_POINT('Ctrl Pts',(18.5514751742199,11.4170275976682,-4.81597194686246));
#12145=CARTESIAN_POINT('Ctrl Pts',(18.5517976286767,11.4325253693733,-4.80616414155158));
#12146=CARTESIAN_POINT('Ctrl Pts',(18.5521424374349,11.4480285606957,-4.79636955823295));
#12147=CARTESIAN_POINT('Ctrl Pts',(18.5525094453159,11.463536648638,-4.78658811388329));
#12148=CARTESIAN_POINT('Ctrl Pts',(18.5536511731741,11.5117808879334,-4.75615893759702));
#12149=CARTESIAN_POINT('Ctrl Pts',(18.555003897283,11.5600961433565,-4.72583964632702));
#12150=CARTESIAN_POINT('Ctrl Pts',(18.5565660506262,11.6084844905168,-4.69561821617437));
#12151=CARTESIAN_POINT('Ctrl Pts',(18.5624098021704,11.7894971162455,-4.58256495549814));
#12152=CARTESIAN_POINT('Ctrl Pts',(18.5711795421502,11.9714205652654,-4.47095775394613));
#12153=CARTESIAN_POINT('Ctrl Pts',(18.5827826956393,12.1538289691793,-4.36049732049744));
#12154=CARTESIAN_POINT('Ctrl Pts',(18.5875094067414,12.2281356504364,-4.31549967760564));
#12155=CARTESIAN_POINT('Ctrl Pts',(18.5927064632334,12.302523301945,-4.27069266980417));
#12156=CARTESIAN_POINT('Ctrl Pts',(18.5983681540258,12.3769650887378,-4.22605743572654));
#12157=CARTESIAN_POINT('Ctrl Pts',(18.6089990472484,12.5167435958486,-4.14224635793386));
#12158=CARTESIAN_POINT('Ctrl Pts',(18.6213040079066,12.6571275039462,-4.05879388233315));
#12159=CARTESIAN_POINT('Ctrl Pts',(18.6352049098432,12.7973698716139,-3.97593038921648));
#12160=CARTESIAN_POINT('Ctrl Pts',(18.6468806128429,12.9151628206142,-3.9063313416461));
#12161=CARTESIAN_POINT('Ctrl Pts',(18.6596812296299,13.0328551938122,-3.83714732492099));
#12162=CARTESIAN_POINT('Ctrl Pts',(18.6735332660427,13.15,-3.76850837361349));
#12163=CARTESIAN_POINT('Origin',(24.8980443547236,25.4,5.02467783148503));
#12164=CARTESIAN_POINT('',(18.9499045174786,-21.9,7.24776858010033));
#12165=CARTESIAN_POINT('Origin',(24.8980443547236,-21.9,5.02467783148503));
#12166=CARTESIAN_POINT('Ctrl Pts',(18.9499045174786,-21.9,7.24776858010033));
#12167=CARTESIAN_POINT('Ctrl Pts',(18.9165632864596,-21.9000000083571,7.15856020902048));
#12168=CARTESIAN_POINT('Ctrl Pts',(18.8856015389054,-21.905443504867,7.06967956038967));
#12169=CARTESIAN_POINT('Ctrl Pts',(18.8568682193457,-21.9155046710502,6.98099906869269));
#12170=CARTESIAN_POINT('Ctrl Pts',(18.8268402135435,-21.9260191803779,6.88832274865634));
#12171=CARTESIAN_POINT('Ctrl Pts',(18.7992459742723,-21.9415773497166,6.79586509501603));
#12172=CARTESIAN_POINT('Ctrl Pts',(18.7739308975765,-21.9612924551018,6.70348260201988));
#12173=CARTESIAN_POINT('Ctrl Pts',(18.7465025188002,-21.9826533770779,6.60338802041375));
#12174=CARTESIAN_POINT('Ctrl Pts',(18.721749596084,-22.008894721168,6.50338176627315));
#12175=CARTESIAN_POINT('Ctrl Pts',(18.6994970857502,-22.038945623935,6.4032824569844));
#12176=CARTESIAN_POINT('Ctrl Pts',(18.6952867728324,-22.0446314410502,6.38434304706415));
#12177=CARTESIAN_POINT('Ctrl Pts',(18.6911660325344,-22.050453774454,6.36540030635649));
#12178=CARTESIAN_POINT('Ctrl Pts',(18.6871337620087,-22.0564055499457,6.34645300571088));
#12179=CARTESIAN_POINT('Ctrl Pts',(18.685989086576,-22.0580951318186,6.34107427196059));
#12180=CARTESIAN_POINT('Ctrl Pts',(18.6848521394506,-22.0597946861619,6.33569788268522));
#12181=CARTESIAN_POINT('Ctrl Pts',(18.6837228928666,-22.0615041254602,6.33032381442206));
#12182=CARTESIAN_POINT('Ctrl Pts',(18.6618144150191,-22.0946689041087,6.22606168322978));
#12183=CARTESIAN_POINT('Ctrl Pts',(18.6428733488885,-22.1314339084881,6.12301066612014));
#12184=CARTESIAN_POINT('Ctrl Pts',(18.6266592786348,-22.1711120177009,6.02101172312584));
#12185=CARTESIAN_POINT('Ctrl Pts',(18.6091920393942,-22.2138568075897,5.91112938564402));
#12186=CARTESIAN_POINT('Ctrl Pts',(18.5948895381154,-22.2599827034673,5.80246810970979));
#12187=CARTESIAN_POINT('Ctrl Pts',(18.5834816916671,-22.3086850460264,5.6948387914714));
#12188=CARTESIAN_POINT('Ctrl Pts',(18.575159021454,-22.3442161638022,5.61631710685588));
#12189=CARTESIAN_POINT('Ctrl Pts',(18.5683777065849,-22.3811198321318,5.53834489827507));
#12190=CARTESIAN_POINT('Ctrl Pts',(18.5630421655769,-22.4190978671499,5.46085126655351));
#12191=CARTESIAN_POINT('Ctrl Pts',(18.5626162561593,-22.4221294627745,5.4546653394841));
#12192=CARTESIAN_POINT('Ctrl Pts',(18.5621994908211,-22.4251683970663,5.44848158330734));
#12193=CARTESIAN_POINT('Ctrl Pts',(18.5617918514945,-22.4282145883129,5.44229998359246));
#12194=CARTESIAN_POINT('Ctrl Pts',(18.5501487347855,-22.5152208163553,5.26573927846711));
#12195=CARTESIAN_POINT('Ctrl Pts',(18.5459412848334,-22.6081793563307,5.09080840328421));
#12196=CARTESIAN_POINT('Ctrl Pts',(18.5488182589122,-22.7050299994319,4.91761922059265));
#12197=CARTESIAN_POINT('Ctrl Pts',(18.551725093913,-22.8028858825601,4.74263245873062));
#12198=CARTESIAN_POINT('Ctrl Pts',(18.5618641457036,-22.9047151986039,4.56942390981763));
#12199=CARTESIAN_POINT('Ctrl Pts',(18.5788839843097,-23.0084452391659,4.39810529844962));
#12200=CARTESIAN_POINT('Ctrl Pts',(18.5962005664483,-23.1139838291145,4.22379972045343));
#12201=CARTESIAN_POINT('Ctrl Pts',(18.6206399139399,-23.221490102855,4.05145060942632));
#12202=CARTESIAN_POINT('Ctrl Pts',(18.6518436149472,-23.3288332397547,3.88117008435452));
#12203=CARTESIAN_POINT('Ctrl Pts',(18.6587439273645,-23.3525708464022,3.84351465299085));
#12204=CARTESIAN_POINT('Ctrl Pts',(18.6659750759472,-23.3763006710624,3.80596035731296));
#12205=CARTESIAN_POINT('Ctrl Pts',(18.6735332660427,-23.4,3.76850837361377));
#12206=CARTESIAN_POINT('Ctrl Pts',(18.6735332660427,13.15,3.76850837361377));
#12207=CARTESIAN_POINT('Ctrl Pts',(18.6523859914636,12.9711603487853,3.87329634174011));
#12208=CARTESIAN_POINT('Ctrl Pts',(18.6338557671018,12.7922384035346,3.97865911562495));
#12209=CARTESIAN_POINT('Ctrl Pts',(18.6179567083012,12.613568472743,4.0848412819067));
#12210=CARTESIAN_POINT('Ctrl Pts',(18.6029835009531,12.4453030455777,4.18484013167159));
#12211=CARTESIAN_POINT('Ctrl Pts',(18.5903442052403,12.2772593408527,4.28556583286555));
#12212=CARTESIAN_POINT('Ctrl Pts',(18.5800917993731,12.1097298655906,4.3872330641218));
#12213=CARTESIAN_POINT('Ctrl Pts',(18.5705721029945,11.9541732323843,4.48163443544397));
#12214=CARTESIAN_POINT('Ctrl Pts',(18.5631106028855,11.7990589456247,4.57684766352013));
#12215=CARTESIAN_POINT('Ctrl Pts',(18.5577824015727,11.644651703523,4.67305239657088));
#12216=CARTESIAN_POINT('Ctrl Pts',(18.5573723019746,11.6327673274996,4.68045705717646));
#12217=CARTESIAN_POINT('Ctrl Pts',(18.5569748561328,11.6208871602234,4.6878675951984));
#12218=CARTESIAN_POINT('Ctrl Pts',(18.5565901063719,11.6090113330857,4.69528409440914));
#12219=CARTESIAN_POINT('Ctrl Pts',(18.555006490882,11.5601308769556,4.72581012515259));
#12220=CARTESIAN_POINT('Ctrl Pts',(18.5536380790451,11.5113297193643,4.75643443240897));
#12221=CARTESIAN_POINT('Ctrl Pts',(18.5524879351211,11.4626185033473,4.7871620937435));
#12222=CARTESIAN_POINT('Ctrl Pts',(18.5490109152155,11.3153587872477,4.88005541594978));
#12223=CARTESIAN_POINT('Ctrl Pts',(18.5474918941389,11.1688712791072,4.97388804059575));
#12224=CARTESIAN_POINT('Ctrl Pts',(18.5481215194284,11.0233411943008,5.0689474334615));
#12225=CARTESIAN_POINT('Ctrl Pts',(18.5487269577732,10.8834016220832,5.16035513648454));
#12226=CARTESIAN_POINT('Ctrl Pts',(18.5513191063689,10.7443469554757,5.25289693475043));
#12227=CARTESIAN_POINT('Ctrl Pts',(18.5560962085703,10.6063775974687,5.34684107597172));
#12228=CARTESIAN_POINT('Ctrl Pts',(18.5606430100288,10.4750596453383,5.4362562361061));
#12229=CARTESIAN_POINT('Ctrl Pts',(18.5671691933421,10.3447246753313,5.52694161369977));
#12230=CARTESIAN_POINT('Ctrl Pts',(18.5758722092291,10.2155824311613,5.61914300600576));
#12231=CARTESIAN_POINT('Ctrl Pts',(18.5781116021647,10.1823525447605,5.64286755727109));
#12232=CARTESIAN_POINT('Ctrl Pts',(18.5804952642956,10.1492018356779,5.66669256882812));
#12233=CARTESIAN_POINT('Ctrl Pts',(18.583026861788,10.1161343255489,5.6906224166687));
#12234=CARTESIAN_POINT('Ctrl Pts',(18.5887804904878,10.0409809190982,5.7450084159185));
#12235=CARTESIAN_POINT('Ctrl Pts',(18.5952987308817,9.96626705526658,5.79994421287305));
#12236=CARTESIAN_POINT('Ctrl Pts',(18.6026307701818,9.89202045142468,5.85550139909491));
#12237=CARTESIAN_POINT('Ctrl Pts',(18.6125651424763,9.79142178112723,5.93077728742091));
#12238=CARTESIAN_POINT('Ctrl Pts',(18.6240096843225,9.69169193896002,6.00719763544296));
#12239=CARTESIAN_POINT('Ctrl Pts',(18.6371798032762,9.59300570027836,6.08498075574783));
#12240=CARTESIAN_POINT('Ctrl Pts',(18.6455543610639,9.5302535253287,6.13444114697063));
#12241=CARTESIAN_POINT('Ctrl Pts',(18.6546271676009,9.46792401681184,6.18445282728303));
#12242=CARTESIAN_POINT('Ctrl Pts',(18.6644598889995,9.40607058542617,6.23507539236576));
#12243=CARTESIAN_POINT('Ctrl Pts',(18.6762217842539,9.33208154906527,6.2956300734025));
#12244=CARTESIAN_POINT('Ctrl Pts',(18.6890749173201,9.25875668204223,6.35708172070533));
#12245=CARTESIAN_POINT('Ctrl Pts',(18.7031431886276,9.18618721050011,6.41956117514028));
#12246=CARTESIAN_POINT('Ctrl Pts',(18.718114943111,9.10895723055633,6.48605314359989));
#12247=CARTESIAN_POINT('Ctrl Pts',(18.7343958888087,9.03297713418459,6.55338142599361));
#12248=CARTESIAN_POINT('Ctrl Pts',(18.7521243088799,8.95848778473355,6.62161451308793));
#12249=CARTESIAN_POINT('Ctrl Pts',(18.7697284018762,8.88452081927939,6.68936909052928));
#12250=CARTESIAN_POINT('Ctrl Pts',(18.7887596218306,8.81202334049326,6.75801585334146));
#12251=CARTESIAN_POINT('Ctrl Pts',(18.8093722108493,8.74127840230463,6.82762171485896));
#12252=CARTESIAN_POINT('Ctrl Pts',(18.8264816925845,8.68255655874079,6.88539806770923));
#12253=CARTESIAN_POINT('Ctrl Pts',(18.844686454666,8.62503122998396,6.94385527579565));
#12254=CARTESIAN_POINT('Ctrl Pts',(18.8641031487985,8.56885520307105,7.00307453684398));
#12255=CARTESIAN_POINT('Ctrl Pts',(18.883281836806,8.51336777115753,7.06156789951063));
#12256=CARTESIAN_POINT('Ctrl Pts',(18.9036461322825,8.45914957373892,7.12083493263501));
#12257=CARTESIAN_POINT('Ctrl Pts',(18.9253603775997,8.40640557244459,7.18099413813338));
#12258=CARTESIAN_POINT('Ctrl Pts',(18.9461639547566,8.35587358828098,7.23863034215543));
#12259=CARTESIAN_POINT('Ctrl Pts',(18.9682065803238,8.3066946247827,7.2970854228075));
#12260=CARTESIAN_POINT('Ctrl Pts',(18.9916533217175,8.25909114268859,7.35646892349916));
#12261=CARTESIAN_POINT('Ctrl Pts',(19.007113608556,8.22770241044106,7.39562515159708));
#12262=CARTESIAN_POINT('Ctrl Pts',(19.0231847925363,8.19699952043896,7.43518514669757));
#12263=CARTESIAN_POINT('Ctrl Pts',(19.0399196080641,8.16705743584222,7.47518178268543));
#12264=CARTESIAN_POINT('Ctrl Pts',(19.056966546358,8.1365568983451,7.51592440004612));
#12265=CARTESIAN_POINT('Ctrl Pts',(19.0746913261222,8.10686980879578,7.55709495999028));
#12266=CARTESIAN_POINT('Ctrl Pts',(19.0931655915326,8.07806532466688,7.59875680177766));
#12267=CARTESIAN_POINT('Ctrl Pts',(19.1144962432219,8.04480725435168,7.64686016156793));
#12268=CARTESIAN_POINT('Ctrl Pts',(19.1368503227078,8.01279246823063,7.69561131443679));
#12269=CARTESIAN_POINT('Ctrl Pts',(19.1602597784354,7.98223072787771,7.74495049952548));
#12270=CARTESIAN_POINT('Ctrl Pts',(19.1829240735601,7.95264181684349,7.79271913904772));
#12271=CARTESIAN_POINT('Ctrl Pts',(19.2065777448217,7.92441470275061,7.84103922249812));
#12272=CARTESIAN_POINT('Ctrl Pts',(19.2312525356177,7.89778233068509,7.88983809439884));
#12273=CARTESIAN_POINT('Ctrl Pts',(19.2551825374087,7.87195383566371,7.93716401102529));
#12274=CARTESIAN_POINT('Ctrl Pts',(19.2800730507017,7.84762505828644,7.984940478531));
#12275=CARTESIAN_POINT('Ctrl Pts',(19.3059540467289,7.82505223561007,8.0330801379758));
#12276=CARTESIAN_POINT('Ctrl Pts',(19.3308135357918,7.80337034833451,8.07931975472781));
#12277=CARTESIAN_POINT('Ctrl Pts',(19.3565869534279,7.78330843074937,8.1258946220068));
#12278=CARTESIAN_POINT('Ctrl Pts',(19.3833004152209,7.76513667663444,8.17270481742561));
#12279=CARTESIAN_POINT('Ctrl Pts',(19.3884266184092,7.76164959193525,8.18168750094523));
#12280=CARTESIAN_POINT('Ctrl Pts',(19.3935874341475,7.75823224575957,8.19067877697312));
#12281=CARTESIAN_POINT('Ctrl Pts',(19.3987830406924,7.75488674445212,8.19967783148497));
#12282=CARTESIAN_POINT('Origin',(-8.09752352946369,25.4,24.0746778314847));
#12283=CARTESIAN_POINT('',(-3.19820054762209,-21.9,20.0349830014761));
#12284=CARTESIAN_POINT('Ctrl Pts',(-6.07314264709777,-23.4,18.0560083736135));
#12285=CARTESIAN_POINT('Ctrl Pts',(-5.92577312631869,-23.3035563481381,
18.1055761464572));
#12286=CARTESIAN_POINT('Ctrl Pts',(-5.7799969640134,-23.2068396384742,18.1605585901307));
#12287=CARTESIAN_POINT('Ctrl Pts',(-5.63584724081203,-23.1112816984186,
18.2211313626838));
#12288=CARTESIAN_POINT('Ctrl Pts',(-5.4996399026027,-23.0209888253512,18.2783666867219));
#12289=CARTESIAN_POINT('Ctrl Pts',(-5.36488465057871,-22.9317288900636,
18.3405935419584));
#12290=CARTESIAN_POINT('Ctrl Pts',(-5.23162378740032,-22.8447237863145,
18.4079990150367));
#12291=CARTESIAN_POINT('Ctrl Pts',(-5.11018575539893,-22.7654377279672,
18.4694243112679));
#12292=CARTESIAN_POINT('Ctrl Pts',(-4.98998879405928,-22.688023392779,18.5351504504473));
#12293=CARTESIAN_POINT('Ctrl Pts',(-4.87107687669821,-22.6134330617646,
18.6053477651812));
#12294=CARTESIAN_POINT('Ctrl Pts',(-4.7689939559047,-22.5493991194829,18.6656104123483));
#12295=CARTESIAN_POINT('Ctrl Pts',(-4.66785825008194,-22.4874464633674,
18.7291686243386));
#12296=CARTESIAN_POINT('Ctrl Pts',(-4.56770501518154,-22.4282022173721,
18.7961472317784));
#12297=CARTESIAN_POINT('Ctrl Pts',(-4.56256237874832,-22.4251601626824,
18.7995864279981));
#12298=CARTESIAN_POINT('Ctrl Pts',(-4.55742243042036,-22.4221253454027,
18.8030345816224));
#12299=CARTESIAN_POINT('Ctrl Pts',(-4.55228516675424,-22.4190978469188,
18.8064917154177));
#12300=CARTESIAN_POINT('Ctrl Pts',(-4.46260907364606,-22.36624982245,18.8668394554341));
#12301=CARTESIAN_POINT('Ctrl Pts',(-4.37352988347701,-22.3154805384071,
18.9300739413651));
#12302=CARTESIAN_POINT('Ctrl Pts',(-4.28501205257774,-22.2675991945448,
18.9965176621394));
#12303=CARTESIAN_POINT('Ctrl Pts',(-4.20330452989676,-22.223401704052,19.0578493934644));
#12304=CARTESIAN_POINT('Ctrl Pts',(-4.12207540156842,-22.1816645410681,
19.1219155883572));
#12305=CARTESIAN_POINT('Ctrl Pts',(-4.04130255733465,-22.1430604940879,
19.188992872892));
#12306=CARTESIAN_POINT('Ctrl Pts',(-3.98048878468141,-22.113995555756,19.2394952759037));
#12307=CARTESIAN_POINT('Ctrl Pts',(-3.91993377873524,-22.0867072848434,
19.2917049539104));
#12308=CARTESIAN_POINT('Ctrl Pts',(-3.85963012170325,-22.0614998943553,
19.3457496099721));
#12309=CARTESIAN_POINT('Ctrl Pts',(-3.85554403175164,-22.0597918774613,
19.3494115989283));
#12310=CARTESIAN_POINT('Ctrl Pts',(-3.85145977887563,-22.0580937292924,
19.3530814045083));
#12311=CARTESIAN_POINT('Ctrl Pts',(-3.84737735665805,-22.0564055371509,
19.3567590624002));
#12312=CARTESIAN_POINT('Ctrl Pts',(-3.77236645160972,-22.0253864965719,
19.4243327802147));
#12313=CARTESIAN_POINT('Ctrl Pts',(-3.69866349853912,-21.997880025637,19.493924344581));
#12314=CARTESIAN_POINT('Ctrl Pts',(-3.62619987237413,-21.9749039650179,
19.5657626286246));
#12315=CARTESIAN_POINT('Ctrl Pts',(-3.55790342605073,-21.9532491931849,
19.6334696944975));
#12316=CARTESIAN_POINT('Ctrl Pts',(-3.49070795830701,-21.9356181609376,
19.7031724954035));
#12317=CARTESIAN_POINT('Ctrl Pts',(-3.42456389553437,-21.9229055031068,
19.7750775735084));
#12318=CARTESIAN_POINT('Ctrl Pts',(-3.36249546381872,-21.9109761673294,
19.8425520412577));
#12319=CARTESIAN_POINT('Ctrl Pts',(-3.30135293266074,-21.9033774739789,
19.9119657700143));
#12320=CARTESIAN_POINT('Ctrl Pts',(-3.24110133014448,-21.9008931019147,
19.9835028624463));
#12321=CARTESIAN_POINT('Ctrl Pts',(-3.22675064343828,-21.900301375825,20.0005415196519));
#12322=CARTESIAN_POINT('Ctrl Pts',(-3.21245052416384,-21.9000000019656,
20.017700696624));
#12323=CARTESIAN_POINT('Ctrl Pts',(-3.19820054762209,-21.9,20.0349830014761));
#12324=CARTESIAN_POINT('Origin',(-8.09752352946369,-21.9,24.0746778314847));
#12325=CARTESIAN_POINT('Ctrl Pts',(-2.59826221543248,7.75488674445211,20.8996778314848));
#12326=CARTESIAN_POINT('Ctrl Pts',(-2.63105191627123,7.77600035063574,20.8428844036671));
#12327=CARTESIAN_POINT('Ctrl Pts',(-2.66398834136481,7.79969631459274,20.7878476354939));
#12328=CARTESIAN_POINT('Ctrl Pts',(-2.69705567354774,7.82564845388557,20.7343753409493));
#12329=CARTESIAN_POINT('Ctrl Pts',(-2.73094311438655,7.85224423669808,20.6795768707287));
#12330=CARTESIAN_POINT('Ctrl Pts',(-2.76496806068104,7.88120973564853,20.6264215211099));
#12331=CARTESIAN_POINT('Ctrl Pts',(-2.7991214779807,7.91224591463994,20.574721955647));
#12332=CARTESIAN_POINT('Ctrl Pts',(-2.83464656562271,7.94452856937605,20.5209460310299));
#12333=CARTESIAN_POINT('Ctrl Pts',(-2.87031065788748,7.97905171375511,20.4687452183232));
#12334=CARTESIAN_POINT('Ctrl Pts',(-2.90611190620181,8.01553158397781,20.4179286049906));
#12335=CARTESIAN_POINT('Ctrl Pts',(-2.92551405397642,8.03530150447458,20.3903890222189));
#12336=CARTESIAN_POINT('Ctrl Pts',(-2.9449566253594,8.05564699924486,20.3632563129462));
#12337=CARTESIAN_POINT('Ctrl Pts',(-2.9644402707131,8.07652873453461,20.3365023060375));
#12338=CARTESIAN_POINT('Ctrl Pts',(-2.98991627136349,8.1038328191741,20.3015198843688));
#12339=CARTESIAN_POINT('Ctrl Pts',(-3.01546265394331,8.13206076164095,20.2671874911136));
#12340=CARTESIAN_POINT('Ctrl Pts',(-3.04108539386802,8.16115913750231,20.2334547288528));
#12341=CARTESIAN_POINT('Ctrl Pts',(-3.08652949487372,8.21276757343192,20.1736268158392));
#12342=CARTESIAN_POINT('Ctrl Pts',(-3.13203636606265,8.26690043734288,20.1159177783991));
#12343=CARTESIAN_POINT('Ctrl Pts',(-3.17755524682584,8.32314897455742,20.0601342793104));
#12344=CARTESIAN_POINT('Ctrl Pts',(-3.22432195048657,8.38093946999923,20.0028215702257));
#12345=CARTESIAN_POINT('Ctrl Pts',(-3.27110133080977,8.4409633324214,19.9475414687676));
#12346=CARTESIAN_POINT('Ctrl Pts',(-3.31784550357409,8.50282830731164,19.8941035216878));
#12347=CARTESIAN_POINT('Ctrl Pts',(-3.33340086872185,8.52341552101904,19.8763206253306));
#12348=CARTESIAN_POINT('Ctrl Pts',(-3.3489523924956,8.54420702222892,19.8587418804176));
#12349=CARTESIAN_POINT('Ctrl Pts',(-3.36449847946483,8.56518952756249,19.8413607070121));
#12350=CARTESIAN_POINT('Ctrl Pts',(-3.40691236619082,8.62243541884093,19.7939402132604));
#12351=CARTESIAN_POINT('Ctrl Pts',(-3.44924177893934,8.68106595956033,19.7480604763911));
#12352=CARTESIAN_POINT('Ctrl Pts',(-3.49136596676808,8.74069382312879,19.7036770461595));
#12353=CARTESIAN_POINT('Ctrl Pts',(-3.53509055502149,8.80258709436672,19.6576073813855));
#12354=CARTESIAN_POINT('Ctrl Pts',(-3.57869061706342,8.86568736322834,19.6130478678103));
#12355=CARTESIAN_POINT('Ctrl Pts',(-3.62207808072827,8.92967013781227,19.5699382005166));
#12356=CARTESIAN_POINT('Ctrl Pts',(-3.66755511856297,8.99673437284105,19.5247523379434));
#12357=CARTESIAN_POINT('Ctrl Pts',(-3.71279869458657,9.06476837723555,19.4811592322964));
#12358=CARTESIAN_POINT('Ctrl Pts',(-3.75772475960894,9.13345255195358,19.439094912377));
#12359=CARTESIAN_POINT('Ctrl Pts',(-3.76851341939143,9.14994654476389,19.4289934793589));
#12360=CARTESIAN_POINT('Ctrl Pts',(-3.77928383976051,9.16647825760466,19.4189802368632));
#12361=CARTESIAN_POINT('Ctrl Pts',(-3.7900349850261,9.18304367617654,19.4090543533692));
#12362=CARTESIAN_POINT('Ctrl Pts',(-3.84338762762093,9.26524969559742,19.3597970787797));
#12363=CARTESIAN_POINT('Ctrl Pts',(-3.89641623100928,9.34848879466418,19.312519437982));
#12364=CARTESIAN_POINT('Ctrl Pts',(-3.94920298987383,9.43264075175752,19.2669688773235));
#12365=CARTESIAN_POINT('Ctrl Pts',(-4.00465670938737,9.52104434245995,19.2191169525459));
#12366=CARTESIAN_POINT('Ctrl Pts',(-4.05984349679059,9.61045552747327,19.1731710962252));
#12367=CARTESIAN_POINT('Ctrl Pts',(-4.11486175771081,9.7007827075446,19.1288726481045));
#12368=CARTESIAN_POINT('Ctrl Pts',(-4.15207724766588,9.76188188091706,19.0989082613083));
#12369=CARTESIAN_POINT('Ctrl Pts',(-4.18921569512279,9.82340116495859,19.0696983544146));
#12370=CARTESIAN_POINT('Ctrl Pts',(-4.2263084128575,9.88532296597213,19.0411707518213));
#12371=CARTESIAN_POINT('Ctrl Pts',(-4.27111143173269,9.96011618116432,19.0067132411425));
#12372=CARTESIAN_POINT('Ctrl Pts',(-4.31584768219754,10.0354996811099,18.9732530327533));
#12373=CARTESIAN_POINT('Ctrl Pts',(-4.36057769144337,10.111478019192,18.940692114664));
#12374=CARTESIAN_POINT('Ctrl Pts',(-4.42892061974248,10.2275652322147,18.8909423263709));
#12375=CARTESIAN_POINT('Ctrl Pts',(-4.49710627109395,10.3447938290632,18.8433951049612));
#12376=CARTESIAN_POINT('Ctrl Pts',(-4.56524407243742,10.4630236268316,18.7977890095272));
#12377=CARTESIAN_POINT('Ctrl Pts',(-4.6012713099202,10.5255365479672,18.7736752048774));
#12378=CARTESIAN_POINT('Ctrl Pts',(-4.63728521548576,10.5883301347704,18.7501046160461));
#12379=CARTESIAN_POINT('Ctrl Pts',(-4.67330231315613,10.6513883422586,18.7270419929154));
#12380=CARTESIAN_POINT('Ctrl Pts',(-4.74222702829795,10.7720607248103,18.6829078224097));
#12381=CARTESIAN_POINT('Ctrl Pts',(-4.81115906209138,10.8936995222528,18.6406488353005));
#12382=CARTESIAN_POINT('Ctrl Pts',(-4.88008076708229,11.0159833665814,18.600143147662));
#12383=CARTESIAN_POINT('Ctrl Pts',(-4.95506354104002,11.149021019367,18.5560753344731));
#12384=CARTESIAN_POINT('Ctrl Pts',(-5.03003423681176,11.2828228206758,18.5140824431372));
#12385=CARTESIAN_POINT('Ctrl Pts',(-5.10498353721246,11.4170275976618,18.4740347519827));
#12386=CARTESIAN_POINT('Ctrl Pts',(-5.11363857299637,11.4325253693685,18.469410103078));
#12387=CARTESIAN_POINT('Ctrl Pts',(-5.12229333534976,11.4480285606925,18.4648114245623));
#12388=CARTESIAN_POINT('Ctrl Pts',(-5.1309478185836,11.4635366486365,18.4602385405353));
#12389=CARTESIAN_POINT('Ctrl Pts',(-5.15787112219279,11.5117808879322,18.4460127177216));
#12390=CARTESIAN_POINT('Ctrl Pts',(-5.18480476071166,11.5600961433554,18.4320245655294));
#12391=CARTESIAN_POINT('Ctrl Pts',(-5.21175836363394,11.6084844905159,18.4182667149329));
#12392=CARTESIAN_POINT('Ctrl Pts',(-5.31258723548669,11.7894971168827,18.3668009217045));
#12393=CARTESIAN_POINT('Ctrl Pts',(-5.41362677762227,11.9714205665464,18.3185921383772));
#12394=CARTESIAN_POINT('Ctrl Pts',(-5.5150898962066,12.1538289711062,18.2734105472006));
#12395=CARTESIAN_POINT('Ctrl Pts',(-5.55642235325627,12.2281356517223,18.2550051778132));
#12396=CARTESIAN_POINT('Ctrl Pts',(-5.59782488816878,12.3025233025885,18.2371024570184));
#12397=CARTESIAN_POINT('Ctrl Pts',(-5.6393109798215,12.3769650887378,18.2196880081847));
#12398=CARTESIAN_POINT('Ctrl Pts',(-5.71720894883317,12.5167435956931,18.1869890929205));
#12399=CARTESIAN_POINT('Ctrl Pts',(-5.79563339295387,12.6571275036336,18.1559192636753));
#12400=CARTESIAN_POINT('Ctrl Pts',(-5.87434573391953,12.7973698711455,18.1265260513586));
#12401=CARTESIAN_POINT('Ctrl Pts',(-5.94045812878175,12.915162820302,18.1018379829425));
#12402=CARTESIAN_POINT('Ctrl Pts',(-6.00677355328274,13.0328551936566,18.0783316338689));
#12403=CARTESIAN_POINT('Ctrl Pts',(-6.07314264709777,13.15,18.0560083736135));
#12404=CARTESIAN_POINT('Origin',(-16.8005208252602,25.4,19.05));
#12405=CARTESIAN_POINT('',(-15.7517039698567,-21.9,12.7872144213759));
#12406=CARTESIAN_POINT('Origin',(-16.8005208252602,-21.9,19.05));
#12407=CARTESIAN_POINT('Ctrl Pts',(-15.7517039698567,-21.9,12.7872144213759));
#12408=CARTESIAN_POINT('Ctrl Pts',(-15.6577766387567,-21.9000000083571,
12.8029442538608));
#12409=CARTESIAN_POINT('Ctrl Pts',(-15.5653228653555,-21.9054435048675,
12.8205709182498));
#12410=CARTESIAN_POINT('Ctrl Pts',(-15.4741566469411,-21.9155046710518,
12.8400273794258));
#12411=CARTESIAN_POINT('Ctrl Pts',(-15.3788825965547,-21.9260191803806,
12.8603605235955));
#12412=CARTESIAN_POINT('Ctrl Pts',(-15.2850148000878,-21.9415773497208,
12.8826920382101));
#12413=CARTESIAN_POINT('Ctrl Pts',(-15.192351675936,-21.9612924551078,12.9069597851924));
#12414=CARTESIAN_POINT('Ctrl Pts',(-15.0919530360919,-21.9826533770858,
12.9332534031922));
#12415=CARTESIAN_POINT('Ctrl Pts',(-14.9929686181069,-22.008894721178,12.961819870374));
#12416=CARTESIAN_POINT('Ctrl Pts',(-14.895153818191,-22.0389456239473,12.9925982857732));
#12417=CARTESIAN_POINT('Ctrl Pts',(-14.8766466516217,-22.0446314410586,
12.9984217527846));
#12418=CARTESIAN_POINT('Ctrl Pts',(-14.8581813868158,-22.0504537744583,
13.0043244573537));
#12419=CARTESIAN_POINT('Ctrl Pts',(-14.839756407874,-22.0564055499457,13.0103060589621));
#12420=CARTESIAN_POINT('Ctrl Pts',(-14.8345259500896,-22.0580951318186,
13.0120041078334));
#12421=CARTESIAN_POINT('Ctrl Pts',(-14.8293013868339,-22.0597946861619,
13.0137076773778));
#12422=CARTESIAN_POINT('Ctrl Pts',(-14.8240826839043,-22.0615041254602,
13.0154167552805));
#12423=CARTESIAN_POINT('Ctrl Pts',(-14.7228347907064,-22.0946689041117,
13.0485745225054));
#12424=CARTESIAN_POINT('Ctrl Pts',(-14.6241194589298,-22.1314339084946,
13.0836965866196));
#12425=CARTESIAN_POINT('Ctrl Pts',(-14.5276787480026,-22.1711120177115,
13.1206542613819));
#12426=CARTESIAN_POINT('Ctrl Pts',(-14.423784232686,-22.213856807605,13.1604683572107));
#12427=CARTESIAN_POINT('Ctrl Pts',(-14.3225295566706,-22.259982703488,13.2024126657374));
#12428=CARTESIAN_POINT('Ctrl Pts',(-14.2236159096512,-22.3086850460529,
13.2463478400349));
#12429=CARTESIAN_POINT('Ctrl Pts',(-14.1514528009381,-22.3442161638206,
13.2784010385034));
#12430=CARTESIAN_POINT('Ctrl Pts',(-14.0805362301013,-22.3811198321414,
13.3115143518381));
#12431=CARTESIAN_POINT('Ctrl Pts',(-14.0107570059122,-22.4190978671501,
13.3456404536346));
#12432=CARTESIAN_POINT('Ctrl Pts',(-14.0051868812153,-22.4221294627747,
13.348364568794));
#12433=CARTESIAN_POINT('Ctrl Pts',(-13.9996232086063,-22.4251683970665,
13.351095517512));
#12434=CARTESIAN_POINT('Ctrl Pts',(-13.9940659665539,-22.4282145883132,
13.3538332913571));
#12435=CARTESIAN_POINT('Ctrl Pts',(-13.8353383484615,-22.5152208184325,
13.4320304109373));
#12436=CARTESIAN_POINT('Ctrl Pts',(-13.6817400381253,-22.6081793607658,
13.5158520921216));
#12437=CARTESIAN_POINT('Ctrl Pts',(-13.5331922899877,-22.7050300063637,
13.6049382184845));
#12438=CARTESIAN_POINT('Ctrl Pts',(-13.3831027231072,-22.8028858919771,
13.6949489947399));
#12439=CARTESIAN_POINT('Ctrl Pts',(-13.2381692424498,-22.904715210645,13.7903339482295));
#12440=CARTESIAN_POINT('Ctrl Pts',(-13.098312889361,-23.0084452538252,13.890732869345));
#12441=CARTESIAN_POINT('Ctrl Pts',(-12.9560181195809,-23.1139838460137,
13.9928822608513));
#12442=CARTESIAN_POINT('Ctrl Pts',(-12.8189790827752,-23.2214901219724,
14.1002219147977));
#12443=CARTESIAN_POINT('Ctrl Pts',(-12.687113670909,-23.3288332609408,14.2123853779174));
#12444=CARTESIAN_POINT('Ctrl Pts',(-12.6579532757914,-23.3525708605219,
14.2371889322083));
#12445=CARTESIAN_POINT('Ctrl Pts',(-12.6290458846788,-23.3763006781133,
14.2622284310387));
#12446=CARTESIAN_POINT('Ctrl Pts',(-12.6003906189451,-23.4,14.2875));
#12447=CARTESIAN_POINT('Ctrl Pts',(-12.6003906189451,13.15,14.2875));
#12448=CARTESIAN_POINT('Ctrl Pts',(-12.6805660239936,12.9711603489454,14.2167919389926));
#12449=CARTESIAN_POINT('Ctrl Pts',(-12.7625477505346,12.7922384038523,14.1480629070756));
#12450=CARTESIAN_POINT('Ctrl Pts',(-12.8465546744841,12.6135684732185,14.081202835174));
#12451=CARTESIAN_POINT('Ctrl Pts',(-12.9256696150891,12.4453030459724,14.0182362323196));
#12452=CARTESIAN_POINT('Ctrl Pts',(-13.0065809833159,12.2772593411672,13.9569274305183));
#12453=CARTESIAN_POINT('Ctrl Pts',(-13.0895011854204,12.1097298658262,13.8972149709292));
#12454=CARTESIAN_POINT('Ctrl Pts',(-13.1664953235755,11.95417323135,13.8417699859134));
#12455=CARTESIAN_POINT('Ctrl Pts',(-13.2452216484674,11.7990589433282,13.787701522798));
#12456=CARTESIAN_POINT('Ctrl Pts',(-13.3258732912857,11.6446516999771,13.7349847981691));
#12457=CARTESIAN_POINT('Ctrl Pts',(-13.3320808650622,11.6327673251369,13.7309273116015));
#12458=CARTESIAN_POINT('Ctrl Pts',(-13.3382998557066,11.620887159043,13.7268778447985));
#12459=CARTESIAN_POINT('Ctrl Pts',(-13.34453035693,11.6090113330868,13.7228363925281));
#12460=CARTESIAN_POINT('Ctrl Pts',(-13.3701748672856,11.5601308769568,13.7062019259122));
#12461=CARTESIAN_POINT('Ctrl Pts',(-13.3960120894246,11.5113297193656,13.6897046928704));
#12462=CARTESIAN_POINT('Ctrl Pts',(-13.4220479527771,11.4626185033485,13.673344808347));
#12463=CARTESIAN_POINT('Ctrl Pts',(-13.5007574197068,11.3153587872303,13.62388695967));
#12464=CARTESIAN_POINT('Ctrl Pts',(-13.5812593458259,11.1688712790712,13.5756551364999));
#12465=CARTESIAN_POINT('Ctrl Pts',(-13.6638980075716,11.0233411942463,13.528670711557));
#12466=CARTESIAN_POINT('Ctrl Pts',(-13.7433621196739,10.8834016220112,13.4834911850273));
#12467=CARTESIAN_POINT('Ctrl Pts',(-13.8248017421929,10.7443469553863,13.4394651524236));
#12468=CARTESIAN_POINT('Ctrl Pts',(-13.9085483061395,10.6063775973624,13.3966301736711));
#12469=CARTESIAN_POINT('Ctrl Pts',(-13.9882575070387,10.4750596452175,13.3558602391689));
#12470=CARTESIAN_POINT('Ctrl Pts',(-14.0700564394539,10.3447246751962,13.3161693909074));
#12471=CARTESIAN_POINT('Ctrl Pts',(-14.1542566954101,10.2155824310125,13.2776057275986));
#12472=CARTESIAN_POINT('Ctrl Pts',(-14.1759224559351,10.1823525446615,13.2676828231522));
#12473=CARTESIAN_POINT('Ctrl Pts',(-14.1977473522222,10.1492018356285,13.257834629348));
#12474=CARTESIAN_POINT('Ctrl Pts',(-14.2197370070741,10.1161343255489,13.2480621331828));
#12475=CARTESIAN_POINT('Ctrl Pts',(-14.2697134783846,10.0409809190981,13.2258519221759));
#12476=CARTESIAN_POINT('Ctrl Pts',(-14.3205483943213,9.96626705526651,13.2040289854677));
#12477=CARTESIAN_POINT('Ctrl Pts',(-14.3723283486023,9.89202045142466,13.1826001246522));
#12478=CARTESIAN_POINT('Ctrl Pts',(-14.4424863663332,9.79142178112592,13.1535655992665));
#12479=CARTESIAN_POINT('Ctrl Pts',(-14.5143906000105,9.69169193895732,13.1252666892286));
#12480=CARTESIAN_POINT('Ctrl Pts',(-14.5883378176581,9.59300570027429,13.0977807866605));
#12481=CARTESIAN_POINT('Ctrl Pts',(-14.635359051831,9.53025352532599,13.0803031708391));
#12482=CARTESIAN_POINT('Ctrl Pts',(-14.683206840735,9.46792401681048,13.063154611628));
#12483=CARTESIAN_POINT('Ctrl Pts',(-14.7319636287996,9.40607058542615,13.0463587156065));
#12484=CARTESIAN_POINT('Ctrl Pts',(-14.7902864685227,9.33208154906526,13.0262674751751));
#12485=CARTESIAN_POINT('Ctrl Pts',(-14.8499317227244,9.25875668204221,13.0066727912773));
#12486=CARTESIAN_POINT('Ctrl Pts',(-14.9110746531334,9.18618721050011,12.9876165443994));
#12487=CARTESIAN_POINT('Ctrl Pts',(-14.976144264209,9.10895723055615,12.9673364798914));
#12488=CARTESIAN_POINT('Ctrl Pts',(-15.0425927400042,9.03297713418422,12.9477720512664));
#12489=CARTESIAN_POINT('Ctrl Pts',(-15.1105485368423,8.95848778473299,12.9290087698698));
#12490=CARTESIAN_POINT('Ctrl Pts',(-15.1780277686271,8.88452081927902,12.9103770728945));
#12491=CARTESIAN_POINT('Ctrl Pts',(-15.2469932190871,8.81202334049308,12.892535211434));
#12492=CARTESIAN_POINT('Ctrl Pts',(-15.3175799579227,8.74127840230462,12.8755833064032));
#12493=CARTESIAN_POINT('Ctrl Pts',(-15.3761704880966,8.68255655874077,12.8615123758064));
#12494=CARTESIAN_POINT('Ctrl Pts',(-15.4358982963745,8.62503122998396,12.8480495581956));
#12495=CARTESIAN_POINT('Ctrl Pts',(-15.496892027902,8.56885520307108,12.8352552780477));
#12496=CARTESIAN_POINT('Ctrl Pts',(-15.5571381099264,8.51336777115895,12.8226178277404));
#12497=CARTESIAN_POINT('Ctrl Pts',(-15.6186470139557,8.45914957374164,12.8106203083913));
#12498=CARTESIAN_POINT('Ctrl Pts',(-15.6816035368458,8.40640557244853,12.7993457937111));
#12499=CARTESIAN_POINT('Ctrl Pts',(-15.7419197422832,8.35587358828636,12.7885441180079));
#12500=CARTESIAN_POINT('Ctrl Pts',(-15.8035646398897,8.30669462478942,12.7784060513894));
#12501=CARTESIAN_POINT('Ctrl Pts',(-15.8667156307491,8.25909114269656,12.7690197747266));
#12502=CARTESIAN_POINT('Ctrl Pts',(-15.9083560624209,8.22770241044624,12.762830661829));
#12503=CARTESIAN_POINT('Ctrl Pts',(-15.9506516151452,8.19699952044147,12.7569687178741));
#12504=CARTESIAN_POINT('Ctrl Pts',(-15.9936571257441,8.1670574358422,12.7514631752544));
#12505=CARTESIAN_POINT('Ctrl Pts',(-16.0374647365421,8.13655689834508,12.7458549481933));
#12506=CARTESIAN_POINT('Ctrl Pts',(-16.0819818772239,8.10686980879577,12.7406197777735));
#12507=CARTESIAN_POINT('Ctrl Pts',(-16.1272992232855,8.07806532466692,12.7357880400415));
#12508=CARTESIAN_POINT('Ctrl Pts',(-16.1796232807136,8.04480725435319,12.7302092463888));
#12509=CARTESIAN_POINT('Ctrl Pts',(-16.2330200573025,8.01279246823339,12.7251928706675));
#12510=CARTESIAN_POINT('Ctrl Pts',(-16.2874537728527,7.98223072788154,12.7207964614722));
#12511=CARTESIAN_POINT('Ctrl Pts',(-16.3401547757431,7.95264181684838,12.7165399970481));
#12512=CARTESIAN_POINT('Ctrl Pts',(-16.3938280311525,7.92441470275639,12.7128646355283));
#12513=CARTESIAN_POINT('Ctrl Pts',(-16.44842648929,7.89778233069164,12.7098341952403));
#12514=CARTESIAN_POINT('Ctrl Pts',(-16.5013769362388,7.87195383567105,12.7068952263907));
#12515=CARTESIAN_POINT('Ctrl Pts',(-16.5551978274457,7.84762505829446,12.7045628094629));
#12516=CARTESIAN_POINT('Ctrl Pts',(-16.6098284934653,7.82505223561866,12.7029065797752));
#12517=CARTESIAN_POINT('Ctrl Pts',(-16.6623029207626,7.80337034834364,12.7013157204526));
#12518=CARTESIAN_POINT('Ctrl Pts',(-16.7155246478195,7.78330843075896,12.7003487212281));
#12519=CARTESIAN_POINT('Ctrl Pts',(-16.7694201971022,7.76513667664443,12.7000781600543));
#12520=CARTESIAN_POINT('Ctrl Pts',(-16.7797625308285,7.76164959194177,12.7000262404804));
#12521=CARTESIAN_POINT('Ctrl Pts',(-16.7901296121603,7.75823224576275,12.7));
#12522=CARTESIAN_POINT('Ctrl Pts',(-16.8005208252602,7.75488674445212,12.7));
#12523=CARTESIAN_POINT('Origin',(0.,-23.4,0.));
#12524=CARTESIAN_POINT('Ctrl Pts',(-6.07314264709753,-23.4,-18.0560083736136));
#12525=CARTESIAN_POINT('Ctrl Pts',(-5.88858797454276,-23.3670436986155,
-18.1180833809697));
#12526=CARTESIAN_POINT('Ctrl Pts',(-5.70415854699224,-23.3340202714534,
-18.1802846951814));
#12527=CARTESIAN_POINT('Ctrl Pts',(-5.51977350812678,-23.3013555121265,
-18.2428536513247));
#12528=CARTESIAN_POINT('Ctrl Pts',(-5.37004319496178,-23.2748300159497,
-18.2936629222688));
#12529=CARTESIAN_POINT('Ctrl Pts',(-5.22034041400646,-23.2485394306939,
-18.3447134083939));
#12530=CARTESIAN_POINT('Ctrl Pts',(-5.07065077098291,-23.2227118266261,
-18.3961284339486));
#12531=CARTESIAN_POINT('Ctrl Pts',(-4.93247587122431,-23.1988709881352,
-18.4435884041817));
#12532=CARTESIAN_POINT('Ctrl Pts',(-4.79431122189726,-23.175423671515,-18.4913586401195));
#12533=CARTESIAN_POINT('Ctrl Pts',(-4.65618933923002,-23.1525653653545,
-18.5395394451827));
#12534=CARTESIAN_POINT('Ctrl Pts',(-4.53506332264139,-23.1325197685401,
-18.5817916132));
#12535=CARTESIAN_POINT('Ctrl Pts',(-4.41397019874696,-23.1129267585465,
-18.6243594808228));
#12536=CARTESIAN_POINT('Ctrl Pts',(-4.2929717674843,-23.0939393203888,-18.6673155065398));
#12537=CARTESIAN_POINT('Ctrl Pts',(-4.27599380361344,-23.0912750871779,
-18.67334290578));
#12538=CARTESIAN_POINT('Ctrl Pts',(-4.25901777583649,-23.0886228201603,
-18.6793779562881));
#12539=CARTESIAN_POINT('Ctrl Pts',(-4.24204392806113,-23.0859829876026,
-18.6854208674118));
#12540=CARTESIAN_POINT('Ctrl Pts',(-4.21403849285808,-23.0816274837345,
-18.6953911674966));
#12541=CARTESIAN_POINT('Ctrl Pts',(-4.18604700646962,-23.0773075842939,
-18.7053795884347));
#12542=CARTESIAN_POINT('Ctrl Pts',(-4.15807096333259,-23.0730255541513,
-18.7153867564022));
#12543=CARTESIAN_POINT('Ctrl Pts',(-4.04200724753667,-23.0552607713668,
-18.7569033173116));
#12544=CARTESIAN_POINT('Ctrl Pts',(-3.92593006481832,-23.0380976121148,
-18.7988741217285));
#12545=CARTESIAN_POINT('Ctrl Pts',(-3.80990120850084,-23.0218415529602,
-18.8414809578007));
#12546=CARTESIAN_POINT('Ctrl Pts',(-3.70072977930051,-23.0065462439535,
-18.8815696851685));
#12547=CARTESIAN_POINT('Ctrl Pts',(-3.59160104576938,-22.9920537993331,
-18.9222214064209));
#12548=CARTESIAN_POINT('Ctrl Pts',(-3.48259310512416,-22.9786542884005,
-18.963599792128));
#12549=CARTESIAN_POINT('Ctrl Pts',(-3.43157384280193,-22.9723828813891,
-18.982966222705));
#12550=CARTESIAN_POINT('Ctrl Pts',(-3.38058144102074,-22.9663514277305,
-19.0024920199359));
#12551=CARTESIAN_POINT('Ctrl Pts',(-3.32962618541098,-22.9605927752761,
-19.0221950481898));
#12552=CARTESIAN_POINT('Ctrl Pts',(-3.30407684920651,-22.9577053450026,
-19.0320742900282));
#12553=CARTESIAN_POINT('Ctrl Pts',(-3.27849980805422,-22.9548823672324,
-19.0420123529479));
#12554=CARTESIAN_POINT('Ctrl Pts',(-3.2528923075186,-22.9521283805007,-19.052013666249));
#12555=CARTESIAN_POINT('Ctrl Pts',(-3.17837177385048,-22.9441139879725,
-19.0811185452486));
#12556=CARTESIAN_POINT('Ctrl Pts',(-3.10413037938078,-22.9367118504462,
-19.1105498162239));
#12557=CARTESIAN_POINT('Ctrl Pts',(-3.03010916781498,-22.9301299080702,
-19.1404318150206));
#12558=CARTESIAN_POINT('Ctrl Pts',(-2.95870293024803,-22.9237804883428,
-19.1692581616841));
#12559=CARTESIAN_POINT('Ctrl Pts',(-2.88750160968762,-22.9181939831414,
-19.1985038155338));
#12560=CARTESIAN_POINT('Ctrl Pts',(-2.81647463478462,-22.9135965970107,
-19.2282900937695));
#12561=CARTESIAN_POINT('Ctrl Pts',(-2.74923181322827,-22.9092441490057,
-19.2564894278248));
#12562=CARTESIAN_POINT('Ctrl Pts',(-2.68214533086182,-22.9057780702214,
-19.2851732366577));
#12563=CARTESIAN_POINT('Ctrl Pts',(-2.61520888367674,-22.903429789029,-19.3144547693357));
#12564=CARTESIAN_POINT('Ctrl Pts',(-2.55222036166138,-22.9012200099355,
-19.3420092713043));
#12565=CARTESIAN_POINT('Ctrl Pts',(-2.48936478214343,-22.9,-19.3700930276043));
#12566=CARTESIAN_POINT('Ctrl Pts',(-2.42665362134758,-22.9,-19.3988105873015));
#12567=CARTESIAN_POINT('Ctrl Pts',(18.0131895824795,-22.9,-7.59786161137808));
#12568=CARTESIAN_POINT('Ctrl Pts',(18.0202404656926,-22.9,-7.52320647355465));
#12569=CARTESIAN_POINT('Ctrl Pts',(18.028025155963,-22.9014413252167,-7.44877824034678));
#12570=CARTESIAN_POINT('Ctrl Pts',(18.0364209165634,-22.9040302787143,-7.37452199635976));
#12571=CARTESIAN_POINT('Ctrl Pts',(18.0449193548697,-22.9066508943588,-7.2993576201457));
#12572=CARTESIAN_POINT('Ctrl Pts',(18.0540441011123,-22.9104479219793,-7.22436948480864));
#12573=CARTESIAN_POINT('Ctrl Pts',(18.063691899772,-22.9151689742966,-7.14948735848897));
#12574=CARTESIAN_POINT('Ctrl Pts',(18.0738958528035,-22.9201621751089,-7.07028859752707));
#12575=CARTESIAN_POINT('Ctrl Pts',(18.0846849419657,-22.9261892251373,-6.99120855793443));
#12576=CARTESIAN_POINT('Ctrl Pts',(18.0959620640515,-22.9330040852343,-6.91214802540154));
#12577=CARTESIAN_POINT('Ctrl Pts',(18.1056234232792,-22.9388425261932,-6.844415123362));
#12578=CARTESIAN_POINT('Ctrl Pts',(18.1156434929245,-22.9452603057859,-6.77669626729572));
#12579=CARTESIAN_POINT('Ctrl Pts',(18.1259739820853,-22.9521283804573,-6.70891945900388));
#12580=CARTESIAN_POINT('Ctrl Pts',(18.1301164636466,-22.9548824487541,-6.68174125144072));
#12581=CARTESIAN_POINT('Ctrl Pts',(18.1342984943433,-22.9577055122081,-6.65462105077966));
#12582=CARTESIAN_POINT('Ctrl Pts',(18.1385176153026,-22.960593031896,-6.62755425650044));
#12583=CARTESIAN_POINT('Ctrl Pts',(18.1564082194725,-22.9728371633794,-6.51278122504063));
#12584=CARTESIAN_POINT('Ctrl Pts',(18.175074850113,-22.9863118482887,-6.39826461568774));
#12585=CARTESIAN_POINT('Ctrl Pts',(18.1943268007347,-23.0007124806144,-6.28399909928586));
#12586=CARTESIAN_POINT('Ctrl Pts',(18.2147324024488,-23.0159760543397,-6.16288635267795));
#12587=CARTESIAN_POINT('Ctrl Pts',(18.235795699568,-23.032280074281,-6.04205565211729));
#12588=CARTESIAN_POINT('Ctrl Pts',(18.2573203896198,-23.0493077902555,-5.92147920377189));
#12589=CARTESIAN_POINT('Ctrl Pts',(18.2671348228347,-23.0570717757452,-5.86650096730342));
#12590=CARTESIAN_POINT('Ctrl Pts',(18.2770455748766,-23.0649868063112,-5.81157531072592));
#12591=CARTESIAN_POINT('Ctrl Pts',(18.2870358543848,-23.0730255541295,-5.75669829320565));
#12592=CARTESIAN_POINT('Ctrl Pts',(18.2923577031983,-23.0773078167532,-5.72746515810246));
#12593=CARTESIAN_POINT('Ctrl Pts',(18.2977035116034,-23.0816279527548,-5.69822802204645));
#12594=CARTESIAN_POINT('Ctrl Pts',(18.3030719898805,-23.0859836968892,-5.66898786636628));
#12595=CARTESIAN_POINT('Ctrl Pts',(18.326479713442,-23.1049756810869,-5.54149447890509));
#12596=CARTESIAN_POINT('Ctrl Pts',(18.3502967025003,-23.1246111362575,-5.41409447936928));
#12597=CARTESIAN_POINT('Ctrl Pts',(18.3744213032108,-23.1447278442602,-5.28681965750206));
#12598=CARTESIAN_POINT('Ctrl Pts',(18.4018259099811,-23.1675796410191,-5.14224041712917));
#12599=CARTESIAN_POINT('Ctrl Pts',(18.4296274978877,-23.1910529746929,-4.99782274608269));
#12600=CARTESIAN_POINT('Ctrl Pts',(18.4577147532105,-23.214943810437,-4.85356339888911));
#12601=CARTESIAN_POINT('Ctrl Pts',(18.4890884148577,-23.2416300419142,-4.69242469393962));
#12602=CARTESIAN_POINT('Ctrl Pts',(18.5208193133129,-23.2688383567222,-4.53148298254906));
#12603=CARTESIAN_POINT('Ctrl Pts',(18.5527900614526,-23.296309683901,-4.37067927495082));
#12604=CARTESIAN_POINT('Ctrl Pts',(18.5927280414385,-23.3306269701359,-4.16980267276329));
#12605=CARTESIAN_POINT('Ctrl Pts',(18.6330437593144,-23.3653575842487,-3.96914004956012));
#12606=CARTESIAN_POINT('Ctrl Pts',(18.6735332660427,-23.4,-3.76850837361349));
#12607=CARTESIAN_POINT('Origin',(0.,13.15,0.));
#12608=CARTESIAN_POINT('',(1.82293408768446,12.6595351585866,19.3672161093864));
#12609=CARTESIAN_POINT('Ctrl Pts',(-6.07314264709777,13.15,18.0560083736135));
#12610=CARTESIAN_POINT('Ctrl Pts',(-5.89143659083433,13.1379692270487,18.1171252482126));
#12611=CARTESIAN_POINT('Ctrl Pts',(-5.70926339248799,13.1259554920724,18.1757473227728));
#12612=CARTESIAN_POINT('Ctrl Pts',(-5.52650317309585,13.1139455296796,18.2320030637526));
#12613=CARTESIAN_POINT('Ctrl Pts',(-5.34710195439919,13.1021563017123,18.2872248648864));
#12614=CARTESIAN_POINT('Ctrl Pts',(-5.16713396323832,13.0903706662046,18.3401664122538));
#12615=CARTESIAN_POINT('Ctrl Pts',(-4.98648886991423,13.0785760987252,18.3909003151281));
#12616=CARTESIAN_POINT('Ctrl Pts',(-4.81108595020798,13.0671237999969,18.4401619614231));
#12617=CARTESIAN_POINT('Ctrl Pts',(-4.63504371157761,13.0556630399472,18.4873420908706));
#12618=CARTESIAN_POINT('Ctrl Pts',(-4.45827906291381,13.0441829768623,18.5324625404846));
#12619=CARTESIAN_POINT('Ctrl Pts',(-4.29057738820271,13.0332915128753,18.5752696007265));
#12620=CARTESIAN_POINT('Ctrl Pts',(-4.12222485300671,13.0223826439246,18.616222526144));
#12621=CARTESIAN_POINT('Ctrl Pts',(-3.95317780433264,13.0114481775481,18.6553021950897));
#12622=CARTESIAN_POINT('Ctrl Pts',(-3.87704203806503,13.0065234895229,18.6729029788005));
#12623=CARTESIAN_POINT('Ctrl Pts',(-3.80076582857587,13.0015936267076,18.6901232797613));
#12624=CARTESIAN_POINT('Ctrl Pts',(-3.72434765372577,12.996657942793,18.7069588323863));
#12625=CARTESIAN_POINT('Ctrl Pts',(-3.58036899032601,12.987358673681,18.7386785164706));
#12626=CARTESIAN_POINT('Ctrl Pts',(-3.43573644023662,12.9780292666602,18.7690854619261));
#12627=CARTESIAN_POINT('Ctrl Pts',(-3.29066907106318,12.9686821009665,18.798166713184));
#12628=CARTESIAN_POINT('Ctrl Pts',(-3.15493537978566,12.9599363347077,18.825376868043));
#12629=CARTESIAN_POINT('Ctrl Pts',(-3.01882077394898,12.9511750020393,18.8514262764423));
#12630=CARTESIAN_POINT('Ctrl Pts',(-2.88254718378542,12.9424107435028,18.8762907389895));
#12631=CARTESIAN_POINT('Ctrl Pts',(-2.78114456358843,12.9358891660011,18.8947926486335));
#12632=CARTESIAN_POINT('Ctrl Pts',(-2.67965469546404,12.9293660137815,18.9126381832964));
#12633=CARTESIAN_POINT('Ctrl Pts',(-2.57818729839884,12.9228475964189,18.929812644131));
#12634=CARTESIAN_POINT('Ctrl Pts',(-2.44377209138411,12.9142125624618,18.9525638802443));
#12635=CARTESIAN_POINT('Ctrl Pts',(-2.30940063942545,12.9055857664759,18.9741477153703));
#12636=CARTESIAN_POINT('Ctrl Pts',(-2.17514817924979,12.8969734463819,18.9946057570328));
#12637=CARTESIAN_POINT('Ctrl Pts',(-2.05167325408668,12.8890525071477,19.0134214655863));
#12638=CARTESIAN_POINT('Ctrl Pts',(-1.92817267861986,12.8811371827706,19.0313039403008));
#12639=CARTESIAN_POINT('Ctrl Pts',(-1.80456225428477,12.8732239828736,19.0482998974936));
#12640=CARTESIAN_POINT('Ctrl Pts',(-1.70031647335247,12.8665504542666,19.062633290812));
#12641=CARTESIAN_POINT('Ctrl Pts',(-1.59599311213552,12.8598784744128,19.0763358597885));
#12642=CARTESIAN_POINT('Ctrl Pts',(-1.49156999562427,12.8532079839211,19.0894300738828));
#12643=CARTESIAN_POINT('Ctrl Pts',(-1.37302337322002,12.8456352917434,19.1042953154669));
#12644=CARTESIAN_POINT('Ctrl Pts',(-1.25434655584515,12.83806400913,19.1183773452858));
#12645=CARTESIAN_POINT('Ctrl Pts',(-1.13553246318378,12.8305004633234,19.1317219358192));
#12646=CARTESIAN_POINT('Ctrl Pts',(-1.02214813267873,12.8232825688942,19.1444566832688));
#12647=CARTESIAN_POINT('Ctrl Pts',(-0.908638694765087,12.8160717028953,
19.1565195853913));
#12648=CARTESIAN_POINT('Ctrl Pts',(-0.79504399785826,12.8088775452768,19.1679520323113));
#12649=CARTESIAN_POINT('Ctrl Pts',(-0.692063351944374,12.8023555947057,
19.1783162552922));
#12650=CARTESIAN_POINT('Ctrl Pts',(-0.58901291751484,12.795847396274,19.1881621901356));
#12651=CARTESIAN_POINT('Ctrl Pts',(-0.485959105372368,12.7893635951272,
19.1975247440753));
#12652=CARTESIAN_POINT('Ctrl Pts',(-0.397291306545851,12.7837849138173,
19.2055803126366));
#12653=CARTESIAN_POINT('Ctrl Pts',(-0.308450767230545,12.7782136874732,
19.2132892091623));
#12654=CARTESIAN_POINT('Ctrl Pts',(-0.219666931641276,12.7726724740284,
19.2206736432458));
#12655=CARTESIAN_POINT('Ctrl Pts',(-0.207021284979042,12.7718832287019,
19.2217254219124));
#12656=CARTESIAN_POINT('Ctrl Pts',(-0.194376874651241,12.7710945998699,
19.2227706248721));
#12657=CARTESIAN_POINT('Ctrl Pts',(-0.181734451453492,12.7703066605067,
19.2238093232609));
#12658=CARTESIAN_POINT('Ctrl Pts',(-0.112648562634309,12.7660008806426,
19.22948540294));
#12659=CARTESIAN_POINT('Ctrl Pts',(-0.0436037693110482,12.7617151304109,
19.2349679902415));
#12660=CARTESIAN_POINT('Ctrl Pts',(0.02547635923879,12.757449305424,19.2402849388918));
#12661=CARTESIAN_POINT('Ctrl Pts',(0.0916269448846765,12.7533643850993,
19.245376406937));
#12662=CARTESIAN_POINT('Ctrl Pts',(0.157810333253506,12.749297698185,19.250315856965));
#12663=CARTESIAN_POINT('Ctrl Pts',(0.224046235742999,12.7452532521653,19.2551251194837));
#12664=CARTESIAN_POINT('Ctrl Pts',(0.286785346628499,12.74142232456,19.2596804866349));
#12665=CARTESIAN_POINT('Ctrl Pts',(0.34957181954994,12.7376113278546,19.2641189432598));
#12666=CARTESIAN_POINT('Ctrl Pts',(0.412374550348153,12.7338278436746,19.2684582922758));
#12667=CARTESIAN_POINT('Ctrl Pts',(0.415874887835622,12.7336169695399,19.2687001477786));
#12668=CARTESIAN_POINT('Ctrl Pts',(0.419375262237528,12.7334061820621,19.2689416954471));
#12669=CARTESIAN_POINT('Ctrl Pts',(0.422875663239959,12.7331954829858,19.2691829383935));
#12670=CARTESIAN_POINT('Ctrl Pts',(0.490997749735726,12.7290950211557,19.273877821308));
#12671=CARTESIAN_POINT('Ctrl Pts',(0.559094103262397,12.7250294339064,19.2784597940843));
#12672=CARTESIAN_POINT('Ctrl Pts',(0.627197583147417,12.72100812477,19.2829652951132));
#12673=CARTESIAN_POINT('Ctrl Pts',(0.691552601732308,12.7172081511909,19.2872228103376));
#12674=CARTESIAN_POINT('Ctrl Pts',(0.7559138409642,12.7134477064408,19.2914118703163));
#12675=CARTESIAN_POINT('Ctrl Pts',(0.820267024024453,12.7097399996136,19.2955695468785));
#12676=CARTESIAN_POINT('Ctrl Pts',(0.874397449907384,12.706621276653,19.2990667601054));
#12677=CARTESIAN_POINT('Ctrl Pts',(0.928336362683676,12.7035507329861,19.3025295407969));
#12678=CARTESIAN_POINT('Ctrl Pts',(0.982238818325173,12.7005283628061,19.3059969894654));
#12679=CARTESIAN_POINT('Ctrl Pts',(1.03466360068771,12.6975888473977,19.3093693820519));
#12680=CARTESIAN_POINT('Ctrl Pts',(1.08705397397595,12.6946948638824,19.3127459826068));
#12681=CARTESIAN_POINT('Ctrl Pts',(1.13950386109632,12.6918520765328,19.3161671454685));
#12682=CARTESIAN_POINT('Ctrl Pts',(1.15856271360277,12.6908190854669,19.3174103023552));
#12683=CARTESIAN_POINT('Ctrl Pts',(1.17762894267694,12.6897929124046,19.3186594013673));
#12684=CARTESIAN_POINT('Ctrl Pts',(1.19670535537073,12.6887740383049,19.3199166147567));
#12685=CARTESIAN_POINT('Ctrl Pts',(1.2486425919455,12.68600006261,19.3233394904449));
#12686=CARTESIAN_POINT('Ctrl Pts',(1.30066077866098,12.6832787578847,19.3268211239109));
#12687=CARTESIAN_POINT('Ctrl Pts',(1.35277970669886,12.6806283209993,19.3304073273177));
#12688=CARTESIAN_POINT('Ctrl Pts',(1.40175117770664,12.6781379437415,19.3337769602472));
#12689=CARTESIAN_POINT('Ctrl Pts',(1.45081143546155,12.6757101114834,19.3372387703585));
#12690=CARTESIAN_POINT('Ctrl Pts',(1.49992966112441,12.6733674903705,19.3408403785556));
#12691=CARTESIAN_POINT('Ctrl Pts',(1.54792459291616,12.6710784430971,19.3443596209025));
#12692=CARTESIAN_POINT('Ctrl Pts',(1.59597502673672,12.6688706813137,19.348012128234));
#12693=CARTESIAN_POINT('Ctrl Pts',(1.64400519519223,12.666773564035,19.3518544508691));
#12694=CARTESIAN_POINT('Ctrl Pts',(1.6904627290876,12.6647451119144,19.3555709657138));
#12695=CARTESIAN_POINT('Ctrl Pts',(1.73690137116093,12.6628201182928,19.3594648742118));
#12696=CARTESIAN_POINT('Ctrl Pts',(1.78320656534742,12.6610338566191,19.3636017376306));
#12697=CARTESIAN_POINT('Ctrl Pts',(1.79646145024437,12.6605225383254,19.3647859168445));
#12698=CARTESIAN_POINT('Ctrl Pts',(1.80970510015646,12.6600226469239,19.3659901067536));
#12699=CARTESIAN_POINT('Ctrl Pts',(1.82293408768446,12.6595351585866,19.3672161093864));
#12700=CARTESIAN_POINT('Ctrl Pts',(1.82293408768446,12.6595351585866,19.3672161093864));
#12701=CARTESIAN_POINT('Ctrl Pts',(1.92899847198764,12.6556266847333,19.3770456765946));
#12702=CARTESIAN_POINT('Ctrl Pts',(2.03513094440902,12.6527974939074,19.3867477665312));
#12703=CARTESIAN_POINT('Ctrl Pts',(2.14128049080422,12.6512766915374,19.3963919419144));
#12704=CARTESIAN_POINT('Ctrl Pts',(2.19967982607374,12.650440005461,19.4016977906035));
#12705=CARTESIAN_POINT('Ctrl Pts',(2.25808442071507,12.65,19.4069865889968));
#12706=CARTESIAN_POINT('Ctrl Pts',(2.31648752866395,12.65,19.4122740947459));
#12707=CARTESIAN_POINT('',(15.8610341074694,12.6595351585866,11.2623152840528));
#12708=CARTESIAN_POINT('Ctrl Pts',(15.6532787469444,12.65,11.7122740947461));
#12709=CARTESIAN_POINT('Ctrl Pts',(15.6980337221155,12.65,11.6155345352022));
#12710=CARTESIAN_POINT('Ctrl Pts',(15.7427862154013,12.6514513272118,11.5187867449086));
#12711=CARTESIAN_POINT('Ctrl Pts',(15.7874388179956,12.6541030519079,11.4220256779294));
#12712=CARTESIAN_POINT('Ctrl Pts',(15.8120049363218,12.6555619272896,11.3687915172607));
#12713=CARTESIAN_POINT('Ctrl Pts',(15.8365411965293,12.6573848688951,11.3155539383097));
#12714=CARTESIAN_POINT('Ctrl Pts',(15.8610341074694,12.6595351585866,11.2623152840528));
#12715=CARTESIAN_POINT('Ctrl Pts',(15.8610341074694,12.6595351585866,11.2623152840528));
#12716=CARTESIAN_POINT('Ctrl Pts',(15.8755315725394,12.6608079247682,11.2308030834822));
#12717=CARTESIAN_POINT('Ctrl Pts',(15.8902824743543,12.6621745127569,11.1991317971907));
#12718=CARTESIAN_POINT('Ctrl Pts',(15.9051841193332,12.6636122851386,11.1674271960182));
#12719=CARTESIAN_POINT('Ctrl Pts',(15.9206585676617,12.6651053239581,11.1345039037699));
#12720=CARTESIAN_POINT('Ctrl Pts',(15.9362957629233,12.6666751553055,11.1015444562721));
#12721=CARTESIAN_POINT('Ctrl Pts',(15.9520132214841,12.6683023351355,11.0686433208445));
#12722=CARTESIAN_POINT('Ctrl Pts',(15.9687080951478,12.6700307037253,11.0336961760989));
#12723=CARTESIAN_POINT('Ctrl Pts',(15.9854936245323,12.6718237880044,10.998814731488));
#12724=CARTESIAN_POINT('Ctrl Pts',(16.0023047914919,12.6736645084142,10.9640631789662));
#12725=CARTESIAN_POINT('Ctrl Pts',(16.0197345727335,12.6755729633208,10.9280328450984));
#12726=CARTESIAN_POINT('Ctrl Pts',(16.0371921625325,12.6775326648007,10.8921418342238));
#12727=CARTESIAN_POINT('Ctrl Pts',(16.0546374221841,12.679530611801,10.856413971676));
#12728=CARTESIAN_POINT('Ctrl Pts',(16.0730820056298,12.6816430079993,10.8186394956717));
#12729=CARTESIAN_POINT('Ctrl Pts',(16.0915129761836,12.6837981812692,10.781047216685));
#12730=CARTESIAN_POINT('Ctrl Pts',(16.1099151779263,12.6859869025207,10.7436165469437));
#12731=CARTESIAN_POINT('Ctrl Pts',(16.1180616880166,12.6869558322178,10.7270462836133));
#12732=CARTESIAN_POINT('Ctrl Pts',(16.1262029523282,12.6879314118327,10.7105070921922));
#12733=CARTESIAN_POINT('Ctrl Pts',(16.1343393771825,12.6889131739459,10.6939945272582));
#12734=CARTESIAN_POINT('Ctrl Pts',(16.1554826056401,12.6914643706966,10.6510851488677));
#12735=CARTESIAN_POINT('Ctrl Pts',(16.1765726356144,12.6940529314347,10.6083837729401));
#12736=CARTESIAN_POINT('Ctrl Pts',(16.1976696182531,12.69667992237,10.5657060705175));
#12737=CARTESIAN_POINT('Ctrl Pts',(16.2193768925724,12.6993829066707,10.5217937912274));
#12738=CARTESIAN_POINT('Ctrl Pts',(16.2410917763085,12.7021266206828,10.4779065846965));
#12739=CARTESIAN_POINT('Ctrl Pts',(16.2629098463051,12.7049186032388,10.4337975121256));
#12740=CARTESIAN_POINT('Ctrl Pts',(16.275331417334,12.7065081484936,10.4086851177642));
#12741=CARTESIAN_POINT('Ctrl Pts',(16.2877869550192,12.7081134503575,10.3834999760487));
#12742=CARTESIAN_POINT('Ctrl Pts',(16.3002978241236,12.7097367072451,10.3581900732938));
#12743=CARTESIAN_POINT('Ctrl Pts',(16.3332728445508,12.7140151413477,10.2914805143182));
#12744=CARTESIAN_POINT('Ctrl Pts',(16.3662336781026,12.7183664950041,10.2247075060269));
#12745=CARTESIAN_POINT('Ctrl Pts',(16.3990971166876,12.7227674591413,10.1579087130742));
#12746=CARTESIAN_POINT('Ctrl Pts',(16.4256676679983,12.7263257004105,10.1039009514988));
#12747=CARTESIAN_POINT('Ctrl Pts',(16.4521754332255,12.7299165458893,10.0498755479769));
#12748=CARTESIAN_POINT('Ctrl Pts',(16.4785931654052,12.7335310522426,9.99583444252971));
#12749=CARTESIAN_POINT('Ctrl Pts',(16.5112266697307,12.7379960081257,9.9290781200575));
#12750=CARTESIAN_POINT('Ctrl Pts',(16.5437407424326,12.742500292084,9.86225899460185));
#12751=CARTESIAN_POINT('Ctrl Pts',(16.5760904789354,12.7470331104531,9.79538472693205));
#12752=CARTESIAN_POINT('Ctrl Pts',(16.6098424954697,12.7517624151426,9.72561162729884));
#12753=CARTESIAN_POINT('Ctrl Pts',(16.6434158824976,12.7565228077862,9.65577848505558));
#12754=CARTESIAN_POINT('Ctrl Pts',(16.6767921271902,12.7613076794793,9.58584680971152));
#12755=CARTESIAN_POINT('Ctrl Pts',(16.6976670791072,12.7643003458935,9.54210850500634));
#12756=CARTESIAN_POINT('Ctrl Pts',(16.718465539199,12.7673026982108,9.49833072232483));
#12757=CARTESIAN_POINT('Ctrl Pts',(16.7391883141092,12.7703140978295,9.45449535259596));
#12758=CARTESIAN_POINT('Ctrl Pts',(16.7808367856317,12.7763663853155,9.36639536812287));
#12759=CARTESIAN_POINT('Ctrl Pts',(16.8222902539778,12.7824713543034,9.2778265112276));
#12760=CARTESIAN_POINT('Ctrl Pts',(16.8634541590761,12.7886112584458,9.18886180766335));
#12761=CARTESIAN_POINT('Ctrl Pts',(16.8657796830592,12.788958127731,9.18383581337804));
#12762=CARTESIAN_POINT('Ctrl Pts',(16.8681042913027,12.789305109897,9.17880854502639));
#12763=CARTESIAN_POINT('Ctrl Pts',(16.87042796971,12.7896522022311,9.17378001198317));
#12764=CARTESIAN_POINT('Ctrl Pts',(16.9167422154902,12.7965702506232,9.07355413109334));
#12765=CARTESIAN_POINT('Ctrl Pts',(16.962447971316,12.8034966804412,8.97333336966089));
#12766=CARTESIAN_POINT('Ctrl Pts',(17.0075101299617,12.810423211497,8.87310027386457));
#12767=CARTESIAN_POINT('Ctrl Pts',(17.0548200626743,12.8176952492339,8.76786738755362));
#12768=CARTESIAN_POINT('Ctrl Pts',(17.1014209523388,12.8249674208786,8.66262094537315));
#12769=CARTESIAN_POINT('Ctrl Pts',(17.1473021985064,12.8322356635336,8.55728965067821));
#12770=CARTESIAN_POINT('Ctrl Pts',(17.1927178496159,12.8394301493023,8.45302723999089));
#12771=CARTESIAN_POINT('Ctrl Pts',(17.237428958698,12.8466208518308,8.34868128905732));
#12772=CARTESIAN_POINT('Ctrl Pts',(17.2814464207459,12.8538083506489,8.2441373109611));
#12773=CARTESIAN_POINT('Ctrl Pts',(17.3282209127514,12.8614460378386,8.13304522976901));
#12774=CARTESIAN_POINT('Ctrl Pts',(17.3742029960782,12.8690793531583,8.02170985269986));
#12775=CARTESIAN_POINT('Ctrl Pts',(17.4194367848341,12.8767174233848,7.90998003610143));
#12776=CARTESIAN_POINT('Ctrl Pts',(17.4592412159324,12.8834387051615,7.81166101598985));
#12777=CARTESIAN_POINT('Ctrl Pts',(17.4984666249301,12.8901637443241,7.71303551607771));
#12778=CARTESIAN_POINT('Ctrl Pts',(17.537147804236,12.8969009187565,7.61396771456222));
#12779=CARTESIAN_POINT('Ctrl Pts',(17.592514077251,12.9065441676352,7.47216710134099));
#12780=CARTESIAN_POINT('Ctrl Pts',(17.6466111403711,12.9161930408258,7.3298409308964));
#12781=CARTESIAN_POINT('Ctrl Pts',(17.6993823050438,12.9258391470742,7.18703139954518));
#12782=CARTESIAN_POINT('Ctrl Pts',(17.7538795876936,12.9358007725557,7.03955064100196));
#12783=CARTESIAN_POINT('Ctrl Pts',(17.8069632788614,12.9457594336855,6.89155414629607));
#12784=CARTESIAN_POINT('Ctrl Pts',(17.8585858804981,12.9557103540787,6.74303368137663));
#12785=CARTESIAN_POINT('Ctrl Pts',(17.9126720143282,12.9661361519861,6.58742552743936));
#12786=CARTESIAN_POINT('Ctrl Pts',(17.9651548061949,12.9765534332868,6.43124205075313));
#12787=CARTESIAN_POINT('Ctrl Pts',(18.0159880164975,12.9869618042602,6.2744175466783));
#12788=CARTESIAN_POINT('Ctrl Pts',(18.0316413020919,12.9901668979863,6.22612591339651));
#12789=CARTESIAN_POINT('Ctrl Pts',(18.0471381945933,12.9933711829021,6.17777311859869));
#12790=CARTESIAN_POINT('Ctrl Pts',(18.0624773722234,12.9965747421708,6.12935627695676));
#12791=CARTESIAN_POINT('Ctrl Pts',(18.1057590938429,13.0056140507834,5.9927411133419));
#12792=CARTESIAN_POINT('Ctrl Pts',(18.1477566607642,13.0146488660571,5.8556152595047));
#12793=CARTESIAN_POINT('Ctrl Pts',(18.1884785365491,13.0236795201517,5.71803784983784));
#12794=CARTESIAN_POINT('Ctrl Pts',(18.2387485231049,13.0348276033668,5.54820248736866));
#12795=CARTESIAN_POINT('Ctrl Pts',(18.2870623372161,13.0459810891294,5.37771014955191));
#12796=CARTESIAN_POINT('Ctrl Pts',(18.333408890949,13.0571305535019,5.206676417006));
#12797=CARTESIAN_POINT('Ctrl Pts',(18.3822015246055,13.0688684646684,5.02661586054878));
#12798=CARTESIAN_POINT('Ctrl Pts',(18.4288144063872,13.0806018838886,4.84595419871784));
#12799=CARTESIAN_POINT('Ctrl Pts',(18.4732069565691,13.0923262622486,4.66477210676923));
#12800=CARTESIAN_POINT('Ctrl Pts',(18.5198097359117,13.104634377358,4.47456926828994));
#12801=CARTESIAN_POINT('Ctrl Pts',(18.5639664343605,13.1169325338878,4.28379137577915));
#12802=CARTESIAN_POINT('Ctrl Pts',(18.6055886379374,13.1292226566585,4.09249383743625));
#12803=CARTESIAN_POINT('Ctrl Pts',(18.6290505764319,13.1361504519157,3.98466170234839));
#12804=CARTESIAN_POINT('Ctrl Pts',(18.651706382388,13.1430758235437,3.87666390827378));
#12805=CARTESIAN_POINT('Ctrl Pts',(18.6735332660427,13.15,3.76850837361377));
#12806=CARTESIAN_POINT('Origin',(0.,13.15,0.));
#12807=CARTESIAN_POINT('',(-17.6839681951541,12.6595351585866,8.10490082533369));
#12808=CARTESIAN_POINT('Ctrl Pts',(-17.9697662756086,12.65,7.7));
#12809=CARTESIAN_POINT('Ctrl Pts',(-17.9083648469828,12.65,7.78712872535143));
#12810=CARTESIAN_POINT('Ctrl Pts',(-17.8469550493761,12.6514513272162,7.87425941670175));
#12811=CARTESIAN_POINT('Ctrl Pts',(-17.7854838084763,12.6541030519202,7.96131023851809));
#12812=CARTESIAN_POINT('Ctrl Pts',(-17.7516647322465,12.6555619272999,8.00920220125992));
#12813=CARTESIAN_POINT('Ctrl Pts',(-17.7178277666382,12.6573848689011,8.05707001525365));
#12814=CARTESIAN_POINT('Ctrl Pts',(-17.6839681951541,12.6595351585866,8.1049008253337));
#12815=CARTESIAN_POINT('Ctrl Pts',(-17.6839681951541,12.6595351585866,8.1049008253337));
#12816=CARTESIAN_POINT('Ctrl Pts',(-17.6639265614649,12.6608079247683,8.13321209866034));
#12817=CARTESIAN_POINT('Ctrl Pts',(-17.6438738738723,12.6621745127572,8.16182239750707));
#12818=CARTESIAN_POINT('Ctrl Pts',(-17.6238677063287,12.663612285139,8.19057990120395));
#12819=CARTESIAN_POINT('Ctrl Pts',(-17.6030925230288,12.6651053239586,8.22044281269102));
#12820=CARTESIAN_POINT('Ctrl Pts',(-17.5823674018309,12.6666751553062,8.25046474478147));
#12821=CARTESIAN_POINT('Ctrl Pts',(-17.5617329120168,12.6683023351362,8.28052703089315));
#12822=CARTESIAN_POINT('Ctrl Pts',(-17.5398152337084,12.6700307037261,8.31245878797306));
#12823=CARTESIAN_POINT('Ctrl Pts',(-17.5179997812459,12.6718237880053,8.34443620514295));
#12824=CARTESIAN_POINT('Ctrl Pts',(-17.4963096374199,12.6736645084151,8.37637087905986));
#12825=CARTESIAN_POINT('Ctrl Pts',(-17.4738213436033,12.6755729633218,8.4094806793332));
#12826=CARTESIAN_POINT('Ctrl Pts',(-17.451467611317,12.6775326648018,8.44254490102727));
#12827=CARTESIAN_POINT('Ctrl Pts',(-17.4292490045524,12.6795306118022,8.47551687033708));
#12828=CARTESIAN_POINT('Ctrl Pts',(-17.4057576404398,12.6816430080006,8.51037758616752));
#12829=CARTESIAN_POINT('Ctrl Pts',(-17.3824172571268,12.6837981812706,8.5451354143792));
#12830=CARTESIAN_POINT('Ctrl Pts',(-17.3592024471202,12.6859869025222,8.57978752344679));
#12831=CARTESIAN_POINT('Ctrl Pts',(-17.3489254331789,12.6869558322188,8.59512773979505));
#12832=CARTESIAN_POINT('Ctrl Pts',(-17.338672705411,12.6879314118332,8.61044787721113));
#12833=CARTESIAN_POINT('Ctrl Pts',(-17.3284406171285,12.6889131739459,8.62575051029075));
#12834=CARTESIAN_POINT('Ctrl Pts',(-17.3018516196084,12.6914643706967,8.66551577245167));
#12835=CARTESIAN_POINT('Ctrl Pts',(-17.2754161582636,12.6940529314351,8.70513096214322));
#12836=CARTESIAN_POINT('Ctrl Pts',(-17.2490046751076,12.6966799223705,8.74474033626622));
#12837=CARTESIAN_POINT('Ctrl Pts',(-17.2218291628616,12.6993829066715,8.7854955269224));
#12838=CARTESIAN_POINT('Ctrl Pts',(-17.1946791689703,12.7021266206838,8.82624477114721));
#12839=CARTESIAN_POINT('Ctrl Pts',(-17.1673886265825,12.7049186032401,8.86719431031478));
#12840=CARTESIAN_POINT('Ctrl Pts',(-17.1518514406346,12.7065081484945,8.89050790355471));
#12841=CARTESIAN_POINT('Ctrl Pts',(-17.1362682369582,12.7081134503579,8.91388728645879));
#12842=CARTESIAN_POINT('Ctrl Pts',(-17.120604652762,12.709736707245,8.93737696829701));
#12843=CARTESIAN_POINT('Ctrl Pts',(-17.0793199902274,12.7140151413476,8.99928895316511));
#12844=CARTESIAN_POINT('Ctrl Pts',(-17.0379732855358,12.7183664950041,9.06122037649655));
#12845=CARTESIAN_POINT('Ctrl Pts',(-16.996555553189,12.7227674591413,9.12308034564325));
#12846=CARTESIAN_POINT('Ctrl Pts',(-16.9630687353186,12.7263257004105,9.1730949988584));
#12847=CARTESIAN_POINT('Ctrl Pts',(-16.9295352460326,12.7299165458893,9.22306409870345));
#12848=CARTESIAN_POINT('Ctrl Pts',(-16.8959431419567,12.7335310522426,9.2729630786048));
#12849=CARTESIAN_POINT('Ctrl Pts',(-16.8544472229965,12.7379960081256,9.33460268359952));
#12850=CARTESIAN_POINT('Ctrl Pts',(-16.8128371992455,12.7425002920837,9.39617025926588));
#12851=CARTESIAN_POINT('Ctrl Pts',(-16.7710972528366,12.7470331104527,9.45762308671611));
#12852=CARTESIAN_POINT('Ctrl Pts',(-16.7275479843214,12.751762415142,9.52173974027936));
#12853=CARTESIAN_POINT('Ctrl Pts',(-16.6838574026273,12.7565228077855,9.58573171745721));
#12854=CARTESIAN_POINT('Ctrl Pts',(-16.6399829175973,12.7613076794785,9.64960223091488));
#12855=CARTESIAN_POINT('Ctrl Pts',(-16.6125419105606,12.7643003458929,9.68954962193329));
#12856=CARTESIAN_POINT('Ctrl Pts',(-16.5850284686809,12.7673026982104,9.72945050807611));
#12857=CARTESIAN_POINT('Ctrl Pts',(-16.5574273123645,12.7703140978294,9.76931464245264));
#12858=CARTESIAN_POINT('Ctrl Pts',(-16.5019547235018,12.7763663853151,9.84943326905253));
#12859=CARTESIAN_POINT('Ctrl Pts',(-16.4459785776221,12.7824713543027,9.9296174541588));
#12860=CARTESIAN_POINT('Ctrl Pts',(-16.3895148368472,12.788611258445,10.0097487934709));
#12861=CARTESIAN_POINT('Ctrl Pts',(-16.3863249601057,12.7889581277305,10.0142757534639));
#12862=CARTESIAN_POINT('Ctrl Pts',(-16.3831335221205,12.7893051098969,10.0188025574363));
#12863=CARTESIAN_POINT('Ctrl Pts',(-16.3799405239623,12.7896522022313,10.0233291884927));
#12864=CARTESIAN_POINT('Ctrl Pts',(-16.3162994878893,12.796570250623,10.113551442334));
#12865=CARTESIAN_POINT('Ctrl Pts',(-16.2523586404194,12.8034966804406,10.2032441686885));
#12866=CARTESIAN_POINT('Ctrl Pts',(-16.1880853124871,12.8104232114959,10.2923856907174));
#12867=CARTESIAN_POINT('Ctrl Pts',(-16.1206059259881,12.8176952492324,10.3859737374485));
#12868=CARTESIAN_POINT('Ctrl Pts',(-16.0527602782377,12.8249674208766,10.4789545128227));
#12869=CARTESIAN_POINT('Ctrl Pts',(-15.9844813243059,12.8322356635312,10.5713544849041));
#12870=CARTESIAN_POINT('Ctrl Pts',(-15.9168952535378,12.8394301493006,10.6628167978489));
#12871=CARTESIAN_POINT('Ctrl Pts',(-15.8488845637804,12.8466208518299,10.753710729623));
#12872=CARTESIAN_POINT('Ctrl Pts',(-15.7803555539523,12.8538083506489,10.8441029590253));
#12873=CARTESIAN_POINT('Ctrl Pts',(-15.7075342354825,12.8614460378387,10.9401568979484));
#12874=CARTESIAN_POINT('Ctrl Pts',(-15.6341060122632,12.8690793531585,11.035646238764));
#12875=CARTESIAN_POINT('Ctrl Pts',(-15.5599620471059,12.8767174233851,11.1306847572363));
#12876=CARTESIAN_POINT('Ctrl Pts',(-15.4947174935641,12.8834387051617,11.2143159158053));
#12877=CARTESIAN_POINT('Ctrl Pts',(-15.428918009679,12.8901637443243,11.297598866426));
#12878=CARTESIAN_POINT('Ctrl Pts',(-15.3624633665233,12.8969009187565,11.3806316511099));
#12879=CARTESIAN_POINT('Ctrl Pts',(-15.2673435697082,12.9065441676353,11.4994805566654));
#12880=CARTESIAN_POINT('Ctrl Pts',(-15.1711340220391,12.916193040826,11.6174930728209));
#12881=CARTESIAN_POINT('Ctrl Pts',(-15.0738429223219,12.9258391470746,11.7345990076912));
#12882=CARTESIAN_POINT('Ctrl Pts',(-14.9733694801788,12.9358007725561,11.8555354181748));
#12883=CARTESIAN_POINT('Ctrl Pts',(-14.8717426016762,12.945759433686,11.9755054906058));
#12884=CARTESIAN_POINT('Ctrl Pts',(-14.7689314068923,12.9557103540793,12.0944722074925));
#12885=CARTESIAN_POINT('Ctrl Pts',(-14.6612138594637,12.9661361519865,12.219116250348));
#12886=CARTESIAN_POINT('Ctrl Pts',(-14.5521963969374,12.9765534332871,12.3426594197069));
#12887=CARTESIAN_POINT('Ctrl Pts',(-14.441798997626,12.9869618042603,12.4650945232202));
#12888=CARTESIAN_POINT('Ctrl Pts',(-14.4078038592099,12.9901668979865,12.5027964828396));
#12889=CARTESIAN_POINT('Ctrl Pts',(-14.3736775568208,12.9933711829024,12.5403935828256));
#12890=CARTESIAN_POINT('Ctrl Pts',(-14.3394169308019,12.9965747421713,12.5778861211484));
#12891=CARTESIAN_POINT('Ctrl Pts',(-14.242745589379,13.0056140507838,12.683676773398));
#12892=CARTESIAN_POINT('Ctrl Pts',(-14.144989899901,13.0146488660574,12.7886106601676));
#12893=CARTESIAN_POINT('Ctrl Pts',(-14.046205306035,13.0236795201519,12.8926655439204));
#12894=CARTESIAN_POINT('Ctrl Pts',(-13.9242585601308,13.0348276034422,13.0211183114271));
#12895=CARTESIAN_POINT('Ctrl Pts',(-13.8007647706452,13.0459810892792,13.1482054715556));
#12896=CARTESIAN_POINT('Ctrl Pts',(-13.675818489362,13.0571305537241,13.2738596315664));
#12897=CARTESIAN_POINT('Ctrl Pts',(-13.544277788722,13.0688684650071,13.4061455713829));
#12898=CARTESIAN_POINT('Ctrl Pts',(-13.411126639588,13.0806018843413,13.5368443433571));
#12899=CARTESIAN_POINT('Ctrl Pts',(-13.2764146189179,13.0923262628158,13.6658804667858));
#12900=CARTESIAN_POINT('Ctrl Pts',(-13.1349955163823,13.1046343781079,13.8013410788322));
#12901=CARTESIAN_POINT('Ctrl Pts',(-12.9918553619456,13.1169325348207,13.9349708496446));
#12902=CARTESIAN_POINT('Ctrl Pts',(-12.8469979335291,13.1292226577834,14.0666655063646));
#12903=CARTESIAN_POINT('Ctrl Pts',(-12.7653435388819,13.1361504526617,14.1409002045109));
#12904=CARTESIAN_POINT('Ctrl Pts',(-12.6831426131348,13.143075823914,14.2145196009598));
#12905=CARTESIAN_POINT('Ctrl Pts',(-12.6003906189451,13.15,14.2875));
#12906=CARTESIAN_POINT('',(-17.6839681951541,12.6595351585866,-8.10490082533369));
#12907=CARTESIAN_POINT('Ctrl Pts',(-12.6003906189451,13.15,-14.2875));
#12908=CARTESIAN_POINT('Ctrl Pts',(-12.7441724131263,13.1379692270445,-14.1606963765126));
#12909=CARTESIAN_POINT('Ctrl Pts',(-12.8860272181368,13.125955492064,-14.0322407960939));
#12910=CARTESIAN_POINT('Ctrl Pts',(-13.0261262286746,13.113945529667,-13.9020936737457));
#12911=CARTESIAN_POINT('Ctrl Pts',(-13.1636503206767,13.1021563016968,-13.7743385614223));
#12912=CARTESIAN_POINT('Ctrl Pts',(-13.2994830412214,13.0903706661861,-13.6449524828629));
#12913=CARTESIAN_POINT('Ctrl Pts',(-13.4337424366336,13.0785760987039,-13.5138761943818));
#12914=CARTESIAN_POINT('Ctrl Pts',(-13.5641057336281,13.0671237999736,-13.3866036331451));
#12915=CARTESIAN_POINT('Ctrl Pts',(-13.6929860436161,13.0556630399218,-13.2577366470546));
#12916=CARTESIAN_POINT('Ctrl Pts',(-13.8204438235608,13.0441829768352,-13.1272141956059));
#12917=CARTESIAN_POINT('Ctrl Pts',(-13.941366662559,13.0332915128467,-13.0033838151535));
#12918=CARTESIAN_POINT('Ctrl Pts',(-14.0610092039394,13.0223826438948,-12.8780627055743));
#12919=CARTESIAN_POINT('Ctrl Pts',(-14.1793767143662,13.0114481775172,-12.7512035014433));
#12920=CARTESIAN_POINT('Ctrl Pts',(-14.2326873232158,13.0065234895016,-12.6940683856839));
#12921=CARTESIAN_POINT('Ctrl Pts',(-14.2857386459499,13.001593626696,-12.636621401153));
#12922=CARTESIAN_POINT('Ctrl Pts',(-14.3385277495326,12.9966579427912,-12.5788590968463));
#12923=CARTESIAN_POINT('Ctrl Pts',(-14.4379871334572,12.9873586736788,-12.4700297587729));
#12924=CARTESIAN_POINT('Ctrl Pts',(-14.5366365957252,12.9780292666576,-12.3599777689006));
#12925=CARTESIAN_POINT('Ctrl Pts',(-14.6343553826822,12.9686821009635,-12.2488863675566));
#12926=CARTESIAN_POINT('Ctrl Pts',(-14.7257869136757,12.9599363347044,-12.1449426201832));
#12927=CARTESIAN_POINT('Ctrl Pts',(-14.8164036660272,12.9511750020356,-12.040088617895));
#12928=CARTESIAN_POINT('Ctrl Pts',(-14.9060737173319,12.9424107434987,-11.9345044582147));
#12929=CARTESIAN_POINT('Ctrl Pts',(-14.9727981511875,12.9358891659985,-11.8559381679508));
#12930=CARTESIAN_POINT('Ctrl Pts',(-15.038997771599,12.9293660137802,-11.776968131275));
#12931=CARTESIAN_POINT('Ctrl Pts',(-15.104604989498,12.922847596419,-11.6976820181931));
#12932=CARTESIAN_POINT('Ctrl Pts',(-15.191515741447,12.9142125624619,-11.59265065232));
#12933=CARTESIAN_POINT('Ctrl Pts',(-15.2773936169565,12.9055857664761,-11.4870734789433));
#12934=CARTESIAN_POINT('Ctrl Pts',(-15.3622370308358,12.896973446382,-11.3810364587419));
#12935=CARTESIAN_POINT('Ctrl Pts',(-15.4402693750153,12.8890525071477,-11.2835118910966));
#12936=CARTESIAN_POINT('Ctrl Pts',(-15.5175063401343,12.8811371827706,-11.1854984927171));
#12937=CARTESIAN_POINT('Ctrl Pts',(-15.5940304829928,12.8732239828736,-11.0869467036663));
#12938=CARTESIAN_POINT('Ctrl Pts',(-15.6585664561948,12.8665504542666,-11.0038339058012));
#12939=CARTESIAN_POINT('Ctrl Pts',(-15.7225949096337,12.8598784744129,-10.9203385092677));
#12940=CARTESIAN_POINT('Ctrl Pts',(-15.7861463899371,12.8532079839213,-10.8364525446741));
#12941=CARTESIAN_POINT('Ctrl Pts',(-15.8582933779828,12.845635291744,-10.7412207789333));
#12942=CARTESIAN_POINT('Ctrl Pts',(-15.9298271822287,12.8380640091307,-10.645484655158));
#12943=CARTESIAN_POINT('Ctrl Pts',(-16.0007909829629,12.8305004633243,-10.5492609278545));
#12944=CARTESIAN_POINT('Ctrl Pts',(-16.0685117630156,12.8232825688953,-10.4574345909735));
#12945=CARTESIAN_POINT('Ctrl Pts',(-16.135713261652,12.8160717028965,-10.3651639852349));
#12946=CARTESIAN_POINT('Ctrl Pts',(-16.2024113995638,12.8088775452781,-10.2725043154411));
#12947=CARTESIAN_POINT('Ctrl Pts',(-16.2628774029162,12.8023555947066,-10.1885025714674));
#12948=CARTESIAN_POINT('Ctrl Pts',(-16.3229294498328,12.7958473962744,-10.1041812447974));
#12949=CARTESIAN_POINT('Ctrl Pts',(-16.3825645654634,12.7893635951272,-10.0196153024904));
#12950=CARTESIAN_POINT('Ctrl Pts',(-16.4338747918932,12.7837849138171,-9.94685452048908));
#12951=CARTESIAN_POINT('Ctrl Pts',(-16.4849711617777,12.7782136874731,-9.87377080481835));
#12952=CARTESIAN_POINT('Ctrl Pts',(-16.5357581870816,12.7726724740281,-9.80057396479367));
#12953=CARTESIAN_POINT('Ctrl Pts',(-16.5429918774568,12.7718832287017,-9.79014840287087));
#12954=CARTESIAN_POINT('Ctrl Pts',(-16.5502192549354,12.7710945998698,-9.77972062379159));
#12955=CARTESIAN_POINT('Ctrl Pts',(-16.5574400057254,12.7703066605067,-9.76929131333199));
#12956=CARTESIAN_POINT('Ctrl Pts',(-16.5968985793309,12.7660008806426,-9.71229921841124));
#12957=CARTESIAN_POINT('Ctrl Pts',(-16.6361690358739,12.7617151304109,-9.65524596704519));
#12958=CARTESIAN_POINT('Ctrl Pts',(-16.6753137127505,12.757449305424,-9.59807929514968));
#12959=CARTESIAN_POINT('Ctrl Pts',(-16.7127983462431,12.7533643850993,-9.54333694152762));
#12960=CARTESIAN_POINT('Ctrl Pts',(-16.7501677296326,12.7492976981851,-9.48849017090563));
#12961=CARTESIAN_POINT('Ctrl Pts',(-16.787450624392,12.7452532521653,-9.43353282796637));
#12962=CARTESIAN_POINT('Ctrl Pts',(-16.8227652435108,12.7414223245601,-9.38147684770499));
#12963=CARTESIAN_POINT('Ctrl Pts',(-16.8580022961618,12.7376113278547,-9.3293213954541));
#12964=CARTESIAN_POINT('Ctrl Pts',(-16.8931616480444,12.7338278436747,-9.2771023096645));
#12965=CARTESIAN_POINT('Ctrl Pts',(-16.8951212697981,12.73361696954,-9.27419185622914));
#12966=CARTESIAN_POINT('Ctrl Pts',(-16.8970806434167,12.7334061820621,-9.27128121690781));
#12967=CARTESIAN_POINT('Ctrl Pts',(-16.8990397664385,12.7331954829857,-9.26837040218869));
#12968=CARTESIAN_POINT('Ctrl Pts',(-16.9371666975596,12.7290950211555,-9.21172238617983));
#12969=CARTESIAN_POINT('Ctrl Pts',(-16.975182979148,12.7250294339061,-9.15504020050686));
#12970=CARTESIAN_POINT('Ctrl Pts',(-17.0131365974396,12.7210081247695,-9.09831360735279));
#12971=CARTESIAN_POINT('Ctrl Pts',(-17.049001223072,12.7172081511905,-9.04470928401151));
#12972=CARTESIAN_POINT('Ctrl Pts',(-17.0848096750461,12.7134477064406,-8.99106534580903));
#12973=CARTESIAN_POINT('Ctrl Pts',(-17.1205869200985,12.7097399996136,-8.93741269274753));
#12974=CARTESIAN_POINT('Ctrl Pts',(-17.1506808085402,12.7066212766525,-8.89228297542374));
#12975=CARTESIAN_POINT('Ctrl Pts',(-17.1806491209783,12.7035507329854,-8.84730189704762));
#12976=CARTESIAN_POINT('Ctrl Pts',(-17.2106032474357,12.700528362805,-8.80235472546476));
#12977=CARTESIAN_POINT('Ctrl Pts',(-17.2397362162722,12.6975888473963,-8.75863972843841));
#12978=CARTESIAN_POINT('Ctrl Pts',(-17.2688556247791,12.6946948638806,-8.71495663452867));
#12979=CARTESIAN_POINT('Ctrl Pts',(-17.298043382292,12.6918520765307,-8.67124428128174));
#12980=CARTESIAN_POINT('Ctrl Pts',(-17.3086494139828,12.6908190854655,-8.65536040929836));
#12981=CARTESIAN_POINT('Ctrl Pts',(-17.319264279989,12.6897929124039,-8.63947312008266));
#12982=CARTESIAN_POINT('Ctrl Pts',(-17.3298912650618,12.6887740383049,-8.62358106878228));
#12983=CARTESIAN_POINT('Ctrl Pts',(-17.3588241806496,12.68600006261,-8.58031354034972));
#12984=CARTESIAN_POINT('Ctrl Pts',(-17.3878484570357,12.6832787578847,-8.53700528592784));
#12985=CARTESIAN_POINT('Ctrl Pts',(-17.4170136643082,12.6806283209993,-8.49366207193208));
#12986=CARTESIAN_POINT('Ctrl Pts',(-17.4444175875333,12.6781379437412,-8.45293635043883));
#12987=CARTESIAN_POINT('Ctrl Pts',(-17.4719457319131,12.6757101114829,-8.41217982595808));
#12988=CARTESIAN_POINT('Ctrl Pts',(-17.4996239289404,12.6733674903698,-8.37144299883949));
#12989=CARTESIAN_POINT('Ctrl Pts',(-17.5266691481136,12.6710784430962,-8.33163778982419));
#12990=CARTESIAN_POINT('Ctrl Pts',(-17.5538575291632,12.6688706813127,-8.29185114713442));
#12991=CARTESIAN_POINT('Ctrl Pts',(-17.5812001624053,12.6667735640338,-8.2521769624176));
#12992=CARTESIAN_POINT('Ctrl Pts',(-17.6076475256248,12.664745111913,-8.21380181528551));
#12993=CARTESIAN_POINT('Ctrl Pts',(-17.6342390703436,12.6628201182912,-8.17553172577809));
#12994=CARTESIAN_POINT('Ctrl Pts',(-17.6609742962525,12.6610338566174,-8.13749868299144));
#12995=CARTESIAN_POINT('Ctrl Pts',(-17.6686272679742,12.6605225383243,-8.12661170556599));
#12996=CARTESIAN_POINT('Ctrl Pts',(-17.6762919519737,12.6600226469234,-8.11574446327037));
#12997=CARTESIAN_POINT('Ctrl Pts',(-17.6839681951541,12.6595351585866,-8.1049008253337));
#12998=CARTESIAN_POINT('Ctrl Pts',(-17.6839681951541,12.6595351585866,-8.1049008253337));
#12999=CARTESIAN_POINT('Ctrl Pts',(-17.7455130422198,12.6556266847331,-8.01796115768933));
#13000=CARTESIAN_POINT('Ctrl Pts',(-17.8069815347887,12.6527974939074,-7.93089878537348));
#13001=CARTESIAN_POINT('Ctrl Pts',(-17.8684084088704,12.6512766915374,-7.84379266928167));
#13002=CARTESIAN_POINT('Ctrl Pts',(-17.9022030762551,12.6504400054611,-7.79587028572398));
#13003=CARTESIAN_POINT('Ctrl Pts',(-17.9359856073363,12.65,-7.74793482226751));
#13004=CARTESIAN_POINT('Ctrl Pts',(-17.9697662756086,12.65,-7.7));
#13005=CARTESIAN_POINT('Origin',(0.,22.22,7.70000000000001));
#13006=CARTESIAN_POINT('',(2.55537495509676,22.22,-8.00360031633711));
#13007=CARTESIAN_POINT('Ctrl Pts',(2.55537495509672,22.22,-8.00360031633714));
#13008=CARTESIAN_POINT('Ctrl Pts',(2.31636652071332,22.22,-8.05981884049116));
#13009=CARTESIAN_POINT('Ctrl Pts',(2.09333395643987,22.2199999999995,-8.10671764219108));
#13010=CARTESIAN_POINT('Ctrl Pts',(1.62382106309547,22.2199999999995,-8.18876435835048));
#13011=CARTESIAN_POINT('Ctrl Pts',(1.39036720391674,22.22,-8.22145831436959));
#13012=CARTESIAN_POINT('Ctrl Pts',(1.15457232288596,22.22,-8.24555872886889));
#13013=CARTESIAN_POINT('',(4.50738083181344,22.22,8.84193633985987));
#13014=CARTESIAN_POINT('Ctrl Pts',(4.50738083181345,22.22,8.84193633985991));
#13015=CARTESIAN_POINT('Ctrl Pts',(5.50129019941128,22.22,8.24752673459274));
#13016=CARTESIAN_POINT('Ctrl Pts',(6.38273063962348,22.22,7.48282682306534));
#13017=CARTESIAN_POINT('Ctrl Pts',(7.72906558127775,22.22,5.82007728703888));
#13018=CARTESIAN_POINT('Ctrl Pts',(8.42964347032215,22.2199999999936,4.72920057212043));
#13019=CARTESIAN_POINT('Ctrl Pts',(9.2043748646196,22.2199999999936,2.1387789590176));
#13020=CARTESIAN_POINT('Ctrl Pts',(9.31838831238722,22.22,0.915490022079924));
#13021=CARTESIAN_POINT('Ctrl Pts',(9.06300659638671,22.22,-1.507993106964));
#13022=CARTESIAN_POINT('Ctrl Pts',(8.69486484793729,22.22,-2.68367031517768));
#13023=CARTESIAN_POINT('Ctrl Pts',(7.55278087878453,22.22,-4.76564642192656));
#13024=CARTESIAN_POINT('Ctrl Pts',(6.81838193887901,22.219999999987,-5.65268890498168));
#13025=CARTESIAN_POINT('Ctrl Pts',(5.41795245135685,22.219999999987,-6.76839622139175));
#13026=CARTESIAN_POINT('Ctrl Pts',(4.87996243897349,22.2199999976409,-7.10670058837755));
#13027=CARTESIAN_POINT('Ctrl Pts',(3.74918166874661,22.2199999976409,-7.65278819993115));
#13028=CARTESIAN_POINT('Ctrl Pts',(3.16100732091391,22.22,-7.86114610599102));
#13029=CARTESIAN_POINT('Ctrl Pts',(2.55537495509677,22.22,-8.00360031633713));
#13030=CARTESIAN_POINT('',(-7.96780251527898,22.22,-2.66489817109789));
#13031=CARTESIAN_POINT('Ctrl Pts',(-7.96780251527902,22.22,-2.66489817109774));
#13032=CARTESIAN_POINT('Ctrl Pts',(-8.23599312974415,22.22,-2.02792425502546));
#13033=CARTESIAN_POINT('Ctrl Pts',(-8.4263439618362,22.22,-1.36096366704832));
#13034=CARTESIAN_POINT('Ctrl Pts',(-8.64297828766049,22.22,0.00360816572491401));
#13035=CARTESIAN_POINT('Ctrl Pts',(-8.66859900866027,22.22,0.696135165601527));
#13036=CARTESIAN_POINT('Ctrl Pts',(-8.52525050570627,22.22,2.41043360782728));
#13037=CARTESIAN_POINT('Ctrl Pts',(-8.255689969321,22.2199999999164,3.41277917262433));
#13038=CARTESIAN_POINT('Ctrl Pts',(-7.37169226325107,22.2199999999164,5.28253364315786));
#13039=CARTESIAN_POINT('Ctrl Pts',(-6.69159903012222,22.2199999999999,6.31291964415821));
#13040=CARTESIAN_POINT('Ctrl Pts',(-4.74829296569674,22.2199999999999,8.0685409876383));
#13041=CARTESIAN_POINT('Ctrl Pts',(-3.68909457138914,22.22,8.69991320242805));
#13042=CARTESIAN_POINT('Ctrl Pts',(-1.08588604419115,22.22,9.62226726459541));
#13043=CARTESIAN_POINT('Ctrl Pts',(0.195202339552547,22.22,9.67166205579421));
#13044=CARTESIAN_POINT('Ctrl Pts',(2.25253429025285,22.22,9.57488020226816));
#13045=CARTESIAN_POINT('Ctrl Pts',(3.41720895858078,22.22,9.30785410203658));
#13046=CARTESIAN_POINT('Ctrl Pts',(4.50738083181195,22.22,8.84193633986044));
#13047=CARTESIAN_POINT('Ctrl Pts',(-7.30706743901568,22.22,-3.99112032412916));
#13048=CARTESIAN_POINT('Ctrl Pts',(-7.43302521096891,22.22,-3.77868598418148));
#13049=CARTESIAN_POINT('Ctrl Pts',(-7.54996154878007,22.2200000000004,-3.56259441822855));
#13050=CARTESIAN_POINT('Ctrl Pts',(-7.77060228250538,22.2200000000004,-3.1175628528368));
#13051=CARTESIAN_POINT('Ctrl Pts',(-7.86861240549784,22.22,-2.90048252511764));
#13052=CARTESIAN_POINT('Ctrl Pts',(-7.96780251527901,22.22,-2.66489817109778));
#13053=CARTESIAN_POINT('Ctrl Pts',(-1.78726082715848E-11,-144.88675111262,
-9.92453123331945));
#13054=CARTESIAN_POINT('Ctrl Pts',(-5.7299307791557,-144.71175111262,-9.92453123330913));
#13055=CARTESIAN_POINT('Ctrl Pts',(-8.59489616871569,-144.53675111262,-4.96226561664425));
#13056=CARTESIAN_POINT('Ctrl Pts',(-11.4598615582757,-144.36175111262,2.06368086793017E-11));
#13057=CARTESIAN_POINT('Ctrl Pts',(-8.59489616869782,-144.18675111262,4.9622656166752));
#13058=CARTESIAN_POINT('Ctrl Pts',(-5.72993077911996,-144.01175111262,9.92453123332977));
#13059=CARTESIAN_POINT('Ctrl Pts',(1.7871392867044E-11,-143.83675111262,
9.92453123331945));
#13060=CARTESIAN_POINT('Ctrl Pts',(5.7299307791557,-143.66175111262,9.92453123330913));
#13061=CARTESIAN_POINT('Ctrl Pts',(8.59489616871569,-143.48675111262,4.96226561664425));
#13062=CARTESIAN_POINT('Ctrl Pts',(11.4598615582757,-143.31175111262,-2.06354052510241E-11));
#13063=CARTESIAN_POINT('Ctrl Pts',(8.59489616869782,-143.13675111262,-4.9622656166752));
#13064=CARTESIAN_POINT('Ctrl Pts',(5.72993077911996,-142.96175111262,-9.92453123332976));
#13065=CARTESIAN_POINT('Ctrl Pts',(-1.78726082715848E-11,-142.78675111262,
-9.92453123331945));
#13066=CARTESIAN_POINT('Ctrl Pts',(-5.7299307791557,-142.61175111262,-9.92453123330913));
#13067=CARTESIAN_POINT('Ctrl Pts',(-8.59489616871569,-142.43675111262,-4.96226561664425));
#13068=CARTESIAN_POINT('Ctrl Pts',(-11.4598615582757,-142.26175111262,2.06368086793017E-11));
#13069=CARTESIAN_POINT('Ctrl Pts',(-8.59489616869782,-142.08675111262,4.9622656166752));
#13070=CARTESIAN_POINT('Ctrl Pts',(-5.72993077911996,-141.91175111262,9.92453123332977));
#13071=CARTESIAN_POINT('Ctrl Pts',(1.7871392867044E-11,-141.73675111262,
9.92453123331945));
#13072=CARTESIAN_POINT('Ctrl Pts',(5.7299307791557,-141.56175111262,9.92453123330913));
#13073=CARTESIAN_POINT('Ctrl Pts',(8.59489616871569,-141.38675111262,4.96226561664425));
#13074=CARTESIAN_POINT('Ctrl Pts',(11.4598615582757,-141.21175111262,-2.06354052510241E-11));
#13075=CARTESIAN_POINT('Ctrl Pts',(8.59489616869782,-141.03675111262,-4.9622656166752));
#13076=CARTESIAN_POINT('Ctrl Pts',(5.72993077911996,-140.86175111262,-9.92453123332976));
#13077=CARTESIAN_POINT('Ctrl Pts',(-1.78726082715848E-11,-140.68675111262,
-9.92453123331945));
#13078=CARTESIAN_POINT('Ctrl Pts',(-5.7299307791557,-140.51175111262,-9.92453123330913));
#13079=CARTESIAN_POINT('Ctrl Pts',(-8.59489616871569,-140.33675111262,-4.96226561664425));
#13080=CARTESIAN_POINT('Ctrl Pts',(-11.4598615582757,-140.16175111262,2.06368086793017E-11));
#13081=CARTESIAN_POINT('Ctrl Pts',(-8.59489616869782,-139.98675111262,4.9622656166752));
#13082=CARTESIAN_POINT('Ctrl Pts',(-5.72993077911996,-139.81175111262,9.92453123332977));
#13083=CARTESIAN_POINT('Ctrl Pts',(1.7871392867044E-11,-139.63675111262,
9.92453123331945));
#13084=CARTESIAN_POINT('Ctrl Pts',(5.7299307791557,-139.46175111262,9.92453123330913));
#13085=CARTESIAN_POINT('Ctrl Pts',(8.59489616871569,-139.28675111262,4.96226561664425));
#13086=CARTESIAN_POINT('Ctrl Pts',(11.4598615582757,-139.11175111262,-2.06354052510241E-11));
#13087=CARTESIAN_POINT('Ctrl Pts',(8.59489616869782,-138.93675111262,-4.9622656166752));
#13088=CARTESIAN_POINT('Ctrl Pts',(5.72993077911996,-138.76175111262,-9.92453123332976));
#13089=CARTESIAN_POINT('Ctrl Pts',(-1.78726082715848E-11,-138.58675111262,
-9.92453123331945));
#13090=CARTESIAN_POINT('Ctrl Pts',(-5.7299307791557,-138.41175111262,-9.92453123330913));
#13091=CARTESIAN_POINT('Ctrl Pts',(-8.59489616871569,-138.23675111262,-4.96226561664425));
#13092=CARTESIAN_POINT('Ctrl Pts',(-11.4598615582757,-138.06175111262,2.06368086793017E-11));
#13093=CARTESIAN_POINT('Ctrl Pts',(-8.59489616869782,-137.88675111262,4.9622656166752));
#13094=CARTESIAN_POINT('Ctrl Pts',(-5.72993077911996,-137.71175111262,9.92453123332977));
#13095=CARTESIAN_POINT('Ctrl Pts',(1.7871392867044E-11,-137.53675111262,
9.92453123331945));
#13096=CARTESIAN_POINT('Ctrl Pts',(5.7299307791557,-137.36175111262,9.92453123330913));
#13097=CARTESIAN_POINT('Ctrl Pts',(8.59489616871569,-137.18675111262,4.96226561664425));
#13098=CARTESIAN_POINT('Ctrl Pts',(11.4598615582757,-137.01175111262,-2.06354052510241E-11));
#13099=CARTESIAN_POINT('Ctrl Pts',(8.59489616869782,-136.83675111262,-4.9622656166752));
#13100=CARTESIAN_POINT('Ctrl Pts',(5.72993077911996,-136.66175111262,-9.92453123332976));
#13101=CARTESIAN_POINT('Ctrl Pts',(-1.78726082715848E-11,-136.48675111262,
-9.92453123331945));
#13102=CARTESIAN_POINT('Ctrl Pts',(-5.7299307791557,-136.31175111262,-9.92453123330913));
#13103=CARTESIAN_POINT('Ctrl Pts',(-8.59489616871569,-136.13675111262,-4.96226561664425));
#13104=CARTESIAN_POINT('Ctrl Pts',(-11.4598615582757,-135.96175111262,2.06368086793017E-11));
#13105=CARTESIAN_POINT('Ctrl Pts',(-8.59489616869782,-135.78675111262,4.9622656166752));
#13106=CARTESIAN_POINT('Ctrl Pts',(-5.72993077911996,-135.61175111262,9.92453123332977));
#13107=CARTESIAN_POINT('Ctrl Pts',(1.7871392867044E-11,-135.43675111262,
9.92453123331945));
#13108=CARTESIAN_POINT('Ctrl Pts',(5.7299307791557,-135.26175111262,9.92453123330913));
#13109=CARTESIAN_POINT('Ctrl Pts',(8.59489616871569,-135.08675111262,4.96226561664425));
#13110=CARTESIAN_POINT('Ctrl Pts',(11.4598615582757,-134.91175111262,-2.06354052510241E-11));
#13111=CARTESIAN_POINT('Ctrl Pts',(8.59489616869782,-134.73675111262,-4.9622656166752));
#13112=CARTESIAN_POINT('Ctrl Pts',(5.72993077911996,-134.56175111262,-9.92453123332976));
#13113=CARTESIAN_POINT('Ctrl Pts',(-1.78726082715848E-11,-134.38675111262,
-9.92453123331945));
#13114=CARTESIAN_POINT('Ctrl Pts',(-5.7299307791557,-134.21175111262,-9.92453123330913));
#13115=CARTESIAN_POINT('Ctrl Pts',(-8.59489616871569,-134.03675111262,-4.96226561664425));
#13116=CARTESIAN_POINT('Ctrl Pts',(-11.4598615582757,-133.86175111262,2.06368086793017E-11));
#13117=CARTESIAN_POINT('Ctrl Pts',(-8.59489616869782,-133.68675111262,4.9622656166752));
#13118=CARTESIAN_POINT('Ctrl Pts',(-5.72993077911996,-133.51175111262,9.92453123332977));
#13119=CARTESIAN_POINT('Ctrl Pts',(1.7871392867044E-11,-133.33675111262,
9.92453123331945));
#13120=CARTESIAN_POINT('Ctrl Pts',(5.7299307791557,-133.16175111262,9.92453123330913));
#13121=CARTESIAN_POINT('Ctrl Pts',(8.59489616871569,-132.98675111262,4.96226561664425));
#13122=CARTESIAN_POINT('Ctrl Pts',(11.4598615582757,-132.81175111262,-2.06354052510241E-11));
#13123=CARTESIAN_POINT('Ctrl Pts',(8.59489616869782,-132.63675111262,-4.9622656166752));
#13124=CARTESIAN_POINT('Ctrl Pts',(5.72993077911996,-132.46175111262,-9.92453123332976));
#13125=CARTESIAN_POINT('Ctrl Pts',(-1.78726082715848E-11,-132.28675111262,
-9.92453123331945));
#13126=CARTESIAN_POINT('Ctrl Pts',(-5.7299307791557,-132.11175111262,-9.92453123330913));
#13127=CARTESIAN_POINT('Ctrl Pts',(-8.59489616871569,-131.93675111262,-4.96226561664425));
#13128=CARTESIAN_POINT('Ctrl Pts',(-11.4598615582757,-131.76175111262,2.06368086793017E-11));
#13129=CARTESIAN_POINT('Ctrl Pts',(-8.59489616869782,-131.58675111262,4.9622656166752));
#13130=CARTESIAN_POINT('Ctrl Pts',(-5.72993077911996,-131.41175111262,9.92453123332977));
#13131=CARTESIAN_POINT('Ctrl Pts',(1.7871392867044E-11,-131.23675111262,
9.92453123331945));
#13132=CARTESIAN_POINT('Ctrl Pts',(5.7299307791557,-131.06175111262,9.92453123330913));
#13133=CARTESIAN_POINT('Ctrl Pts',(8.59489616871569,-130.88675111262,4.96226561664425));
#13134=CARTESIAN_POINT('Ctrl Pts',(11.4598615582757,-130.71175111262,-2.06354052510241E-11));
#13135=CARTESIAN_POINT('Ctrl Pts',(8.59489616869782,-130.53675111262,-4.9622656166752));
#13136=CARTESIAN_POINT('Ctrl Pts',(5.72993077911996,-130.36175111262,-9.92453123332976));
#13137=CARTESIAN_POINT('Ctrl Pts',(-1.78726082715848E-11,-130.18675111262,
-9.92453123331945));
#13138=CARTESIAN_POINT('Ctrl Pts',(-5.7299307791557,-130.01175111262,-9.92453123330913));
#13139=CARTESIAN_POINT('Ctrl Pts',(-8.59489616871569,-129.83675111262,-4.96226561664425));
#13140=CARTESIAN_POINT('Ctrl Pts',(-11.4598615582757,-129.66175111262,2.06368086793017E-11));
#13141=CARTESIAN_POINT('Ctrl Pts',(-8.59489616869782,-129.48675111262,4.9622656166752));
#13142=CARTESIAN_POINT('Ctrl Pts',(-5.72993077911996,-129.31175111262,9.92453123332977));
#13143=CARTESIAN_POINT('Ctrl Pts',(1.7871392867044E-11,-129.13675111262,
9.92453123331945));
#13144=CARTESIAN_POINT('Ctrl Pts',(5.7299307791557,-128.96175111262,9.92453123330913));
#13145=CARTESIAN_POINT('Ctrl Pts',(8.59489616871569,-128.78675111262,4.96226561664425));
#13146=CARTESIAN_POINT('Ctrl Pts',(11.4598615582757,-128.61175111262,-2.06354052510241E-11));
#13147=CARTESIAN_POINT('Ctrl Pts',(8.59489616869782,-128.43675111262,-4.9622656166752));
#13148=CARTESIAN_POINT('Ctrl Pts',(5.72993077911996,-128.26175111262,-9.92453123332976));
#13149=CARTESIAN_POINT('Ctrl Pts',(-1.78726082715848E-11,-128.08675111262,
-9.92453123331945));
#13150=CARTESIAN_POINT('Ctrl Pts',(-5.7299307791557,-127.91175111262,-9.92453123330913));
#13151=CARTESIAN_POINT('Ctrl Pts',(-8.59489616871569,-127.73675111262,-4.96226561664425));
#13152=CARTESIAN_POINT('Ctrl Pts',(-11.4598615582757,-127.56175111262,2.06368086793017E-11));
#13153=CARTESIAN_POINT('Ctrl Pts',(-8.59489616869782,-127.38675111262,4.9622656166752));
#13154=CARTESIAN_POINT('Ctrl Pts',(-5.72993077911996,-127.21175111262,9.92453123332977));
#13155=CARTESIAN_POINT('Ctrl Pts',(1.7871392867044E-11,-127.03675111262,
9.92453123331945));
#13156=CARTESIAN_POINT('Ctrl Pts',(5.7299307791557,-126.86175111262,9.92453123330913));
#13157=CARTESIAN_POINT('Ctrl Pts',(8.59489616871569,-126.68675111262,4.96226561664425));
#13158=CARTESIAN_POINT('Ctrl Pts',(11.4598615582757,-126.51175111262,-2.06354052510241E-11));
#13159=CARTESIAN_POINT('Ctrl Pts',(8.59489616869782,-126.33675111262,-4.9622656166752));
#13160=CARTESIAN_POINT('Ctrl Pts',(5.72993077911996,-126.16175111262,-9.92453123332976));
#13161=CARTESIAN_POINT('Ctrl Pts',(-1.78726082715848E-11,-125.98675111262,
-9.92453123331945));
#13162=CARTESIAN_POINT('Ctrl Pts',(-5.7299307791557,-125.81175111262,-9.92453123330913));
#13163=CARTESIAN_POINT('Ctrl Pts',(-8.59489616871569,-125.63675111262,-4.96226561664425));
#13164=CARTESIAN_POINT('Ctrl Pts',(-11.4598615582757,-125.46175111262,2.06368086793017E-11));
#13165=CARTESIAN_POINT('Ctrl Pts',(-8.59489616869782,-125.28675111262,4.9622656166752));
#13166=CARTESIAN_POINT('Ctrl Pts',(-5.72993077911996,-125.11175111262,9.92453123332977));
#13167=CARTESIAN_POINT('Ctrl Pts',(1.7871392867044E-11,-124.93675111262,
9.92453123331945));
#13168=CARTESIAN_POINT('Ctrl Pts',(5.7299307791557,-124.76175111262,9.92453123330913));
#13169=CARTESIAN_POINT('Ctrl Pts',(8.59489616871569,-124.58675111262,4.96226561664425));
#13170=CARTESIAN_POINT('Ctrl Pts',(11.4598615582757,-124.41175111262,-2.06354052510241E-11));
#13171=CARTESIAN_POINT('Ctrl Pts',(8.59489616869782,-124.23675111262,-4.9622656166752));
#13172=CARTESIAN_POINT('Ctrl Pts',(5.72993077911996,-124.06175111262,-9.92453123332976));
#13173=CARTESIAN_POINT('Ctrl Pts',(-1.78726082715848E-11,-123.88675111262,
-9.92453123331945));
#13174=CARTESIAN_POINT('Ctrl Pts',(-5.7299307791557,-123.71175111262,-9.92453123330913));
#13175=CARTESIAN_POINT('Ctrl Pts',(-8.59489616871569,-123.53675111262,-4.96226561664425));
#13176=CARTESIAN_POINT('Ctrl Pts',(-11.4598615582757,-123.36175111262,2.06368086793017E-11));
#13177=CARTESIAN_POINT('Ctrl Pts',(-8.59489616869782,-123.18675111262,4.9622656166752));
#13178=CARTESIAN_POINT('Ctrl Pts',(-5.72993077911996,-123.01175111262,9.92453123332977));
#13179=CARTESIAN_POINT('Ctrl Pts',(1.7871392867044E-11,-122.83675111262,
9.92453123331945));
#13180=CARTESIAN_POINT('Ctrl Pts',(5.7299307791557,-122.66175111262,9.92453123330913));
#13181=CARTESIAN_POINT('Ctrl Pts',(8.59489616871569,-122.48675111262,4.96226561664425));
#13182=CARTESIAN_POINT('Ctrl Pts',(11.4598615582757,-122.31175111262,-2.06354052510241E-11));
#13183=CARTESIAN_POINT('Ctrl Pts',(8.59489616869782,-122.13675111262,-4.9622656166752));
#13184=CARTESIAN_POINT('Ctrl Pts',(5.72993077911996,-121.96175111262,-9.92453123332976));
#13185=CARTESIAN_POINT('Ctrl Pts',(-1.78726082715848E-11,-121.78675111262,
-9.92453123331945));
#13186=CARTESIAN_POINT('Ctrl Pts',(-5.7299307791557,-121.61175111262,-9.92453123330913));
#13187=CARTESIAN_POINT('Ctrl Pts',(-8.59489616871569,-121.43675111262,-4.96226561664425));
#13188=CARTESIAN_POINT('Ctrl Pts',(-11.4598615582757,-121.26175111262,2.06368086793017E-11));
#13189=CARTESIAN_POINT('Ctrl Pts',(-8.59489616869782,-121.08675111262,4.9622656166752));
#13190=CARTESIAN_POINT('Ctrl Pts',(-5.72993077911996,-120.91175111262,9.92453123332977));
#13191=CARTESIAN_POINT('Ctrl Pts',(1.7871392867044E-11,-120.73675111262,
9.92453123331945));
#13192=CARTESIAN_POINT('Ctrl Pts',(5.7299307791557,-120.56175111262,9.92453123330913));
#13193=CARTESIAN_POINT('Ctrl Pts',(8.59489616871569,-120.38675111262,4.96226561664425));
#13194=CARTESIAN_POINT('Ctrl Pts',(11.4598615582757,-120.21175111262,-2.06354052510241E-11));
#13195=CARTESIAN_POINT('Ctrl Pts',(8.59489616869782,-120.03675111262,-4.9622656166752));
#13196=CARTESIAN_POINT('Ctrl Pts',(5.72993077911996,-119.86175111262,-9.92453123332976));
#13197=CARTESIAN_POINT('Ctrl Pts',(-1.78726082715848E-11,-119.68675111262,
-9.92453123331945));
#13198=CARTESIAN_POINT('Ctrl Pts',(-5.7299307791557,-119.51175111262,-9.92453123330913));
#13199=CARTESIAN_POINT('Ctrl Pts',(-8.59489616871569,-119.33675111262,-4.96226561664425));
#13200=CARTESIAN_POINT('Ctrl Pts',(-11.4598615582757,-119.16175111262,2.06368086793017E-11));
#13201=CARTESIAN_POINT('Ctrl Pts',(-8.59489616869782,-118.98675111262,4.9622656166752));
#13202=CARTESIAN_POINT('Ctrl Pts',(-5.72993077911996,-118.81175111262,9.92453123332977));
#13203=CARTESIAN_POINT('Ctrl Pts',(1.7871392867044E-11,-118.63675111262,
9.92453123331945));
#13204=CARTESIAN_POINT('Ctrl Pts',(5.7299307791557,-118.46175111262,9.92453123330913));
#13205=CARTESIAN_POINT('Ctrl Pts',(8.59489616871569,-118.28675111262,4.96226561664425));
#13206=CARTESIAN_POINT('Ctrl Pts',(11.4598615582757,-118.11175111262,-2.06354052510241E-11));
#13207=CARTESIAN_POINT('Ctrl Pts',(8.59489616869782,-117.93675111262,-4.9622656166752));
#13208=CARTESIAN_POINT('Ctrl Pts',(5.72993077911996,-117.76175111262,-9.92453123332976));
#13209=CARTESIAN_POINT('Ctrl Pts',(-1.78726082715848E-11,-117.58675111262,
-9.92453123331945));
#13210=CARTESIAN_POINT('Ctrl Pts',(-5.7299307791557,-117.41175111262,-9.92453123330913));
#13211=CARTESIAN_POINT('Ctrl Pts',(-8.59489616871569,-117.23675111262,-4.96226561664425));
#13212=CARTESIAN_POINT('Ctrl Pts',(-11.4598615582757,-117.06175111262,2.06368086793017E-11));
#13213=CARTESIAN_POINT('Ctrl Pts',(-8.59489616869782,-116.88675111262,4.9622656166752));
#13214=CARTESIAN_POINT('Ctrl Pts',(-5.72993077911996,-116.71175111262,9.92453123332977));
#13215=CARTESIAN_POINT('Ctrl Pts',(1.7871392867044E-11,-116.53675111262,
9.92453123331945));
#13216=CARTESIAN_POINT('Ctrl Pts',(5.7299307791557,-116.36175111262,9.92453123330913));
#13217=CARTESIAN_POINT('Ctrl Pts',(8.59489616871569,-116.18675111262,4.96226561664425));
#13218=CARTESIAN_POINT('Ctrl Pts',(11.4598615582757,-116.01175111262,-2.06354052510241E-11));
#13219=CARTESIAN_POINT('Ctrl Pts',(8.59489616869782,-115.83675111262,-4.9622656166752));
#13220=CARTESIAN_POINT('Ctrl Pts',(5.72993077911996,-115.66175111262,-9.92453123332976));
#13221=CARTESIAN_POINT('Ctrl Pts',(-1.78726082715848E-11,-115.48675111262,
-9.92453123331945));
#13222=CARTESIAN_POINT('Ctrl Pts',(-5.7299307791557,-115.31175111262,-9.92453123330913));
#13223=CARTESIAN_POINT('Ctrl Pts',(-8.59489616871569,-115.13675111262,-4.96226561664425));
#13224=CARTESIAN_POINT('Ctrl Pts',(-11.4598615582757,-114.96175111262,2.06368086793017E-11));
#13225=CARTESIAN_POINT('Ctrl Pts',(-8.59489616869782,-114.78675111262,4.9622656166752));
#13226=CARTESIAN_POINT('Ctrl Pts',(-5.72993077911996,-114.61175111262,9.92453123332977));
#13227=CARTESIAN_POINT('Ctrl Pts',(1.7871392867044E-11,-114.43675111262,
9.92453123331945));
#13228=CARTESIAN_POINT('Ctrl Pts',(5.7299307791557,-114.26175111262,9.92453123330913));
#13229=CARTESIAN_POINT('Ctrl Pts',(8.59489616871569,-114.08675111262,4.96226561664425));
#13230=CARTESIAN_POINT('Ctrl Pts',(11.4598615582757,-113.91175111262,-2.06354052510241E-11));
#13231=CARTESIAN_POINT('Ctrl Pts',(8.59489616869782,-113.73675111262,-4.9622656166752));
#13232=CARTESIAN_POINT('Ctrl Pts',(5.72993077911996,-113.56175111262,-9.92453123332976));
#13233=CARTESIAN_POINT('Ctrl Pts',(-1.78726082715848E-11,-113.38675111262,
-9.92453123331945));
#13234=CARTESIAN_POINT('Ctrl Pts',(-5.7299307791557,-113.21175111262,-9.92453123330913));
#13235=CARTESIAN_POINT('Ctrl Pts',(-8.59489616871569,-113.03675111262,-4.96226561664425));
#13236=CARTESIAN_POINT('Ctrl Pts',(-11.4598615582757,-112.86175111262,2.06368086793017E-11));
#13237=CARTESIAN_POINT('Ctrl Pts',(-8.59489616869782,-112.68675111262,4.9622656166752));
#13238=CARTESIAN_POINT('Ctrl Pts',(-5.72993077911996,-112.51175111262,9.92453123332977));
#13239=CARTESIAN_POINT('Ctrl Pts',(1.7871392867044E-11,-112.33675111262,
9.92453123331945));
#13240=CARTESIAN_POINT('Ctrl Pts',(5.7299307791557,-112.16175111262,9.92453123330913));
#13241=CARTESIAN_POINT('Ctrl Pts',(8.59489616871569,-111.98675111262,4.96226561664425));
#13242=CARTESIAN_POINT('Ctrl Pts',(11.4598615582757,-111.81175111262,-2.06354052510241E-11));
#13243=CARTESIAN_POINT('Ctrl Pts',(8.59489616869782,-111.63675111262,-4.9622656166752));
#13244=CARTESIAN_POINT('Ctrl Pts',(5.72993077911996,-111.46175111262,-9.92453123332976));
#13245=CARTESIAN_POINT('Ctrl Pts',(-1.78726082715848E-11,-111.28675111262,
-9.92453123331945));
#13246=CARTESIAN_POINT('Ctrl Pts',(-5.7299307791557,-111.11175111262,-9.92453123330913));
#13247=CARTESIAN_POINT('Ctrl Pts',(-8.59489616871569,-110.93675111262,-4.96226561664425));
#13248=CARTESIAN_POINT('Ctrl Pts',(-11.4598615582757,-110.76175111262,2.06368086793017E-11));
#13249=CARTESIAN_POINT('Ctrl Pts',(-8.59489616869782,-110.58675111262,4.9622656166752));
#13250=CARTESIAN_POINT('Ctrl Pts',(-5.72993077911996,-110.41175111262,9.92453123332977));
#13251=CARTESIAN_POINT('Ctrl Pts',(1.7871392867044E-11,-110.23675111262,
9.92453123331945));
#13252=CARTESIAN_POINT('Ctrl Pts',(5.7299307791557,-110.06175111262,9.92453123330913));
#13253=CARTESIAN_POINT('Ctrl Pts',(8.59489616871569,-109.88675111262,4.96226561664425));
#13254=CARTESIAN_POINT('Ctrl Pts',(11.4598615582757,-109.71175111262,-2.06354052510241E-11));
#13255=CARTESIAN_POINT('Ctrl Pts',(8.59489616869782,-109.53675111262,-4.9622656166752));
#13256=CARTESIAN_POINT('Ctrl Pts',(5.72993077911996,-109.36175111262,-9.92453123332976));
#13257=CARTESIAN_POINT('Ctrl Pts',(-1.78726082715848E-11,-109.18675111262,
-9.92453123331945));
#13258=CARTESIAN_POINT('Ctrl Pts',(-5.7299307791557,-109.01175111262,-9.92453123330913));
#13259=CARTESIAN_POINT('Ctrl Pts',(-8.59489616871569,-108.83675111262,-4.96226561664425));
#13260=CARTESIAN_POINT('Ctrl Pts',(-11.4598615582757,-108.66175111262,2.06368086793017E-11));
#13261=CARTESIAN_POINT('Ctrl Pts',(-8.59489616869782,-108.48675111262,4.9622656166752));
#13262=CARTESIAN_POINT('Ctrl Pts',(-5.72993077911996,-108.31175111262,9.92453123332977));
#13263=CARTESIAN_POINT('Ctrl Pts',(1.7871392867044E-11,-108.13675111262,
9.92453123331945));
#13264=CARTESIAN_POINT('Ctrl Pts',(5.7299307791557,-107.96175111262,9.92453123330913));
#13265=CARTESIAN_POINT('Ctrl Pts',(8.59489616871569,-107.78675111262,4.96226561664425));
#13266=CARTESIAN_POINT('Ctrl Pts',(11.4598615582757,-107.61175111262,-2.06354052510241E-11));
#13267=CARTESIAN_POINT('Ctrl Pts',(8.59489616869782,-107.43675111262,-4.9622656166752));
#13268=CARTESIAN_POINT('Ctrl Pts',(5.72993077911996,-107.26175111262,-9.92453123332976));
#13269=CARTESIAN_POINT('Ctrl Pts',(-1.78726082715848E-11,-107.08675111262,
-9.92453123331945));
#13270=CARTESIAN_POINT('Ctrl Pts',(-5.7299307791557,-106.91175111262,-9.92453123330913));
#13271=CARTESIAN_POINT('Ctrl Pts',(-8.59489616871569,-106.73675111262,-4.96226561664425));
#13272=CARTESIAN_POINT('Ctrl Pts',(-11.4598615582757,-106.56175111262,2.06368086793017E-11));
#13273=CARTESIAN_POINT('Ctrl Pts',(-8.59489616869782,-106.38675111262,4.9622656166752));
#13274=CARTESIAN_POINT('Ctrl Pts',(-5.72993077911996,-106.21175111262,9.92453123332977));
#13275=CARTESIAN_POINT('Ctrl Pts',(1.7871392867044E-11,-106.03675111262,
9.92453123331945));
#13276=CARTESIAN_POINT('Ctrl Pts',(5.7299307791557,-105.86175111262,9.92453123330913));
#13277=CARTESIAN_POINT('Ctrl Pts',(8.59489616871569,-105.68675111262,4.96226561664425));
#13278=CARTESIAN_POINT('Ctrl Pts',(11.4598615582757,-105.51175111262,-2.06354052510241E-11));
#13279=CARTESIAN_POINT('Ctrl Pts',(8.59489616869782,-105.33675111262,-4.9622656166752));
#13280=CARTESIAN_POINT('Ctrl Pts',(5.72993077911996,-105.16175111262,-9.92453123332976));
#13281=CARTESIAN_POINT('Ctrl Pts',(-1.78726082715848E-11,-104.98675111262,
-9.92453123331945));
#13282=CARTESIAN_POINT('Ctrl Pts',(-5.7299307791557,-104.81175111262,-9.92453123330913));
#13283=CARTESIAN_POINT('Ctrl Pts',(-8.59489616871569,-104.63675111262,-4.96226561664425));
#13284=CARTESIAN_POINT('Ctrl Pts',(-11.4598615582757,-104.46175111262,2.06368086793017E-11));
#13285=CARTESIAN_POINT('Ctrl Pts',(-8.59489616869782,-104.28675111262,4.9622656166752));
#13286=CARTESIAN_POINT('Ctrl Pts',(-5.72993077911996,-104.11175111262,9.92453123332977));
#13287=CARTESIAN_POINT('Ctrl Pts',(1.7871392867044E-11,-103.93675111262,
9.92453123331945));
#13288=CARTESIAN_POINT('Ctrl Pts',(5.7299307791557,-103.76175111262,9.92453123330913));
#13289=CARTESIAN_POINT('Ctrl Pts',(8.59489616871569,-103.58675111262,4.96226561664425));
#13290=CARTESIAN_POINT('Ctrl Pts',(11.4598615582757,-103.41175111262,-2.06354052510241E-11));
#13291=CARTESIAN_POINT('Ctrl Pts',(8.59489616869782,-103.23675111262,-4.9622656166752));
#13292=CARTESIAN_POINT('Ctrl Pts',(5.72993077911996,-103.06175111262,-9.92453123332976));
#13293=CARTESIAN_POINT('Ctrl Pts',(-1.78726082715848E-11,-102.88675111262,
-9.92453123331945));
#13294=CARTESIAN_POINT('Ctrl Pts',(-5.7299307791557,-102.71175111262,-9.92453123330913));
#13295=CARTESIAN_POINT('Ctrl Pts',(-8.59489616871569,-102.53675111262,-4.96226561664425));
#13296=CARTESIAN_POINT('Ctrl Pts',(-11.4598615582757,-102.36175111262,2.06368086793017E-11));
#13297=CARTESIAN_POINT('Ctrl Pts',(-8.59489616869782,-102.18675111262,4.9622656166752));
#13298=CARTESIAN_POINT('Ctrl Pts',(-5.72993077911996,-102.01175111262,9.92453123332977));
#13299=CARTESIAN_POINT('Ctrl Pts',(1.7871392867044E-11,-101.83675111262,
9.92453123331945));
#13300=CARTESIAN_POINT('Ctrl Pts',(5.7299307791557,-101.66175111262,9.92453123330913));
#13301=CARTESIAN_POINT('Ctrl Pts',(8.59489616871569,-101.48675111262,4.96226561664425));
#13302=CARTESIAN_POINT('Ctrl Pts',(11.4598615582757,-101.31175111262,-2.06354052510241E-11));
#13303=CARTESIAN_POINT('Ctrl Pts',(8.59489616869782,-101.13675111262,-4.9622656166752));
#13304=CARTESIAN_POINT('Ctrl Pts',(5.72993077911996,-100.96175111262,-9.92453123332976));
#13305=CARTESIAN_POINT('Ctrl Pts',(-1.78726082715848E-11,-100.78675111262,
-9.92453123331945));
#13306=CARTESIAN_POINT('Ctrl Pts',(-5.7299307791557,-100.61175111262,-9.92453123330913));
#13307=CARTESIAN_POINT('Ctrl Pts',(-8.59489616871569,-100.43675111262,-4.96226561664425));
#13308=CARTESIAN_POINT('Ctrl Pts',(-11.4598615582757,-100.26175111262,2.06368086793017E-11));
#13309=CARTESIAN_POINT('Ctrl Pts',(-8.59489616869782,-100.08675111262,4.9622656166752));
#13310=CARTESIAN_POINT('Ctrl Pts',(-5.72993077911996,-99.91175111262,9.92453123332977));
#13311=CARTESIAN_POINT('Ctrl Pts',(1.7871392867044E-11,-99.7367511126201,
9.92453123331945));
#13312=CARTESIAN_POINT('Ctrl Pts',(5.7299307791557,-99.5617511126201,9.92453123330913));
#13313=CARTESIAN_POINT('Ctrl Pts',(8.59489616871569,-99.3867511126201,4.96226561664425));
#13314=CARTESIAN_POINT('Ctrl Pts',(11.4598615582757,-99.2117511126201,-2.06354052510241E-11));
#13315=CARTESIAN_POINT('Ctrl Pts',(8.59489616869782,-99.0367511126201,-4.9622656166752));
#13316=CARTESIAN_POINT('Ctrl Pts',(5.72993077911996,-98.8617511126201,-9.92453123332976));
#13317=CARTESIAN_POINT('Ctrl Pts',(-1.78726082715848E-11,-98.6867511126201,
-9.92453123331945));
#13318=CARTESIAN_POINT('Ctrl Pts',(-5.7299307791557,-98.5117511126201,-9.92453123330913));
#13319=CARTESIAN_POINT('Ctrl Pts',(-8.59489616871569,-98.33675111262,-4.96226561664425));
#13320=CARTESIAN_POINT('Ctrl Pts',(-11.4598615582757,-98.16175111262,2.06368086793017E-11));
#13321=CARTESIAN_POINT('Ctrl Pts',(-8.59489616869782,-97.9867511126201,
4.9622656166752));
#13322=CARTESIAN_POINT('Ctrl Pts',(-5.72993077911996,-97.81175111262,9.92453123332977));
#13323=CARTESIAN_POINT('Ctrl Pts',(1.7871392867044E-11,-97.6367511126201,
9.92453123331945));
#13324=CARTESIAN_POINT('Ctrl Pts',(5.7299307791557,-97.46175111262,9.92453123330913));
#13325=CARTESIAN_POINT('Ctrl Pts',(8.59489616871569,-97.2867511126201,4.96226561664425));
#13326=CARTESIAN_POINT('Ctrl Pts',(11.4598615582757,-97.1117511126201,-2.06354052510241E-11));
#13327=CARTESIAN_POINT('Ctrl Pts',(8.59489616869782,-96.9367511126201,-4.9622656166752));
#13328=CARTESIAN_POINT('Ctrl Pts',(5.72993077911996,-96.7617511126201,-9.92453123332976));
#13329=CARTESIAN_POINT('Ctrl Pts',(-1.78726082715848E-11,-96.5867511126201,
-9.92453123331945));
#13330=CARTESIAN_POINT('Ctrl Pts',(-5.7299307791557,-96.4117511126201,-9.92453123330913));
#13331=CARTESIAN_POINT('Ctrl Pts',(-8.59489616871569,-96.2367511126201,
-4.96226561664425));
#13332=CARTESIAN_POINT('Ctrl Pts',(-11.4598615582757,-96.0617511126201,
2.06368086793017E-11));
#13333=CARTESIAN_POINT('Ctrl Pts',(-8.59489616869782,-95.8867511126201,
4.9622656166752));
#13334=CARTESIAN_POINT('Ctrl Pts',(-5.72993077911996,-95.7117511126201,
9.92453123332977));
#13335=CARTESIAN_POINT('Ctrl Pts',(1.7871392867044E-11,-95.5367511126201,
9.92453123331945));
#13336=CARTESIAN_POINT('Ctrl Pts',(5.7299307791557,-95.3617511126201,9.92453123330913));
#13337=CARTESIAN_POINT('Ctrl Pts',(8.59489616871569,-95.1867511126201,4.96226561664425));
#13338=CARTESIAN_POINT('Ctrl Pts',(11.4598615582757,-95.0117511126201,-2.06354052510241E-11));
#13339=CARTESIAN_POINT('Ctrl Pts',(8.59489616869782,-94.83675111262,-4.9622656166752));
#13340=CARTESIAN_POINT('Ctrl Pts',(5.72993077911996,-94.6617511126201,-9.92453123332976));
#13341=CARTESIAN_POINT('Ctrl Pts',(-1.78726082715848E-11,-94.4867511126201,
-9.92453123331945));
#13342=CARTESIAN_POINT('Ctrl Pts',(-5.7299307791557,-94.3117511126201,-9.92453123330913));
#13343=CARTESIAN_POINT('Ctrl Pts',(-8.59489616871569,-94.1367511126201,
-4.96226561664425));
#13344=CARTESIAN_POINT('Ctrl Pts',(-11.4598615582757,-93.9617511126201,
2.06368086793017E-11));
#13345=CARTESIAN_POINT('Ctrl Pts',(-8.59489616869782,-93.7867511126201,
4.9622656166752));
#13346=CARTESIAN_POINT('Ctrl Pts',(-5.72993077911996,-93.6117511126201,
9.92453123332977));
#13347=CARTESIAN_POINT('Ctrl Pts',(1.7871392867044E-11,-93.4367511126201,
9.92453123331945));
#13348=CARTESIAN_POINT('Ctrl Pts',(5.7299307791557,-93.26175111262,9.92453123330913));
#13349=CARTESIAN_POINT('Ctrl Pts',(8.59489616871569,-93.0867511126201,4.96226561664425));
#13350=CARTESIAN_POINT('Ctrl Pts',(11.4598615582757,-92.9117511126201,-2.06354052510241E-11));
#13351=CARTESIAN_POINT('Ctrl Pts',(8.59489616869782,-92.7367511126201,-4.9622656166752));
#13352=CARTESIAN_POINT('Ctrl Pts',(5.72993077911996,-92.5617511126201,-9.92453123332976));
#13353=CARTESIAN_POINT('Ctrl Pts',(-1.78726082715848E-11,-92.3867511126201,
-9.92453123331945));
#13354=CARTESIAN_POINT('Ctrl Pts',(-5.7299307791557,-92.2117511126201,-9.92453123330913));
#13355=CARTESIAN_POINT('Ctrl Pts',(-8.59489616871569,-92.0367511126201,
-4.96226561664425));
#13356=CARTESIAN_POINT('Ctrl Pts',(-11.4598615582757,-91.8617511126201,
2.06368086793017E-11));
#13357=CARTESIAN_POINT('Ctrl Pts',(-8.59489616869782,-91.6867511126201,
4.9622656166752));
#13358=CARTESIAN_POINT('Ctrl Pts',(-5.72993077911996,-91.5117511126201,
9.92453123332977));
#13359=CARTESIAN_POINT('Ctrl Pts',(1.7871392867044E-11,-91.3367511126201,
9.92453123331945));
#13360=CARTESIAN_POINT('Ctrl Pts',(5.7299307791557,-91.1617511126201,9.92453123330913));
#13361=CARTESIAN_POINT('Ctrl Pts',(8.59489616871569,-90.9867511126201,4.96226561664425));
#13362=CARTESIAN_POINT('Ctrl Pts',(11.4598615582757,-90.8117511126201,-2.06354052510241E-11));
#13363=CARTESIAN_POINT('Ctrl Pts',(8.59489616869782,-90.6367511126201,-4.9622656166752));
#13364=CARTESIAN_POINT('Ctrl Pts',(5.72993077911996,-90.4617511126201,-9.92453123332976));
#13365=CARTESIAN_POINT('Ctrl Pts',(-1.78726082715848E-11,-90.2867511126201,
-9.92453123331945));
#13366=CARTESIAN_POINT('Ctrl Pts',(-5.7299307791557,-90.1117511126201,-9.92453123330913));
#13367=CARTESIAN_POINT('Ctrl Pts',(-8.59489616871569,-89.9367511126201,
-4.96226561664425));
#13368=CARTESIAN_POINT('Ctrl Pts',(-11.4598615582757,-89.7617511126201,
2.06368086793017E-11));
#13369=CARTESIAN_POINT('Ctrl Pts',(-8.59489616869782,-89.5867511126201,
4.9622656166752));
#13370=CARTESIAN_POINT('Ctrl Pts',(-5.72993077911996,-89.4117511126201,
9.92453123332977));
#13371=CARTESIAN_POINT('Ctrl Pts',(1.7871392867044E-11,-89.2367511126201,
9.92453123331945));
#13372=CARTESIAN_POINT('Ctrl Pts',(5.7299307791557,-89.0617511126201,9.92453123330913));
#13373=CARTESIAN_POINT('Ctrl Pts',(8.59489616871569,-88.8867511126201,4.96226561664425));
#13374=CARTESIAN_POINT('Ctrl Pts',(11.4598615582757,-88.7117511126201,-2.06354052510241E-11));
#13375=CARTESIAN_POINT('Ctrl Pts',(8.59489616869782,-88.5367511126201,-4.9622656166752));
#13376=CARTESIAN_POINT('Ctrl Pts',(5.72993077911996,-88.3617511126201,-9.92453123332976));
#13377=CARTESIAN_POINT('Ctrl Pts',(-1.78726082715848E-11,-88.1867511126201,
-9.92453123331945));
#13378=CARTESIAN_POINT('Ctrl Pts',(-5.7299307791557,-88.0117511126201,-9.92453123330913));
#13379=CARTESIAN_POINT('Ctrl Pts',(-8.59489616871569,-87.8367511126201,
-4.96226561664425));
#13380=CARTESIAN_POINT('Ctrl Pts',(-11.4598615582757,-87.6617511126201,
2.06368086793017E-11));
#13381=CARTESIAN_POINT('Ctrl Pts',(-8.59489616869782,-87.4867511126201,
4.9622656166752));
#13382=CARTESIAN_POINT('Ctrl Pts',(-5.72993077911996,-87.3117511126201,
9.92453123332977));
#13383=CARTESIAN_POINT('Ctrl Pts',(1.7871392867044E-11,-87.1367511126201,
9.92453123331945));
#13384=CARTESIAN_POINT('Ctrl Pts',(5.7299307791557,-86.9617511126201,9.92453123330913));
#13385=CARTESIAN_POINT('Ctrl Pts',(8.59489616871569,-86.7867511126201,4.96226561664425));
#13386=CARTESIAN_POINT('Ctrl Pts',(11.4598615582757,-86.6117511126201,-2.06354052510241E-11));
#13387=CARTESIAN_POINT('Ctrl Pts',(8.59489616869782,-86.4367511126201,-4.9622656166752));
#13388=CARTESIAN_POINT('Ctrl Pts',(5.72993077911996,-86.2617511126201,-9.92453123332976));
#13389=CARTESIAN_POINT('Ctrl Pts',(-1.78726082715848E-11,-86.0867511126201,
-9.92453123331945));
#13390=CARTESIAN_POINT('Ctrl Pts',(-5.7299307791557,-85.9117511126201,-9.92453123330913));
#13391=CARTESIAN_POINT('Ctrl Pts',(-8.59489616871569,-85.7367511126201,
-4.96226561664425));
#13392=CARTESIAN_POINT('Ctrl Pts',(-11.4598615582757,-85.5617511126201,
2.06368086793017E-11));
#13393=CARTESIAN_POINT('Ctrl Pts',(-8.59489616869782,-85.3867511126201,
4.9622656166752));
#13394=CARTESIAN_POINT('Ctrl Pts',(-5.72993077911996,-85.2117511126201,
9.92453123332977));
#13395=CARTESIAN_POINT('Ctrl Pts',(1.7871392867044E-11,-85.0367511126201,
9.92453123331945));
#13396=CARTESIAN_POINT('Ctrl Pts',(5.7299307791557,-84.8617511126201,9.92453123330913));
#13397=CARTESIAN_POINT('Ctrl Pts',(8.59489616871569,-84.6867511126201,4.96226561664425));
#13398=CARTESIAN_POINT('Ctrl Pts',(11.4598615582757,-84.5117511126201,-2.06354052510241E-11));
#13399=CARTESIAN_POINT('Ctrl Pts',(8.59489616869782,-84.3367511126201,-4.9622656166752));
#13400=CARTESIAN_POINT('Ctrl Pts',(5.72993077911996,-84.1617511126201,-9.92453123332976));
#13401=CARTESIAN_POINT('Ctrl Pts',(-1.78726082715848E-11,-83.9867511126201,
-9.92453123331945));
#13402=CARTESIAN_POINT('Ctrl Pts',(-5.7299307791557,-83.8117511126201,-9.92453123330913));
#13403=CARTESIAN_POINT('Ctrl Pts',(-8.59489616871569,-83.6367511126201,
-4.96226561664425));
#13404=CARTESIAN_POINT('Ctrl Pts',(-11.4598615582757,-83.4617511126201,
2.06368086793017E-11));
#13405=CARTESIAN_POINT('Ctrl Pts',(-8.59489616869782,-83.2867511126201,
4.9622656166752));
#13406=CARTESIAN_POINT('Ctrl Pts',(-5.72993077911996,-83.1117511126201,
9.92453123332977));
#13407=CARTESIAN_POINT('Ctrl Pts',(1.7871392867044E-11,-82.9367511126201,
9.92453123331945));
#13408=CARTESIAN_POINT('Ctrl Pts',(5.7299307791557,-82.7617511126201,9.92453123330913));
#13409=CARTESIAN_POINT('Ctrl Pts',(8.59489616871569,-82.5867511126201,4.96226561664425));
#13410=CARTESIAN_POINT('Ctrl Pts',(11.4598615582757,-82.4117511126201,-2.06354052510241E-11));
#13411=CARTESIAN_POINT('Ctrl Pts',(8.59489616869782,-82.2367511126201,-4.9622656166752));
#13412=CARTESIAN_POINT('Ctrl Pts',(5.72993077911996,-82.0617511126201,-9.92453123332976));
#13413=CARTESIAN_POINT('Ctrl Pts',(-1.78726082715848E-11,-81.8867511126201,
-9.92453123331945));
#13414=CARTESIAN_POINT('Ctrl Pts',(-5.7299307791557,-81.7117511126201,-9.92453123330913));
#13415=CARTESIAN_POINT('Ctrl Pts',(-8.59489616871569,-81.5367511126201,
-4.96226561664425));
#13416=CARTESIAN_POINT('Ctrl Pts',(-11.4598615582757,-81.3617511126201,
2.06368086793017E-11));
#13417=CARTESIAN_POINT('Ctrl Pts',(-8.59489616869782,-81.1867511126201,
4.9622656166752));
#13418=CARTESIAN_POINT('Ctrl Pts',(-5.72993077911996,-81.0117511126201,
9.92453123332977));
#13419=CARTESIAN_POINT('Ctrl Pts',(1.7871392867044E-11,-80.8367511126201,
9.92453123331945));
#13420=CARTESIAN_POINT('Ctrl Pts',(5.7299307791557,-80.6617511126201,9.92453123330913));
#13421=CARTESIAN_POINT('Ctrl Pts',(8.59489616871569,-80.4867511126201,4.96226561664425));
#13422=CARTESIAN_POINT('Ctrl Pts',(11.4598615582757,-80.3117511126201,-2.06354052510241E-11));
#13423=CARTESIAN_POINT('Ctrl Pts',(8.59489616869782,-80.1367511126201,-4.9622656166752));
#13424=CARTESIAN_POINT('Ctrl Pts',(5.72993077911996,-79.9617511126201,-9.92453123332976));
#13425=CARTESIAN_POINT('Ctrl Pts',(-1.78726082715848E-11,-79.7867511126201,
-9.92453123331945));
#13426=CARTESIAN_POINT('Ctrl Pts',(-5.7299307791557,-79.6117511126201,-9.92453123330913));
#13427=CARTESIAN_POINT('Ctrl Pts',(-8.59489616871569,-79.4367511126201,
-4.96226561664425));
#13428=CARTESIAN_POINT('Ctrl Pts',(-11.4598615582757,-79.2617511126201,
2.06368086793017E-11));
#13429=CARTESIAN_POINT('Ctrl Pts',(-8.59489616869782,-79.0867511126201,
4.9622656166752));
#13430=CARTESIAN_POINT('Ctrl Pts',(-5.72993077911996,-78.9117511126201,
9.92453123332977));
#13431=CARTESIAN_POINT('Ctrl Pts',(1.7871392867044E-11,-78.7367511126201,
9.92453123331945));
#13432=CARTESIAN_POINT('Ctrl Pts',(5.7299307791557,-78.5617511126201,9.92453123330913));
#13433=CARTESIAN_POINT('Ctrl Pts',(8.59489616871569,-78.3867511126201,4.96226561664425));
#13434=CARTESIAN_POINT('Ctrl Pts',(11.4598615582757,-78.2117511126201,-2.06354052510241E-11));
#13435=CARTESIAN_POINT('Ctrl Pts',(8.59489616869782,-78.0367511126201,-4.9622656166752));
#13436=CARTESIAN_POINT('Ctrl Pts',(5.72993077911996,-77.8617511126201,-9.92453123332976));
#13437=CARTESIAN_POINT('Ctrl Pts',(-1.78726082715848E-11,-77.6867511126201,
-9.92453123331945));
#13438=CARTESIAN_POINT('Ctrl Pts',(-5.7299307791557,-77.5117511126201,-9.92453123330913));
#13439=CARTESIAN_POINT('Ctrl Pts',(-8.59489616871569,-77.3367511126201,
-4.96226561664425));
#13440=CARTESIAN_POINT('Ctrl Pts',(-11.4598615582757,-77.1617511126201,
2.06368086793017E-11));
#13441=CARTESIAN_POINT('Ctrl Pts',(-8.59489616869782,-76.9867511126201,
4.9622656166752));
#13442=CARTESIAN_POINT('Ctrl Pts',(-5.72993077911996,-76.8117511126201,
9.92453123332977));
#13443=CARTESIAN_POINT('Ctrl Pts',(1.7871392867044E-11,-76.6367511126201,
9.92453123331945));
#13444=CARTESIAN_POINT('Ctrl Pts',(5.7299307791557,-76.4617511126201,9.92453123330913));
#13445=CARTESIAN_POINT('Ctrl Pts',(8.59489616871569,-76.2867511126201,4.96226561664425));
#13446=CARTESIAN_POINT('Ctrl Pts',(11.4598615582757,-76.1117511126201,-2.06354052510241E-11));
#13447=CARTESIAN_POINT('Ctrl Pts',(8.59489616869782,-75.9367511126201,-4.9622656166752));
#13448=CARTESIAN_POINT('Ctrl Pts',(5.72993077911996,-75.7617511126201,-9.92453123332976));
#13449=CARTESIAN_POINT('Ctrl Pts',(-1.78726082715848E-11,-75.5867511126201,
-9.92453123331945));
#13450=CARTESIAN_POINT('Ctrl Pts',(-5.7299307791557,-75.4117511126201,-9.92453123330913));
#13451=CARTESIAN_POINT('Ctrl Pts',(-8.59489616871569,-75.2367511126201,
-4.96226561664425));
#13452=CARTESIAN_POINT('Ctrl Pts',(-11.4598615582757,-75.0617511126201,
2.06368086793017E-11));
#13453=CARTESIAN_POINT('Ctrl Pts',(-8.59489616869782,-74.8867511126201,
4.9622656166752));
#13454=CARTESIAN_POINT('Ctrl Pts',(-5.72993077911996,-74.7117511126201,
9.92453123332977));
#13455=CARTESIAN_POINT('Ctrl Pts',(1.7871392867044E-11,-74.5367511126201,
9.92453123331945));
#13456=CARTESIAN_POINT('Ctrl Pts',(5.7299307791557,-74.3617511126201,9.92453123330913));
#13457=CARTESIAN_POINT('Ctrl Pts',(8.59489616871569,-74.1867511126201,4.96226561664425));
#13458=CARTESIAN_POINT('Ctrl Pts',(11.4598615582757,-74.0117511126201,-2.06354052510241E-11));
#13459=CARTESIAN_POINT('Ctrl Pts',(8.59489616869782,-73.8367511126201,-4.9622656166752));
#13460=CARTESIAN_POINT('Ctrl Pts',(5.72993077911996,-73.6617511126201,-9.92453123332976));
#13461=CARTESIAN_POINT('Ctrl Pts',(-1.78726082715848E-11,-73.4867511126201,
-9.92453123331945));
#13462=CARTESIAN_POINT('Ctrl Pts',(-5.7299307791557,-73.3117511126201,-9.92453123330913));
#13463=CARTESIAN_POINT('Ctrl Pts',(-8.59489616871569,-73.1367511126201,
-4.96226561664425));
#13464=CARTESIAN_POINT('Ctrl Pts',(-11.4598615582757,-72.9617511126201,
2.06368086793017E-11));
#13465=CARTESIAN_POINT('Ctrl Pts',(-8.59489616869782,-72.7867511126201,
4.9622656166752));
#13466=CARTESIAN_POINT('Ctrl Pts',(-5.72993077911996,-72.6117511126201,
9.92453123332977));
#13467=CARTESIAN_POINT('Ctrl Pts',(1.7871392867044E-11,-72.4367511126201,
9.92453123331945));
#13468=CARTESIAN_POINT('Ctrl Pts',(5.7299307791557,-72.2617511126201,9.92453123330913));
#13469=CARTESIAN_POINT('Ctrl Pts',(8.59489616871569,-72.0867511126201,4.96226561664425));
#13470=CARTESIAN_POINT('Ctrl Pts',(11.4598615582757,-71.9117511126201,-2.06354052510241E-11));
#13471=CARTESIAN_POINT('Ctrl Pts',(8.59489616869782,-71.7367511126201,-4.9622656166752));
#13472=CARTESIAN_POINT('Ctrl Pts',(5.72993077911996,-71.5617511126201,-9.92453123332976));
#13473=CARTESIAN_POINT('Ctrl Pts',(-1.78726082715848E-11,-71.3867511126201,
-9.92453123331945));
#13474=CARTESIAN_POINT('Ctrl Pts',(-5.7299307791557,-71.2117511126201,-9.92453123330913));
#13475=CARTESIAN_POINT('Ctrl Pts',(-8.59489616871569,-71.0367511126201,
-4.96226561664425));
#13476=CARTESIAN_POINT('Ctrl Pts',(-11.4598615582757,-70.8617511126201,
2.06368086793017E-11));
#13477=CARTESIAN_POINT('Ctrl Pts',(-8.59489616869782,-70.6867511126201,
4.9622656166752));
#13478=CARTESIAN_POINT('Ctrl Pts',(-5.72993077911996,-70.5117511126201,
9.92453123332977));
#13479=CARTESIAN_POINT('Ctrl Pts',(1.7871392867044E-11,-70.3367511126201,
9.92453123331945));
#13480=CARTESIAN_POINT('Ctrl Pts',(5.7299307791557,-70.1617511126201,9.92453123330913));
#13481=CARTESIAN_POINT('Ctrl Pts',(8.59489616871569,-69.9867511126201,4.96226561664425));
#13482=CARTESIAN_POINT('Ctrl Pts',(11.4598615582757,-69.8117511126202,-2.06354052510241E-11));
#13483=CARTESIAN_POINT('Ctrl Pts',(8.59489616869782,-69.6367511126201,-4.9622656166752));
#13484=CARTESIAN_POINT('Ctrl Pts',(5.72993077911996,-69.4617511126201,-9.92453123332976));
#13485=CARTESIAN_POINT('Ctrl Pts',(-1.78726082715848E-11,-69.2867511126201,
-9.92453123331945));
#13486=CARTESIAN_POINT('Ctrl Pts',(-5.7299307791557,-69.1117511126201,-9.92453123330913));
#13487=CARTESIAN_POINT('Ctrl Pts',(-8.59489616871569,-68.9367511126201,
-4.96226561664425));
#13488=CARTESIAN_POINT('Ctrl Pts',(-11.4598615582757,-68.7617511126201,
2.06368086793017E-11));
#13489=CARTESIAN_POINT('Ctrl Pts',(-8.59489616869782,-68.5867511126201,
4.9622656166752));
#13490=CARTESIAN_POINT('Ctrl Pts',(-5.72993077911996,-68.4117511126201,
9.92453123332977));
#13491=CARTESIAN_POINT('Ctrl Pts',(1.7871392867044E-11,-68.2367511126201,
9.92453123331945));
#13492=CARTESIAN_POINT('Ctrl Pts',(5.7299307791557,-68.0617511126201,9.92453123330913));
#13493=CARTESIAN_POINT('Ctrl Pts',(8.59489616871569,-67.8867511126201,4.96226561664425));
#13494=CARTESIAN_POINT('Ctrl Pts',(11.4598615582757,-67.7117511126201,-2.06354052510241E-11));
#13495=CARTESIAN_POINT('Ctrl Pts',(8.59489616869782,-67.5367511126201,-4.9622656166752));
#13496=CARTESIAN_POINT('Ctrl Pts',(5.72993077911996,-67.3617511126201,-9.92453123332976));
#13497=CARTESIAN_POINT('Ctrl Pts',(-1.78726082715848E-11,-67.1867511126201,
-9.92453123331945));
#13498=CARTESIAN_POINT('Ctrl Pts',(-5.7299307791557,-67.0117511126201,-9.92453123330913));
#13499=CARTESIAN_POINT('Ctrl Pts',(-8.59489616871569,-66.8367511126201,
-4.96226561664425));
#13500=CARTESIAN_POINT('Ctrl Pts',(-11.4598615582757,-66.6617511126201,
2.06368086793017E-11));
#13501=CARTESIAN_POINT('Ctrl Pts',(-8.59489616869782,-66.4867511126201,
4.9622656166752));
#13502=CARTESIAN_POINT('Ctrl Pts',(-5.72993077911996,-66.3117511126201,
9.92453123332977));
#13503=CARTESIAN_POINT('Ctrl Pts',(1.7871392867044E-11,-66.1367511126201,
9.92453123331945));
#13504=CARTESIAN_POINT('Ctrl Pts',(5.7299307791557,-65.9617511126201,9.92453123330913));
#13505=CARTESIAN_POINT('Ctrl Pts',(8.59489616871569,-65.7867511126201,4.96226561664425));
#13506=CARTESIAN_POINT('Ctrl Pts',(11.4598615582757,-65.6117511126201,-2.06354052510241E-11));
#13507=CARTESIAN_POINT('Ctrl Pts',(8.59489616869782,-65.4367511126201,-4.9622656166752));
#13508=CARTESIAN_POINT('Ctrl Pts',(5.72993077911996,-65.2617511126201,-9.92453123332976));
#13509=CARTESIAN_POINT('Ctrl Pts',(-1.78726082715848E-11,-65.0867511126201,
-9.92453123331945));
#13510=CARTESIAN_POINT('Ctrl Pts',(-5.7299307791557,-64.9117511126201,-9.92453123330913));
#13511=CARTESIAN_POINT('Ctrl Pts',(-8.59489616871569,-64.7367511126201,
-4.96226561664425));
#13512=CARTESIAN_POINT('Ctrl Pts',(-11.4598615582757,-64.5617511126202,
2.06368086793017E-11));
#13513=CARTESIAN_POINT('Ctrl Pts',(-8.59489616869782,-64.3867511126201,
4.9622656166752));
#13514=CARTESIAN_POINT('Ctrl Pts',(-5.72993077911996,-64.2117511126201,
9.92453123332977));
#13515=CARTESIAN_POINT('Ctrl Pts',(1.7871392867044E-11,-64.0367511126202,
9.92453123331945));
#13516=CARTESIAN_POINT('Ctrl Pts',(5.7299307791557,-63.8617511126201,9.92453123330913));
#13517=CARTESIAN_POINT('Ctrl Pts',(8.59489616871569,-63.6867511126202,4.96226561664425));
#13518=CARTESIAN_POINT('Ctrl Pts',(11.4598615582757,-63.5117511126202,-2.06354052510241E-11));
#13519=CARTESIAN_POINT('Ctrl Pts',(8.59489616869782,-63.3367511126201,-4.9622656166752));
#13520=CARTESIAN_POINT('Ctrl Pts',(5.72993077911996,-63.1617511126202,-9.92453123332976));
#13521=CARTESIAN_POINT('Ctrl Pts',(-1.78726082715848E-11,-62.9867511126201,
-9.92453123331945));
#13522=CARTESIAN_POINT('Ctrl Pts',(-5.7299307791557,-62.8117511126201,-9.92453123330913));
#13523=CARTESIAN_POINT('Ctrl Pts',(-8.59489616871569,-62.6367511126202,
-4.96226561664425));
#13524=CARTESIAN_POINT('Ctrl Pts',(-11.4598615582757,-62.4617511126202,
2.06368086793017E-11));
#13525=CARTESIAN_POINT('Ctrl Pts',(-8.59489616869782,-62.2867511126201,
4.9622656166752));
#13526=CARTESIAN_POINT('Ctrl Pts',(-5.72993077911996,-62.1117511126202,
9.92453123332977));
#13527=CARTESIAN_POINT('Ctrl Pts',(1.7871392867044E-11,-61.9367511126202,
9.92453123331945));
#13528=CARTESIAN_POINT('Ctrl Pts',(5.7299307791557,-61.7617511126201,9.92453123330913));
#13529=CARTESIAN_POINT('Ctrl Pts',(8.59489616871569,-61.5867511126202,4.96226561664425));
#13530=CARTESIAN_POINT('Ctrl Pts',(11.4598615582757,-61.4117511126202,-2.06354052510241E-11));
#13531=CARTESIAN_POINT('Ctrl Pts',(8.59489616869782,-61.2367511126201,-4.9622656166752));
#13532=CARTESIAN_POINT('Ctrl Pts',(5.72993077911996,-61.0617511126202,-9.92453123332976));
#13533=CARTESIAN_POINT('Ctrl Pts',(-1.78726082715848E-11,-60.8867511126202,
-9.92453123331945));
#13534=CARTESIAN_POINT('Ctrl Pts',(-5.7299307791557,-60.7117511126201,-9.92453123330913));
#13535=CARTESIAN_POINT('Ctrl Pts',(-8.59489616871569,-60.5367511126202,
-4.96226561664425));
#13536=CARTESIAN_POINT('Ctrl Pts',(-11.4598615582757,-60.3617511126201,
2.06368086793017E-11));
#13537=CARTESIAN_POINT('Ctrl Pts',(-8.59489616869782,-60.1867511126201,
4.9622656166752));
#13538=CARTESIAN_POINT('Ctrl Pts',(-5.72993077911996,-60.0117511126202,
9.92453123332977));
#13539=CARTESIAN_POINT('Ctrl Pts',(1.7871392867044E-11,-59.8367511126201,
9.92453123331945));
#13540=CARTESIAN_POINT('Ctrl Pts',(5.7299307791557,-59.6617511126202,9.92453123330913));
#13541=CARTESIAN_POINT('Ctrl Pts',(8.59489616871569,-59.4867511126202,4.96226561664425));
#13542=CARTESIAN_POINT('Ctrl Pts',(11.4598615582757,-59.3117511126202,-2.06354052510241E-11));
#13543=CARTESIAN_POINT('Ctrl Pts',(8.59489616869782,-59.1367511126202,-4.9622656166752));
#13544=CARTESIAN_POINT('Ctrl Pts',(5.72993077911996,-58.9617511126202,-9.92453123332976));
#13545=CARTESIAN_POINT('Ctrl Pts',(-1.78726082715848E-11,-58.7867511126201,
-9.92453123331945));
#13546=CARTESIAN_POINT('Ctrl Pts',(-5.7299307791557,-58.6117511126201,-9.92453123330913));
#13547=CARTESIAN_POINT('Ctrl Pts',(-8.59489616871569,-58.4367511126202,
-4.96226561664425));
#13548=CARTESIAN_POINT('Ctrl Pts',(-11.4598615582757,-58.2617511126201,
2.06368086793017E-11));
#13549=CARTESIAN_POINT('Ctrl Pts',(-8.59489616869782,-58.0867511126202,
4.9622656166752));
#13550=CARTESIAN_POINT('Ctrl Pts',(-5.72993077911996,-57.9117511126202,
9.92453123332977));
#13551=CARTESIAN_POINT('Ctrl Pts',(1.7871392867044E-11,-57.7367511126201,
9.92453123331945));
#13552=CARTESIAN_POINT('Ctrl Pts',(5.7299307791557,-57.5617511126202,9.92453123330913));
#13553=CARTESIAN_POINT('Ctrl Pts',(8.59489616871569,-57.3867511126202,4.96226561664425));
#13554=CARTESIAN_POINT('Ctrl Pts',(11.4598615582757,-57.2117511126201,-2.06354052510241E-11));
#13555=CARTESIAN_POINT('Ctrl Pts',(8.59489616869782,-57.0367511126202,-4.9622656166752));
#13556=CARTESIAN_POINT('Ctrl Pts',(5.72993077911996,-56.8617511126202,-9.92453123332976));
#13557=CARTESIAN_POINT('Ctrl Pts',(-1.78726082715848E-11,-56.6867511126202,
-9.92453123331945));
#13558=CARTESIAN_POINT('Ctrl Pts',(-5.7299307791557,-56.5117511126202,-9.92453123330913));
#13559=CARTESIAN_POINT('Ctrl Pts',(-8.59489616871569,-56.3367511126202,
-4.96226561664425));
#13560=CARTESIAN_POINT('Ctrl Pts',(-11.4598615582757,-56.1617511126202,
2.06368086793017E-11));
#13561=CARTESIAN_POINT('Ctrl Pts',(-8.59489616869782,-55.9867511126202,
4.9622656166752));
#13562=CARTESIAN_POINT('Ctrl Pts',(-5.72993077911996,-55.8117511126202,
9.92453123332977));
#13563=CARTESIAN_POINT('Ctrl Pts',(1.7871392867044E-11,-55.6367511126201,
9.92453123331945));
#13564=CARTESIAN_POINT('Ctrl Pts',(5.7299307791557,-55.4617511126202,9.92453123330913));
#13565=CARTESIAN_POINT('Ctrl Pts',(8.59489616871569,-55.2867511126202,4.96226561664425));
#13566=CARTESIAN_POINT('Ctrl Pts',(11.4598615582757,-55.1117511126202,-2.06354052510241E-11));
#13567=CARTESIAN_POINT('Ctrl Pts',(8.59489616869782,-54.9367511126202,-4.9622656166752));
#13568=CARTESIAN_POINT('Ctrl Pts',(5.72993077911996,-54.7617511126202,-9.92453123332976));
#13569=CARTESIAN_POINT('Ctrl Pts',(-1.78726082715848E-11,-54.5867511126202,
-9.92453123331945));
#13570=CARTESIAN_POINT('Ctrl Pts',(-5.7299307791557,-54.4117511126202,-9.92453123330913));
#13571=CARTESIAN_POINT('Ctrl Pts',(-8.59489616871569,-54.2367511126202,
-4.96226561664425));
#13572=CARTESIAN_POINT('Ctrl Pts',(-11.4598615582757,-54.0617511126202,
2.06368086793017E-11));
#13573=CARTESIAN_POINT('Ctrl Pts',(-8.59489616869782,-53.8867511126202,
4.9622656166752));
#13574=CARTESIAN_POINT('Ctrl Pts',(-5.72993077911996,-53.7117511126202,
9.92453123332977));
#13575=CARTESIAN_POINT('Ctrl Pts',(1.7871392867044E-11,-53.5367511126202,
9.92453123331945));
#13576=CARTESIAN_POINT('Ctrl Pts',(5.7299307791557,-53.3617511126202,9.92453123330913));
#13577=CARTESIAN_POINT('Ctrl Pts',(8.59489616871569,-53.1867511126202,4.96226561664425));
#13578=CARTESIAN_POINT('Ctrl Pts',(11.4598615582757,-53.0117511126202,-2.06354052510241E-11));
#13579=CARTESIAN_POINT('Ctrl Pts',(8.59489616869782,-52.8367511126202,-4.9622656166752));
#13580=CARTESIAN_POINT('Ctrl Pts',(5.72993077911996,-52.6617511126202,-9.92453123332976));
#13581=CARTESIAN_POINT('Ctrl Pts',(-1.78726082715848E-11,-52.4867511126202,
-9.92453123331945));
#13582=CARTESIAN_POINT('Ctrl Pts',(-5.7299307791557,-52.3117511126202,-9.92453123330913));
#13583=CARTESIAN_POINT('Ctrl Pts',(-8.59489616871569,-52.1367511126202,
-4.96226561664425));
#13584=CARTESIAN_POINT('Ctrl Pts',(-11.4598615582757,-51.9617511126202,
2.06368086793017E-11));
#13585=CARTESIAN_POINT('Ctrl Pts',(-8.59489616869782,-51.7867511126202,
4.9622656166752));
#13586=CARTESIAN_POINT('Ctrl Pts',(-5.72993077911996,-51.6117511126202,
9.92453123332977));
#13587=CARTESIAN_POINT('Ctrl Pts',(1.7871392867044E-11,-51.4367511126202,
9.92453123331945));
#13588=CARTESIAN_POINT('Ctrl Pts',(5.7299307791557,-51.2617511126202,9.92453123330913));
#13589=CARTESIAN_POINT('Ctrl Pts',(8.59489616871569,-51.0867511126202,4.96226561664425));
#13590=CARTESIAN_POINT('Ctrl Pts',(11.4598615582757,-50.9117511126202,-2.06354052510241E-11));
#13591=CARTESIAN_POINT('Ctrl Pts',(8.59489616869782,-50.7367511126202,-4.9622656166752));
#13592=CARTESIAN_POINT('Ctrl Pts',(5.72993077911996,-50.5617511126202,-9.92453123332976));
#13593=CARTESIAN_POINT('Ctrl Pts',(-1.78726082715848E-11,-50.3867511126202,
-9.92453123331945));
#13594=CARTESIAN_POINT('Ctrl Pts',(-5.7299307791557,-50.2117511126202,-9.92453123330913));
#13595=CARTESIAN_POINT('Ctrl Pts',(-8.59489616871569,-50.0367511126202,
-4.96226561664425));
#13596=CARTESIAN_POINT('Ctrl Pts',(-11.4598615582757,-49.8617511126202,
2.06368086793017E-11));
#13597=CARTESIAN_POINT('Ctrl Pts',(-8.59489616869782,-49.6867511126202,
4.9622656166752));
#13598=CARTESIAN_POINT('Ctrl Pts',(-5.72993077911996,-49.5117511126202,
9.92453123332977));
#13599=CARTESIAN_POINT('Ctrl Pts',(1.7871392867044E-11,-49.3367511126202,
9.92453123331945));
#13600=CARTESIAN_POINT('Ctrl Pts',(5.7299307791557,-49.1617511126202,9.92453123330913));
#13601=CARTESIAN_POINT('Ctrl Pts',(8.59489616871569,-48.9867511126202,4.96226561664425));
#13602=CARTESIAN_POINT('Ctrl Pts',(11.4598615582757,-48.8117511126202,-2.06354052510241E-11));
#13603=CARTESIAN_POINT('Ctrl Pts',(8.59489616869782,-48.6367511126202,-4.9622656166752));
#13604=CARTESIAN_POINT('Ctrl Pts',(5.72993077911996,-48.4617511126202,-9.92453123332976));
#13605=CARTESIAN_POINT('Ctrl Pts',(-1.78726082715848E-11,-48.2867511126202,
-9.92453123331945));
#13606=CARTESIAN_POINT('Ctrl Pts',(-5.7299307791557,-48.1117511126202,-9.92453123330913));
#13607=CARTESIAN_POINT('Ctrl Pts',(-8.59489616871569,-47.9367511126202,
-4.96226561664425));
#13608=CARTESIAN_POINT('Ctrl Pts',(-11.4598615582757,-47.7617511126202,
2.06368086793017E-11));
#13609=CARTESIAN_POINT('Ctrl Pts',(-8.59489616869782,-47.5867511126202,
4.9622656166752));
#13610=CARTESIAN_POINT('Ctrl Pts',(-5.72993077911996,-47.4117511126202,
9.92453123332977));
#13611=CARTESIAN_POINT('Ctrl Pts',(1.7871392867044E-11,-47.2367511126202,
9.92453123331945));
#13612=CARTESIAN_POINT('Ctrl Pts',(5.7299307791557,-47.0617511126202,9.92453123330913));
#13613=CARTESIAN_POINT('Ctrl Pts',(8.59489616871569,-46.8867511126202,4.96226561664425));
#13614=CARTESIAN_POINT('Ctrl Pts',(11.4598615582757,-46.7117511126202,-2.06354052510241E-11));
#13615=CARTESIAN_POINT('Ctrl Pts',(8.59489616869782,-46.5367511126202,-4.9622656166752));
#13616=CARTESIAN_POINT('Ctrl Pts',(5.72993077911996,-46.3617511126202,-9.92453123332976));
#13617=CARTESIAN_POINT('Ctrl Pts',(-1.78726082715848E-11,-46.1867511126202,
-9.92453123331945));
#13618=CARTESIAN_POINT('Ctrl Pts',(-5.7299307791557,-46.0117511126202,-9.92453123330913));
#13619=CARTESIAN_POINT('Ctrl Pts',(-8.59489616871569,-45.8367511126202,
-4.96226561664425));
#13620=CARTESIAN_POINT('Ctrl Pts',(-11.4598615582757,-45.6617511126202,
2.06368086793017E-11));
#13621=CARTESIAN_POINT('Ctrl Pts',(-8.59489616869782,-45.4867511126202,
4.9622656166752));
#13622=CARTESIAN_POINT('Ctrl Pts',(-5.72993077911996,-45.3117511126202,
9.92453123332977));
#13623=CARTESIAN_POINT('Ctrl Pts',(1.7871392867044E-11,-45.1367511126202,
9.92453123331945));
#13624=CARTESIAN_POINT('Ctrl Pts',(5.7299307791557,-44.9617511126202,9.92453123330913));
#13625=CARTESIAN_POINT('Ctrl Pts',(8.59489616871569,-44.7867511126202,4.96226561664425));
#13626=CARTESIAN_POINT('Ctrl Pts',(11.4598615582757,-44.6117511126202,-2.06354052510241E-11));
#13627=CARTESIAN_POINT('Ctrl Pts',(8.59489616869782,-44.4367511126202,-4.9622656166752));
#13628=CARTESIAN_POINT('Ctrl Pts',(5.72993077911996,-44.2617511126202,-9.92453123332976));
#13629=CARTESIAN_POINT('Ctrl Pts',(-1.78726082715848E-11,-44.0867511126202,
-9.92453123331945));
#13630=CARTESIAN_POINT('Ctrl Pts',(-5.7299307791557,-43.9117511126202,-9.92453123330913));
#13631=CARTESIAN_POINT('Ctrl Pts',(-8.59489616871569,-43.7367511126202,
-4.96226561664425));
#13632=CARTESIAN_POINT('Ctrl Pts',(-11.4598615582757,-43.5617511126202,
2.06368086793017E-11));
#13633=CARTESIAN_POINT('Ctrl Pts',(-8.59489616869782,-43.3867511126202,
4.9622656166752));
#13634=CARTESIAN_POINT('Ctrl Pts',(-5.72993077911996,-43.2117511126202,
9.92453123332977));
#13635=CARTESIAN_POINT('Ctrl Pts',(1.7871392867044E-11,-43.0367511126202,
9.92453123331945));
#13636=CARTESIAN_POINT('Ctrl Pts',(5.7299307791557,-42.8617511126202,9.92453123330913));
#13637=CARTESIAN_POINT('Ctrl Pts',(8.59489616871569,-42.6867511126202,4.96226561664425));
#13638=CARTESIAN_POINT('Ctrl Pts',(11.4598615582757,-42.5117511126202,-2.06354052510241E-11));
#13639=CARTESIAN_POINT('Ctrl Pts',(8.59489616869782,-42.3367511126202,-4.9622656166752));
#13640=CARTESIAN_POINT('Ctrl Pts',(5.72993077911996,-42.1617511126202,-9.92453123332976));
#13641=CARTESIAN_POINT('Ctrl Pts',(-1.78726082715848E-11,-41.9867511126202,
-9.92453123331945));
#13642=CARTESIAN_POINT('Ctrl Pts',(-5.7299307791557,-41.8117511126202,-9.92453123330913));
#13643=CARTESIAN_POINT('Ctrl Pts',(-8.59489616871569,-41.6367511126202,
-4.96226561664425));
#13644=CARTESIAN_POINT('Ctrl Pts',(-11.4598615582757,-41.4617511126202,
2.06368086793017E-11));
#13645=CARTESIAN_POINT('Ctrl Pts',(-8.59489616869782,-41.2867511126202,
4.9622656166752));
#13646=CARTESIAN_POINT('Ctrl Pts',(-5.72993077911996,-41.1117511126202,
9.92453123332977));
#13647=CARTESIAN_POINT('Ctrl Pts',(1.7871392867044E-11,-40.9367511126202,
9.92453123331945));
#13648=CARTESIAN_POINT('Ctrl Pts',(5.7299307791557,-40.7617511126202,9.92453123330913));
#13649=CARTESIAN_POINT('Ctrl Pts',(8.59489616871569,-40.5867511126202,4.96226561664425));
#13650=CARTESIAN_POINT('Ctrl Pts',(11.4598615582757,-40.4117511126202,-2.06354052510241E-11));
#13651=CARTESIAN_POINT('Ctrl Pts',(8.59489616869782,-40.2367511126202,-4.9622656166752));
#13652=CARTESIAN_POINT('Ctrl Pts',(5.72993077911996,-40.0617511126202,-9.92453123332976));
#13653=CARTESIAN_POINT('Ctrl Pts',(-1.78726082715848E-11,-39.8867511126202,
-9.92453123331945));
#13654=CARTESIAN_POINT('Ctrl Pts',(-5.7299307791557,-39.7117511126202,-9.92453123330913));
#13655=CARTESIAN_POINT('Ctrl Pts',(-8.59489616871569,-39.5367511126202,
-4.96226561664425));
#13656=CARTESIAN_POINT('Ctrl Pts',(-11.4598615582757,-39.3617511126202,
2.06368086793017E-11));
#13657=CARTESIAN_POINT('Ctrl Pts',(-8.59489616869782,-39.1867511126202,
4.9622656166752));
#13658=CARTESIAN_POINT('Ctrl Pts',(-5.72993077911996,-39.0117511126202,
9.92453123332977));
#13659=CARTESIAN_POINT('Ctrl Pts',(1.7871392867044E-11,-38.8367511126202,
9.92453123331945));
#13660=CARTESIAN_POINT('Ctrl Pts',(5.7299307791557,-38.6617511126202,9.92453123330913));
#13661=CARTESIAN_POINT('Ctrl Pts',(8.59489616871569,-38.4867511126202,4.96226561664425));
#13662=CARTESIAN_POINT('Ctrl Pts',(11.4598615582757,-38.3117511126202,-2.06354052510241E-11));
#13663=CARTESIAN_POINT('Ctrl Pts',(8.59489616869782,-38.1367511126202,-4.9622656166752));
#13664=CARTESIAN_POINT('Ctrl Pts',(5.72993077911996,-37.9617511126202,-9.92453123332976));
#13665=CARTESIAN_POINT('Ctrl Pts',(-1.78726082715848E-11,-37.7867511126202,
-9.92453123331945));
#13666=CARTESIAN_POINT('Ctrl Pts',(-5.7299307791557,-37.6117511126202,-9.92453123330913));
#13667=CARTESIAN_POINT('Ctrl Pts',(-8.59489616871569,-37.4367511126202,
-4.96226561664425));
#13668=CARTESIAN_POINT('Ctrl Pts',(-11.4598615582757,-37.2617511126202,
2.06368086793017E-11));
#13669=CARTESIAN_POINT('Ctrl Pts',(-8.59489616869782,-37.0867511126202,
4.9622656166752));
#13670=CARTESIAN_POINT('Ctrl Pts',(-5.72993077911996,-36.9117511126202,
9.92453123332977));
#13671=CARTESIAN_POINT('Ctrl Pts',(1.7871392867044E-11,-36.7367511126202,
9.92453123331945));
#13672=CARTESIAN_POINT('Ctrl Pts',(5.7299307791557,-36.5617511126202,9.92453123330913));
#13673=CARTESIAN_POINT('Ctrl Pts',(8.59489616871569,-36.3867511126202,4.96226561664425));
#13674=CARTESIAN_POINT('Ctrl Pts',(11.4598615582757,-36.2117511126202,-2.06354052510241E-11));
#13675=CARTESIAN_POINT('Ctrl Pts',(8.59489616869782,-36.0367511126202,-4.9622656166752));
#13676=CARTESIAN_POINT('Ctrl Pts',(5.72993077911996,-35.8617511126202,-9.92453123332976));
#13677=CARTESIAN_POINT('Ctrl Pts',(-1.78726082715848E-11,-35.6867511126202,
-9.92453123331945));
#13678=CARTESIAN_POINT('Ctrl Pts',(-5.7299307791557,-35.5117511126202,-9.92453123330913));
#13679=CARTESIAN_POINT('Ctrl Pts',(-8.59489616871569,-35.3367511126202,
-4.96226561664425));
#13680=CARTESIAN_POINT('Ctrl Pts',(-11.4598615582757,-35.1617511126202,
2.06368086793017E-11));
#13681=CARTESIAN_POINT('Ctrl Pts',(-8.59489616869782,-34.9867511126202,
4.9622656166752));
#13682=CARTESIAN_POINT('Ctrl Pts',(-5.72993077911996,-34.8117511126202,
9.92453123332977));
#13683=CARTESIAN_POINT('Ctrl Pts',(1.7871392867044E-11,-34.6367511126202,
9.92453123331945));
#13684=CARTESIAN_POINT('Ctrl Pts',(5.7299307791557,-34.4617511126202,9.92453123330913));
#13685=CARTESIAN_POINT('Ctrl Pts',(8.59489616871569,-34.2867511126202,4.96226561664425));
#13686=CARTESIAN_POINT('Ctrl Pts',(11.4598615582757,-34.1117511126202,-2.06354052510241E-11));
#13687=CARTESIAN_POINT('Ctrl Pts',(8.59489616869782,-33.9367511126202,-4.9622656166752));
#13688=CARTESIAN_POINT('Ctrl Pts',(5.72993077911996,-33.7617511126202,-9.92453123332976));
#13689=CARTESIAN_POINT('Ctrl Pts',(-1.78726082715848E-11,-33.5867511126202,
-9.92453123331945));
#13690=CARTESIAN_POINT('Ctrl Pts',(-5.7299307791557,-33.4117511126202,-9.92453123330913));
#13691=CARTESIAN_POINT('Ctrl Pts',(-8.59489616871569,-33.2367511126202,
-4.96226561664425));
#13692=CARTESIAN_POINT('Ctrl Pts',(-11.4598615582757,-33.0617511126202,
2.06368086793017E-11));
#13693=CARTESIAN_POINT('Ctrl Pts',(-8.59489616869782,-32.8867511126202,
4.9622656166752));
#13694=CARTESIAN_POINT('Ctrl Pts',(-5.72993077911996,-32.7117511126202,
9.92453123332977));
#13695=CARTESIAN_POINT('Ctrl Pts',(1.7871392867044E-11,-32.5367511126202,
9.92453123331945));
#13696=CARTESIAN_POINT('Ctrl Pts',(5.7299307791557,-32.3617511126202,9.92453123330913));
#13697=CARTESIAN_POINT('Ctrl Pts',(8.59489616871569,-32.1867511126202,4.96226561664425));
#13698=CARTESIAN_POINT('Ctrl Pts',(11.4598615582757,-32.0117511126202,-2.06354052510241E-11));
#13699=CARTESIAN_POINT('Ctrl Pts',(8.59489616869782,-31.8367511126202,-4.9622656166752));
#13700=CARTESIAN_POINT('Ctrl Pts',(5.72993077911996,-31.6617511126202,-9.92453123332976));
#13701=CARTESIAN_POINT('Ctrl Pts',(-1.78726082715848E-11,-31.4867511126202,
-9.92453123331945));
#13702=CARTESIAN_POINT('Ctrl Pts',(-5.7299307791557,-31.3117511126202,-9.92453123330913));
#13703=CARTESIAN_POINT('Ctrl Pts',(-8.59489616871569,-31.1367511126202,
-4.96226561664425));
#13704=CARTESIAN_POINT('Ctrl Pts',(-11.4598615582757,-30.9617511126202,
2.06368086793017E-11));
#13705=CARTESIAN_POINT('Ctrl Pts',(-8.59489616869782,-30.7867511126202,
4.9622656166752));
#13706=CARTESIAN_POINT('Ctrl Pts',(-5.72993077911996,-30.6117511126202,
9.92453123332977));
#13707=CARTESIAN_POINT('Ctrl Pts',(1.7871392867044E-11,-30.4367511126202,
9.92453123331945));
#13708=CARTESIAN_POINT('Ctrl Pts',(5.7299307791557,-30.2617511126202,9.92453123330913));
#13709=CARTESIAN_POINT('Ctrl Pts',(8.59489616871569,-30.0867511126202,4.96226561664425));
#13710=CARTESIAN_POINT('Ctrl Pts',(11.4598615582757,-29.9117511126202,-2.06354052510241E-11));
#13711=CARTESIAN_POINT('Ctrl Pts',(8.59489616869782,-29.7367511126202,-4.9622656166752));
#13712=CARTESIAN_POINT('Ctrl Pts',(5.72993077911996,-29.5617511126202,-9.92453123332976));
#13713=CARTESIAN_POINT('Ctrl Pts',(-1.78726082715848E-11,-29.3867511126202,
-9.92453123331945));
#13714=CARTESIAN_POINT('Ctrl Pts',(-5.7299307791557,-29.2117511126202,-9.92453123330913));
#13715=CARTESIAN_POINT('Ctrl Pts',(-8.59489616871569,-29.0367511126202,
-4.96226561664425));
#13716=CARTESIAN_POINT('Ctrl Pts',(-11.4598615582757,-28.8617511126202,
2.06368086793017E-11));
#13717=CARTESIAN_POINT('Ctrl Pts',(-8.59489616869782,-28.6867511126202,
4.9622656166752));
#13718=CARTESIAN_POINT('Ctrl Pts',(-5.72993077911996,-28.5117511126202,
9.92453123332977));
#13719=CARTESIAN_POINT('Ctrl Pts',(1.7871392867044E-11,-28.3367511126202,
9.92453123331945));
#13720=CARTESIAN_POINT('Ctrl Pts',(5.7299307791557,-28.1617511126202,9.92453123330913));
#13721=CARTESIAN_POINT('Ctrl Pts',(8.59489616871569,-27.9867511126202,4.96226561664425));
#13722=CARTESIAN_POINT('Ctrl Pts',(11.4598615582757,-27.8117511126202,-2.06354052510241E-11));
#13723=CARTESIAN_POINT('Ctrl Pts',(8.59489616869782,-27.6367511126202,-4.9622656166752));
#13724=CARTESIAN_POINT('Ctrl Pts',(5.72993077911996,-27.4617511126202,-9.92453123332976));
#13725=CARTESIAN_POINT('Ctrl Pts',(-1.78726082715848E-11,-27.2867511126202,
-9.92453123331945));
#13726=CARTESIAN_POINT('Ctrl Pts',(-5.7299307791557,-27.1117511126202,-9.92453123330913));
#13727=CARTESIAN_POINT('Ctrl Pts',(-8.59489616871569,-26.9367511126202,
-4.96226561664425));
#13728=CARTESIAN_POINT('Ctrl Pts',(-11.4598615582757,-26.7617511126202,
2.06368086793017E-11));
#13729=CARTESIAN_POINT('Ctrl Pts',(-8.59489616869782,-26.5867511126202,
4.9622656166752));
#13730=CARTESIAN_POINT('Ctrl Pts',(-5.72993077911996,-26.4117511126202,
9.92453123332977));
#13731=CARTESIAN_POINT('Ctrl Pts',(1.7871392867044E-11,-26.2367511126202,
9.92453123331945));
#13732=CARTESIAN_POINT('Ctrl Pts',(5.7299307791557,-26.0617511126202,9.92453123330913));
#13733=CARTESIAN_POINT('Ctrl Pts',(8.59489616871569,-25.8867511126202,4.96226561664425));
#13734=CARTESIAN_POINT('Ctrl Pts',(11.4598615582757,-25.7117511126202,-2.06354052510241E-11));
#13735=CARTESIAN_POINT('Ctrl Pts',(8.59489616869782,-25.5367511126202,-4.9622656166752));
#13736=CARTESIAN_POINT('Ctrl Pts',(5.72993077911996,-25.3617511126202,-9.92453123332976));
#13737=CARTESIAN_POINT('Ctrl Pts',(-1.78726082715848E-11,-25.1867511126202,
-9.92453123331945));
#13738=CARTESIAN_POINT('Ctrl Pts',(-5.7299307791557,-25.0117511126202,-9.92453123330913));
#13739=CARTESIAN_POINT('Ctrl Pts',(-8.59489616871569,-24.8367511126202,
-4.96226561664425));
#13740=CARTESIAN_POINT('Ctrl Pts',(-11.4598615582757,-24.6617511126202,
2.06368086793017E-11));
#13741=CARTESIAN_POINT('Ctrl Pts',(-8.59489616869782,-24.4867511126202,
4.9622656166752));
#13742=CARTESIAN_POINT('Ctrl Pts',(-5.72993077911996,-24.3117511126202,
9.92453123332977));
#13743=CARTESIAN_POINT('Ctrl Pts',(1.7871392867044E-11,-24.1367511126202,
9.92453123331945));
#13744=CARTESIAN_POINT('Ctrl Pts',(5.7299307791557,-23.9617511126202,9.92453123330913));
#13745=CARTESIAN_POINT('Ctrl Pts',(8.59489616871569,-23.7867511126202,4.96226561664425));
#13746=CARTESIAN_POINT('Ctrl Pts',(11.4598615582757,-23.6117511126202,-2.06354052510241E-11));
#13747=CARTESIAN_POINT('Ctrl Pts',(8.59489616869782,-23.4367511126202,-4.9622656166752));
#13748=CARTESIAN_POINT('Ctrl Pts',(5.72993077911996,-23.2617511126202,-9.92453123332976));
#13749=CARTESIAN_POINT('Ctrl Pts',(-1.78726082715848E-11,-23.0867511126202,
-9.92453123331945));
#13750=CARTESIAN_POINT('Ctrl Pts',(-5.7299307791557,-22.9117511126202,-9.92453123330913));
#13751=CARTESIAN_POINT('Ctrl Pts',(-8.59489616871569,-22.7367511126202,
-4.96226561664425));
#13752=CARTESIAN_POINT('Ctrl Pts',(-11.4598615582757,-22.5617511126203,
2.06368086793017E-11));
#13753=CARTESIAN_POINT('Ctrl Pts',(-8.59489616869782,-22.3867511126202,
4.9622656166752));
#13754=CARTESIAN_POINT('Ctrl Pts',(-5.72993077911996,-22.2117511126202,
9.92453123332977));
#13755=CARTESIAN_POINT('Ctrl Pts',(1.7871392867044E-11,-22.0367511126202,
9.92453123331945));
#13756=CARTESIAN_POINT('Ctrl Pts',(5.7299307791557,-21.8617511126202,9.92453123330913));
#13757=CARTESIAN_POINT('Ctrl Pts',(8.59489616871569,-21.6867511126202,4.96226561664425));
#13758=CARTESIAN_POINT('Ctrl Pts',(11.4598615582757,-21.5117511126203,-2.06354052510241E-11));
#13759=CARTESIAN_POINT('Ctrl Pts',(8.59489616869782,-21.3367511126202,-4.9622656166752));
#13760=CARTESIAN_POINT('Ctrl Pts',(5.72993077911996,-21.1617511126202,-9.92453123332976));
#13761=CARTESIAN_POINT('Ctrl Pts',(-1.78726082715848E-11,-20.9867511126202,
-9.92453123331945));
#13762=CARTESIAN_POINT('Ctrl Pts',(-5.7299307791557,-20.8117511126202,-9.92453123330913));
#13763=CARTESIAN_POINT('Ctrl Pts',(-8.59489616871569,-20.6367511126202,
-4.96226561664425));
#13764=CARTESIAN_POINT('Ctrl Pts',(-11.4598615582757,-20.4617511126202,
2.06368086793017E-11));
#13765=CARTESIAN_POINT('Ctrl Pts',(-8.59489616869782,-20.2867511126202,
4.9622656166752));
#13766=CARTESIAN_POINT('Ctrl Pts',(-5.72993077911996,-20.1117511126202,
9.92453123332977));
#13767=CARTESIAN_POINT('Ctrl Pts',(1.7871392867044E-11,-19.9367511126202,
9.92453123331945));
#13768=CARTESIAN_POINT('Ctrl Pts',(5.7299307791557,-19.7617511126202,9.92453123330913));
#13769=CARTESIAN_POINT('Ctrl Pts',(8.59489616871569,-19.5867511126202,4.96226561664425));
#13770=CARTESIAN_POINT('Ctrl Pts',(11.4598615582757,-19.4117511126203,-2.06354052510241E-11));
#13771=CARTESIAN_POINT('Ctrl Pts',(8.59489616869782,-19.2367511126202,-4.9622656166752));
#13772=CARTESIAN_POINT('Ctrl Pts',(5.72993077911996,-19.0617511126202,-9.92453123332976));
#13773=CARTESIAN_POINT('Ctrl Pts',(-1.78726082715848E-11,-18.8867511126203,
-9.92453123331945));
#13774=CARTESIAN_POINT('Ctrl Pts',(-5.7299307791557,-18.7117511126203,-9.92453123330913));
#13775=CARTESIAN_POINT('Ctrl Pts',(-8.59489616871569,-18.5367511126202,
-4.96226561664425));
#13776=CARTESIAN_POINT('Ctrl Pts',(-11.4598615582757,-18.3617511126203,
2.06368086793017E-11));
#13777=CARTESIAN_POINT('Ctrl Pts',(-8.59489616869782,-18.1867511126202,
4.9622656166752));
#13778=CARTESIAN_POINT('Ctrl Pts',(-5.72993077911996,-18.0117511126202,
9.92453123332977));
#13779=CARTESIAN_POINT('Ctrl Pts',(1.7871392867044E-11,-17.8367511126203,
9.92453123331945));
#13780=CARTESIAN_POINT('Ctrl Pts',(5.7299307791557,-17.6617511126203,9.92453123330913));
#13781=CARTESIAN_POINT('Ctrl Pts',(8.59489616871569,-17.4867511126202,4.96226561664425));
#13782=CARTESIAN_POINT('Ctrl Pts',(11.4598615582757,-17.3117511126203,-2.06354052510241E-11));
#13783=CARTESIAN_POINT('Ctrl Pts',(8.59489616869782,-17.1367511126203,-4.9622656166752));
#13784=CARTESIAN_POINT('Ctrl Pts',(5.72993077911996,-16.9617511126202,-9.92453123332976));
#13785=CARTESIAN_POINT('Ctrl Pts',(-1.78726082715848E-11,-16.7867511126202,
-9.92453123331945));
#13786=CARTESIAN_POINT('Ctrl Pts',(-5.7299307791557,-16.6117511126203,-9.92453123330913));
#13787=CARTESIAN_POINT('Ctrl Pts',(-8.59489616871569,-16.4367511126202,
-4.96226561664425));
#13788=CARTESIAN_POINT('Ctrl Pts',(-11.4598615582757,-16.2617511126202,
2.06368086793017E-11));
#13789=CARTESIAN_POINT('Ctrl Pts',(-8.59489616869782,-16.0867511126203,
4.9622656166752));
#13790=CARTESIAN_POINT('Ctrl Pts',(-5.72993077911996,-15.9117511126202,
9.92453123332977));
#13791=CARTESIAN_POINT('Ctrl Pts',(1.7871392867044E-11,-15.7367511126202,
9.92453123331945));
#13792=CARTESIAN_POINT('Ctrl Pts',(5.7299307791557,-15.5617511126203,9.92453123330913));
#13793=CARTESIAN_POINT('Ctrl Pts',(8.59489616871569,-15.3867511126203,4.96226561664425));
#13794=CARTESIAN_POINT('Ctrl Pts',(11.4598615582757,-15.2117511126203,-2.06354052510241E-11));
#13795=CARTESIAN_POINT('Ctrl Pts',(8.59489616869782,-15.0367511126203,-4.9622656166752));
#13796=CARTESIAN_POINT('Ctrl Pts',(5.72993077911996,-14.8617511126203,-9.92453123332976));
#13797=CARTESIAN_POINT('Ctrl Pts',(-1.78726082715848E-11,-14.6867511126202,
-9.92453123331945));
#13798=CARTESIAN_POINT('Ctrl Pts',(-5.7299307791557,-14.5117511126203,-9.92453123330913));
#13799=CARTESIAN_POINT('Ctrl Pts',(-8.59489616871569,-14.3367511126203,
-4.96226561664425));
#13800=CARTESIAN_POINT('Ctrl Pts',(-11.4598615582757,-14.1617511126203,
2.06368086793017E-11));
#13801=CARTESIAN_POINT('Ctrl Pts',(-8.59489616869782,-13.9867511126203,
4.9622656166752));
#13802=CARTESIAN_POINT('Ctrl Pts',(-5.72993077911996,-13.8117511126203,
9.92453123332977));
#13803=CARTESIAN_POINT('Ctrl Pts',(1.7871392867044E-11,-13.6367511126203,
9.92453123331945));
#13804=CARTESIAN_POINT('Ctrl Pts',(5.7299307791557,-13.4617511126203,9.92453123330913));
#13805=CARTESIAN_POINT('Ctrl Pts',(8.59489616871569,-13.2867511126203,4.96226561664425));
#13806=CARTESIAN_POINT('Ctrl Pts',(11.4598615582757,-13.1117511126203,-2.06354052510241E-11));
#13807=CARTESIAN_POINT('Ctrl Pts',(8.59489616869782,-12.9367511126203,-4.9622656166752));
#13808=CARTESIAN_POINT('Ctrl Pts',(5.72993077911996,-12.7617511126203,-9.92453123332976));
#13809=CARTESIAN_POINT('Ctrl Pts',(-1.78726082715848E-11,-12.5867511126203,
-9.92453123331945));
#13810=CARTESIAN_POINT('Ctrl Pts',(-5.7299307791557,-12.4117511126202,-9.92453123330913));
#13811=CARTESIAN_POINT('Ctrl Pts',(-8.59489616871569,-12.2367511126203,
-4.96226561664425));
#13812=CARTESIAN_POINT('Ctrl Pts',(-11.4598615582757,-12.0617511126203,
2.06368086793017E-11));
#13813=CARTESIAN_POINT('Ctrl Pts',(-8.59489616869782,-11.8867511126202,
4.9622656166752));
#13814=CARTESIAN_POINT('Ctrl Pts',(-5.72993077911996,-11.7117511126203,
9.92453123332977));
#13815=CARTESIAN_POINT('Ctrl Pts',(1.7871392867044E-11,-11.5367511126203,
9.92453123331945));
#13816=CARTESIAN_POINT('Ctrl Pts',(5.7299307791557,-11.3617511126203,9.92453123330913));
#13817=CARTESIAN_POINT('Ctrl Pts',(8.59489616871569,-11.1867511126203,4.96226561664425));
#13818=CARTESIAN_POINT('Ctrl Pts',(11.4598615582757,-11.0117511126203,-2.06354052510241E-11));
#13819=CARTESIAN_POINT('Ctrl Pts',(8.59489616869782,-10.8367511126203,-4.9622656166752));
#13820=CARTESIAN_POINT('Ctrl Pts',(5.72993077911996,-10.6617511126203,-9.92453123332976));
#13821=CARTESIAN_POINT('Ctrl Pts',(-1.78726082715848E-11,-10.4867511126203,
-9.92453123331945));
#13822=CARTESIAN_POINT('Ctrl Pts',(-5.7299307791557,-10.3117511126203,-9.92453123330913));
#13823=CARTESIAN_POINT('Ctrl Pts',(-8.59489616871569,-10.1367511126203,
-4.96226561664425));
#13824=CARTESIAN_POINT('Ctrl Pts',(-11.4598615582757,-9.96175111262027,
2.06368086793017E-11));
#13825=CARTESIAN_POINT('Ctrl Pts',(-8.59489616869782,-9.78675111262026,
4.9622656166752));
#13826=CARTESIAN_POINT('Ctrl Pts',(-5.72993077911996,-9.61175111262028,
9.92453123332977));
#13827=CARTESIAN_POINT('Ctrl Pts',(1.7871392867044E-11,-9.43675111262027,
9.92453123331945));
#13828=CARTESIAN_POINT('Ctrl Pts',(5.7299307791557,-9.26175111262026,9.92453123330913));
#13829=CARTESIAN_POINT('Ctrl Pts',(8.59489616871569,-9.08675111262028,4.96226561664425));
#13830=CARTESIAN_POINT('Ctrl Pts',(11.4598615582757,-8.91175111262028,-2.06354052510241E-11));
#13831=CARTESIAN_POINT('Ctrl Pts',(8.59489616869782,-8.73675111262026,-4.9622656166752));
#13832=CARTESIAN_POINT('Ctrl Pts',(5.72993077911996,-8.56175111262028,-9.92453123332976));
#13833=CARTESIAN_POINT('Ctrl Pts',(-1.78726082715848E-11,-8.38675111262027,
-9.92453123331945));
#13834=CARTESIAN_POINT('Ctrl Pts',(-5.7299307791557,-8.21175111262026,-9.92453123330913));
#13835=CARTESIAN_POINT('Ctrl Pts',(-8.59489616871569,-8.03675111262026,
-4.96226561664425));
#13836=CARTESIAN_POINT('Ctrl Pts',(-11.4598615582757,-7.86175111262028,
2.06368086793017E-11));
#13837=CARTESIAN_POINT('Ctrl Pts',(-8.59489616869782,-7.68675111262027,
4.9622656166752));
#13838=CARTESIAN_POINT('Ctrl Pts',(-5.72993077911996,-7.51175111262027,
9.92453123332977));
#13839=CARTESIAN_POINT('Ctrl Pts',(1.7871392867044E-11,-7.33675111262028,
9.92453123331945));
#13840=CARTESIAN_POINT('Ctrl Pts',(5.7299307791557,-7.16175111262027,9.92453123330913));
#13841=CARTESIAN_POINT('Ctrl Pts',(8.59489616871569,-6.98675111262026,4.96226561664425));
#13842=CARTESIAN_POINT('Ctrl Pts',(11.4598615582757,-6.81175111262029,-2.06354052510241E-11));
#13843=CARTESIAN_POINT('Ctrl Pts',(8.59489616869782,-6.63675111262027,-4.9622656166752));
#13844=CARTESIAN_POINT('Ctrl Pts',(5.72993077911996,-6.46175111262027,-9.92453123332976));
#13845=CARTESIAN_POINT('Ctrl Pts',(-1.78726082715848E-11,-6.28675111262028,
-9.92453123331945));
#13846=CARTESIAN_POINT('Ctrl Pts',(-5.7299307791557,-6.11175111262027,-9.92453123330913));
#13847=CARTESIAN_POINT('Ctrl Pts',(-8.59489616871569,-5.93675111262026,
-4.96226561664425));
#13848=CARTESIAN_POINT('Ctrl Pts',(-11.4598615582757,-5.76175111262029,
2.06368086793017E-11));
#13849=CARTESIAN_POINT('Ctrl Pts',(-8.59489616869782,-5.58675111262028,
4.9622656166752));
#13850=CARTESIAN_POINT('Ctrl Pts',(-5.72993077911996,-5.41175111262028,
9.92453123332977));
#13851=CARTESIAN_POINT('Ctrl Pts',(1.7871392867044E-11,-5.23675111262029,
9.92453123331945));
#13852=CARTESIAN_POINT('Ctrl Pts',(5.7299307791557,-5.06175111262028,9.92453123330913));
#13853=CARTESIAN_POINT('Ctrl Pts',(8.59489616871569,-4.88675111262027,4.96226561664425));
#13854=CARTESIAN_POINT('Ctrl Pts',(11.4598615582757,-4.7117511126203,-2.06354052510241E-11));
#13855=CARTESIAN_POINT('Ctrl Pts',(8.59489616869782,-4.53675111262028,-4.9622656166752));
#13856=CARTESIAN_POINT('Ctrl Pts',(5.72993077911996,-4.36175111262028,-9.92453123332976));
#13857=CARTESIAN_POINT('Ctrl Pts',(-1.78726082715848E-11,-4.18675111262029,
-9.92453123331945));
#13858=CARTESIAN_POINT('Ctrl Pts',(-5.7299307791557,-4.01175111262028,-9.92453123330913));
#13859=CARTESIAN_POINT('Ctrl Pts',(-8.59489616871569,-3.83675111262027,
-4.96226561664425));
#13860=CARTESIAN_POINT('Ctrl Pts',(-11.4598615582757,-3.66175111262027,
2.06368086793017E-11));
#13861=CARTESIAN_POINT('Ctrl Pts',(-8.59489616869782,-3.48675111262029,
4.9622656166752));
#13862=CARTESIAN_POINT('Ctrl Pts',(-5.72993077911996,-3.31175111262029,
9.92453123332977));
#13863=CARTESIAN_POINT('Ctrl Pts',(1.7871392867044E-11,-3.13675111262027,
9.92453123331945));
#13864=CARTESIAN_POINT('Ctrl Pts',(5.7299307791557,-2.96175111262029,9.92453123330913));
#13865=CARTESIAN_POINT('Ctrl Pts',(8.59489616871569,-2.78675111262028,4.96226561664425));
#13866=CARTESIAN_POINT('Ctrl Pts',(11.4598615582757,-2.61175111262027,-2.06354052510241E-11));
#13867=CARTESIAN_POINT('Ctrl Pts',(8.59489616869782,-2.43675111262029,-4.9622656166752));
#13868=CARTESIAN_POINT('Ctrl Pts',(5.72993077911996,-2.26175111262028,-9.92453123332976));
#13869=CARTESIAN_POINT('Ctrl Pts',(-1.78726082715848E-11,-2.08675111262027,
-9.92453123331945));
#13870=CARTESIAN_POINT('Ctrl Pts',(-5.7299307791557,-1.91175111262029,-9.92453123330913));
#13871=CARTESIAN_POINT('Ctrl Pts',(-8.59489616871569,-1.73675111262028,
-4.96226561664425));
#13872=CARTESIAN_POINT('Ctrl Pts',(-11.4598615582757,-1.56175111262028,
2.06368086793017E-11));
#13873=CARTESIAN_POINT('Ctrl Pts',(-8.59489616869782,-1.38675111262029,
4.9622656166752));
#13874=CARTESIAN_POINT('Ctrl Pts',(-5.72993077911996,-1.21175111262029,
9.92453123332977));
#13875=CARTESIAN_POINT('Ctrl Pts',(1.7871392867044E-11,-1.03675111262028,
9.92453123331945));
#13876=CARTESIAN_POINT('Ctrl Pts',(5.7299307791557,-0.861751112620297,9.92453123330913));
#13877=CARTESIAN_POINT('Ctrl Pts',(8.59489616871569,-0.686751112620287,
4.96226561664425));
#13878=CARTESIAN_POINT('Ctrl Pts',(11.4598615582757,-0.511751112620282,
-2.06354052510241E-11));
#13879=CARTESIAN_POINT('Ctrl Pts',(8.59489616869782,-0.336751112620298,
-4.9622656166752));
#13880=CARTESIAN_POINT('Ctrl Pts',(5.72993077911996,-0.161751112620292,
-9.92453123332976));
#13881=CARTESIAN_POINT('Ctrl Pts',(-1.78726082715848E-11,0.0132488873797187,
-9.92453123331945));
#13882=CARTESIAN_POINT('Ctrl Pts',(-5.7299307791557,0.188248887379698,-9.92453123330913));
#13883=CARTESIAN_POINT('Ctrl Pts',(-8.59489616871569,0.363248887379708,
-4.96226561664425));
#13884=CARTESIAN_POINT('Ctrl Pts',(-11.4598615582757,0.538248887379713,
2.06368086793017E-11));
#13885=CARTESIAN_POINT('Ctrl Pts',(-8.59489616869782,0.713248887379725,
4.9622656166752));
#13886=CARTESIAN_POINT('Ctrl Pts',(-5.72993077911996,0.888248887379703,
9.92453123332977));
#13887=CARTESIAN_POINT('Ctrl Pts',(1.7871392867044E-11,1.06324888737971,
9.92453123331945));
#13888=CARTESIAN_POINT('Ctrl Pts',(5.7299307791557,1.23824888737972,9.92453123330913));
#13889=CARTESIAN_POINT('Ctrl Pts',(8.59489616871569,1.4132488873797,4.96226561664425));
#13890=CARTESIAN_POINT('Ctrl Pts',(11.4598615582757,1.58824888737971,-2.06354052510241E-11));
#13891=CARTESIAN_POINT('Ctrl Pts',(8.59489616869782,1.76324888737972,-4.9622656166752));
#13892=CARTESIAN_POINT('Ctrl Pts',(5.72993077911996,1.9382488873797,-9.92453123332976));
#13893=CARTESIAN_POINT('Ctrl Pts',(-1.78726082715848E-11,2.11324888737971,
-9.92453123331945));
#13894=CARTESIAN_POINT('Ctrl Pts',(-5.7299307791557,2.28824888737971,-9.92453123330913));
#13895=CARTESIAN_POINT('Ctrl Pts',(-8.59489616871569,2.4632488873797,-4.96226561664425));
#13896=CARTESIAN_POINT('Ctrl Pts',(-11.4598615582757,2.6382488873797,2.06368086793017E-11));
#13897=CARTESIAN_POINT('Ctrl Pts',(-8.59489616869782,2.81324888737972,4.9622656166752));
#13898=CARTESIAN_POINT('Ctrl Pts',(-5.72993077911996,2.98824888737969,9.92453123332977));
#13899=CARTESIAN_POINT('Ctrl Pts',(1.7871392867044E-11,3.16324888737971,
9.92453123331945));
#13900=CARTESIAN_POINT('Ctrl Pts',(5.7299307791557,3.33824888737971,9.92453123330913));
#13901=CARTESIAN_POINT('Ctrl Pts',(8.59489616871569,3.51324888737969,4.96226561664425));
#13902=CARTESIAN_POINT('Ctrl Pts',(11.4598615582757,3.6882488873797,-2.06354052510241E-11));
#13903=CARTESIAN_POINT('Ctrl Pts',(8.59489616869782,3.86324888737971,-4.9622656166752));
#13904=CARTESIAN_POINT('Ctrl Pts',(5.72993077911996,4.03824888737969,-9.92453123332976));
#13905=CARTESIAN_POINT('Ctrl Pts',(-1.78726082715848E-11,4.2132488873797,
-9.92453123331945));
#13906=CARTESIAN_POINT('Ctrl Pts',(-5.7299307791557,4.3882488873797,-9.92453123330913));
#13907=CARTESIAN_POINT('Ctrl Pts',(-8.59489616871569,4.56324888737969,-4.96226561664425));
#13908=CARTESIAN_POINT('Ctrl Pts',(-11.4598615582757,4.73824888737969,2.06368086793017E-11));
#13909=CARTESIAN_POINT('Ctrl Pts',(-8.59489616869782,4.91324888737971,4.9622656166752));
#13910=CARTESIAN_POINT('Ctrl Pts',(-5.72993077911996,5.08824888737969,9.92453123332977));
#13911=CARTESIAN_POINT('Ctrl Pts',(1.7871392867044E-11,5.2632488873797,
9.92453123331945));
#13912=CARTESIAN_POINT('Ctrl Pts',(5.7299307791557,5.4382488873797,9.92453123330913));
#13913=CARTESIAN_POINT('Ctrl Pts',(8.59489616871569,5.61324888737971,4.96226561664425));
#13914=CARTESIAN_POINT('Ctrl Pts',(11.4598615582757,5.78824888737969,-2.06354052510241E-11));
#13915=CARTESIAN_POINT('Ctrl Pts',(8.59489616869782,5.9632488873797,-4.9622656166752));
#13916=CARTESIAN_POINT('Ctrl Pts',(5.72993077911996,6.1382488873797,-9.92453123332976));
#13917=CARTESIAN_POINT('Ctrl Pts',(-1.78726082715848E-11,6.31324888737969,
-9.92453123331945));
#13918=CARTESIAN_POINT('Ctrl Pts',(-5.7299307791557,6.4882488873797,-9.92453123330913));
#13919=CARTESIAN_POINT('Ctrl Pts',(-8.59489616871569,6.66324888737971,-4.96226561664425));
#13920=CARTESIAN_POINT('Ctrl Pts',(-11.4598615582757,6.83824888737969,2.06368086793017E-11));
#13921=CARTESIAN_POINT('Ctrl Pts',(-8.59489616869782,7.0132488873797,4.9622656166752));
#13922=CARTESIAN_POINT('Ctrl Pts',(-5.72993077911996,7.1882488873797,9.92453123332977));
#13923=CARTESIAN_POINT('Ctrl Pts',(1.7871392867044E-11,7.36324888737969,
9.92453123331945));
#13924=CARTESIAN_POINT('Ctrl Pts',(5.7299307791557,7.53824888737969,9.92453123330913));
#13925=CARTESIAN_POINT('Ctrl Pts',(8.59489616871569,7.7132488873797,4.96226561664425));
#13926=CARTESIAN_POINT('Ctrl Pts',(11.4598615582757,7.88824888737968,-2.06354052510241E-11));
#13927=CARTESIAN_POINT('Ctrl Pts',(8.59489616869782,8.06324888737969,-4.9622656166752));
#13928=CARTESIAN_POINT('Ctrl Pts',(5.72993077911996,8.2382488873797,-9.92453123332976));
#13929=CARTESIAN_POINT('Ctrl Pts',(-1.78726082715848E-11,8.41324888737968,
-9.92453123331945));
#13930=CARTESIAN_POINT('Ctrl Pts',(-5.7299307791557,8.58824888737968,-9.92453123330913));
#13931=CARTESIAN_POINT('Ctrl Pts',(-8.59489616871569,8.7632488873797,-4.96226561664425));
#13932=CARTESIAN_POINT('Ctrl Pts',(-11.4598615582757,8.93824888737968,2.06368086793017E-11));
#13933=CARTESIAN_POINT('Ctrl Pts',(-8.59489616869782,9.11324888737969,4.9622656166752));
#13934=CARTESIAN_POINT('Ctrl Pts',(-5.72993077911996,9.28824888737969,9.92453123332977));
#13935=CARTESIAN_POINT('Ctrl Pts',(1.7871392867044E-11,9.46324888737968,
9.92453123331945));
#13936=CARTESIAN_POINT('Ctrl Pts',(5.7299307791557,9.63824888737968,9.92453123330913));
#13937=CARTESIAN_POINT('Ctrl Pts',(8.59489616871569,9.81324888737969,4.96226561664425));
#13938=CARTESIAN_POINT('Ctrl Pts',(11.4598615582757,9.9882488873797,-2.06354052510241E-11));
#13939=CARTESIAN_POINT('Ctrl Pts',(8.59489616869782,10.1632488873797,-4.9622656166752));
#13940=CARTESIAN_POINT('Ctrl Pts',(5.72993077911996,10.3382488873797,-9.92453123332976));
#13941=CARTESIAN_POINT('Ctrl Pts',(-1.78726082715848E-11,10.5132488873797,
-9.92453123331945));
#13942=CARTESIAN_POINT('Ctrl Pts',(-5.7299307791557,10.6882488873797,-9.92453123330913));
#13943=CARTESIAN_POINT('Ctrl Pts',(-8.59489616871569,10.8632488873797,-4.96226561664425));
#13944=CARTESIAN_POINT('Ctrl Pts',(-11.4598615582757,11.0382488873797,2.06368086793017E-11));
#13945=CARTESIAN_POINT('Ctrl Pts',(-8.59489616869782,11.2132488873797,4.9622656166752));
#13946=CARTESIAN_POINT('Ctrl Pts',(-5.72993077911996,11.3882488873797,9.92453123332977));
#13947=CARTESIAN_POINT('Ctrl Pts',(1.7871392867044E-11,11.5632488873797,
9.92453123331945));
#13948=CARTESIAN_POINT('Ctrl Pts',(5.7299307791557,11.7382488873797,9.92453123330913));
#13949=CARTESIAN_POINT('Ctrl Pts',(8.59489616871569,11.9132488873797,4.96226561664425));
#13950=CARTESIAN_POINT('Ctrl Pts',(11.4598615582757,12.0882488873797,-2.06354052510241E-11));
#13951=CARTESIAN_POINT('Ctrl Pts',(8.59489616869782,12.2632488873797,-4.9622656166752));
#13952=CARTESIAN_POINT('Ctrl Pts',(5.72993077911996,12.4382488873797,-9.92453123332976));
#13953=CARTESIAN_POINT('Ctrl Pts',(-1.78726082715848E-11,12.6132488873797,
-9.92453123331945));
#13954=CARTESIAN_POINT('Ctrl Pts',(-5.7299307791557,12.7882488873797,-9.92453123330913));
#13955=CARTESIAN_POINT('Ctrl Pts',(-8.59489616871569,12.9632488873797,-4.96226561664425));
#13956=CARTESIAN_POINT('Ctrl Pts',(-11.4598615582757,13.1382488873797,2.06368086793017E-11));
#13957=CARTESIAN_POINT('Ctrl Pts',(-8.59489616869782,13.3132488873797,4.9622656166752));
#13958=CARTESIAN_POINT('Ctrl Pts',(-5.72993077911996,13.4882488873797,9.92453123332977));
#13959=CARTESIAN_POINT('Ctrl Pts',(1.7871392867044E-11,13.6632488873797,
9.92453123331945));
#13960=CARTESIAN_POINT('Ctrl Pts',(5.7299307791557,13.8382488873797,9.92453123330913));
#13961=CARTESIAN_POINT('Ctrl Pts',(8.59489616871569,14.0132488873797,4.96226561664425));
#13962=CARTESIAN_POINT('Ctrl Pts',(11.4598615582757,14.1882488873797,-2.06354052510241E-11));
#13963=CARTESIAN_POINT('Ctrl Pts',(8.59489616869782,14.3632488873797,-4.9622656166752));
#13964=CARTESIAN_POINT('Ctrl Pts',(5.72993077911996,14.5382488873797,-9.92453123332976));
#13965=CARTESIAN_POINT('Ctrl Pts',(-1.78726082715848E-11,14.7132488873797,
-9.92453123331945));
#13966=CARTESIAN_POINT('Ctrl Pts',(-5.7299307791557,14.8882488873797,-9.92453123330913));
#13967=CARTESIAN_POINT('Ctrl Pts',(-8.59489616871569,15.0632488873797,-4.96226561664425));
#13968=CARTESIAN_POINT('Ctrl Pts',(-11.4598615582757,15.2382488873797,2.06368086793017E-11));
#13969=CARTESIAN_POINT('Ctrl Pts',(-8.59489616869782,15.4132488873797,4.9622656166752));
#13970=CARTESIAN_POINT('Ctrl Pts',(-5.72993077911996,15.5882488873797,9.92453123332977));
#13971=CARTESIAN_POINT('Ctrl Pts',(1.7871392867044E-11,15.7632488873797,
9.92453123331945));
#13972=CARTESIAN_POINT('Ctrl Pts',(5.7299307791557,15.9382488873797,9.92453123330913));
#13973=CARTESIAN_POINT('Ctrl Pts',(8.59489616871569,16.1132488873797,4.96226561664425));
#13974=CARTESIAN_POINT('Ctrl Pts',(11.4598615582757,16.2882488873797,-2.06354052510241E-11));
#13975=CARTESIAN_POINT('Ctrl Pts',(8.59489616869782,16.4632488873797,-4.9622656166752));
#13976=CARTESIAN_POINT('Ctrl Pts',(5.72993077911996,16.6382488873797,-9.92453123332976));
#13977=CARTESIAN_POINT('Ctrl Pts',(-1.78726082715848E-11,16.8132488873797,
-9.92453123331945));
#13978=CARTESIAN_POINT('Ctrl Pts',(-5.7299307791557,16.9882488873797,-9.92453123330913));
#13979=CARTESIAN_POINT('Ctrl Pts',(-8.59489616871569,17.1632488873797,-4.96226561664425));
#13980=CARTESIAN_POINT('Ctrl Pts',(-11.4598615582757,17.3382488873797,2.06368086793017E-11));
#13981=CARTESIAN_POINT('Ctrl Pts',(-8.59489616869782,17.5132488873797,4.9622656166752));
#13982=CARTESIAN_POINT('Ctrl Pts',(-5.72993077911996,17.6882488873797,9.92453123332977));
#13983=CARTESIAN_POINT('Ctrl Pts',(1.7871392867044E-11,17.8632488873797,
9.92453123331945));
#13984=CARTESIAN_POINT('Ctrl Pts',(5.7299307791557,18.0382488873797,9.92453123330913));
#13985=CARTESIAN_POINT('Ctrl Pts',(8.59489616871569,18.2132488873797,4.96226561664425));
#13986=CARTESIAN_POINT('Ctrl Pts',(11.4598615582757,18.3882488873797,-2.06354052510241E-11));
#13987=CARTESIAN_POINT('Ctrl Pts',(8.59489616869782,18.5632488873797,-4.9622656166752));
#13988=CARTESIAN_POINT('Ctrl Pts',(5.72993077911996,18.7382488873797,-9.92453123332976));
#13989=CARTESIAN_POINT('Ctrl Pts',(-1.78726082715848E-11,18.9132488873797,
-9.92453123331945));
#13990=CARTESIAN_POINT('Ctrl Pts',(-5.7299307791557,19.0882488873797,-9.92453123330913));
#13991=CARTESIAN_POINT('Ctrl Pts',(-8.59489616871569,19.2632488873797,-4.96226561664425));
#13992=CARTESIAN_POINT('Ctrl Pts',(-11.4598615582757,19.4382488873797,2.06368086793017E-11));
#13993=CARTESIAN_POINT('Ctrl Pts',(-8.59489616869782,19.6132488873797,4.9622656166752));
#13994=CARTESIAN_POINT('Ctrl Pts',(-5.72993077911996,19.7882488873797,9.92453123332977));
#13995=CARTESIAN_POINT('Ctrl Pts',(1.7871392867044E-11,19.9632488873797,
9.92453123331945));
#13996=CARTESIAN_POINT('Ctrl Pts',(5.7299307791557,20.1382488873797,9.92453123330913));
#13997=CARTESIAN_POINT('Ctrl Pts',(8.59489616871569,20.3132488873797,4.96226561664425));
#13998=CARTESIAN_POINT('Ctrl Pts',(11.4598615582757,20.4882488873796,-2.06354052510241E-11));
#13999=CARTESIAN_POINT('Ctrl Pts',(8.59489616869782,20.6632488873797,-4.9622656166752));
#14000=CARTESIAN_POINT('Ctrl Pts',(5.72993077911996,20.8382488873797,-9.92453123332976));
#14001=CARTESIAN_POINT('Ctrl Pts',(-1.78726082715848E-11,21.0132488873797,
-9.92453123331945));
#14002=CARTESIAN_POINT('Ctrl Pts',(-5.7299307791557,21.1882488873797,-9.92453123330913));
#14003=CARTESIAN_POINT('Ctrl Pts',(-8.59489616871569,21.3632488873797,-4.96226561664425));
#14004=CARTESIAN_POINT('Ctrl Pts',(-11.4598615582757,21.5382488873796,2.06368086793017E-11));
#14005=CARTESIAN_POINT('Ctrl Pts',(-8.59489616869782,21.7132488873797,4.9622656166752));
#14006=CARTESIAN_POINT('Ctrl Pts',(-5.72993077911996,21.8882488873797,9.92453123332977));
#14007=CARTESIAN_POINT('Ctrl Pts',(1.7871392867044E-11,22.0632488873797,
9.92453123331945));
#14008=CARTESIAN_POINT('Ctrl Pts',(5.7299307791557,22.2382488873797,9.92453123330913));
#14009=CARTESIAN_POINT('Ctrl Pts',(8.59489616871569,22.4132488873797,4.96226561664425));
#14010=CARTESIAN_POINT('Ctrl Pts',(11.4598615582757,22.5882488873796,-2.06354052510241E-11));
#14011=CARTESIAN_POINT('Ctrl Pts',(8.59489616869782,22.7632488873797,-4.9622656166752));
#14012=CARTESIAN_POINT('Ctrl Pts',(5.72993077911996,22.9382488873797,-9.92453123332976));
#14013=CARTESIAN_POINT('Ctrl Pts',(-1.78726082715848E-11,23.1132488873796,
-9.92453123331945));
#14014=CARTESIAN_POINT('Ctrl Pts',(-5.7299307791557,23.2882488873797,-9.92453123330913));
#14015=CARTESIAN_POINT('Ctrl Pts',(-8.59489616871569,23.4632488873797,-4.96226561664425));
#14016=CARTESIAN_POINT('Ctrl Pts',(-11.4598615582757,23.6382488873797,2.06368086793017E-11));
#14017=CARTESIAN_POINT('Ctrl Pts',(-8.59489616869782,23.8132488873797,4.9622656166752));
#14018=CARTESIAN_POINT('Ctrl Pts',(-5.72993077911996,23.9882488873797,9.92453123332977));
#14019=CARTESIAN_POINT('Ctrl Pts',(1.7871392867044E-11,24.1632488873797,
9.92453123331945));
#14020=CARTESIAN_POINT('Ctrl Pts',(5.7299307791557,24.3382488873796,9.92453123330913));
#14021=CARTESIAN_POINT('Ctrl Pts',(8.59489616871569,24.5132488873797,4.96226561664425));
#14022=CARTESIAN_POINT('Ctrl Pts',(11.4598615582757,24.6882488873797,-2.06354052510241E-11));
#14023=CARTESIAN_POINT('Ctrl Pts',(8.59489616869782,24.8632488873796,-4.9622656166752));
#14024=CARTESIAN_POINT('Ctrl Pts',(5.72993077911996,25.0382488873797,-9.92453123332976));
#14025=CARTESIAN_POINT('Ctrl Pts',(-1.78726082715848E-11,25.2132488873797,
-9.92453123331945));
#14026=CARTESIAN_POINT('Ctrl Pts',(-1.5130096486293E-11,-144.093981044533,
-8.40163410172683));
#14027=CARTESIAN_POINT('Ctrl Pts',(-4.85068571027985,-143.918981044533,
-8.40163410171809));
#14028=CARTESIAN_POINT('Ctrl Pts',(-7.27602856540465,-143.743981044533,
-4.20081705085031));
#14029=CARTESIAN_POINT('Ctrl Pts',(-9.70137142052945,-143.568981044533,
1.74701365207797E-11));
#14030=CARTESIAN_POINT('Ctrl Pts',(-7.27602856538952,-143.393981044533,
4.20081705087652));
#14031=CARTESIAN_POINT('Ctrl Pts',(-4.8506857102496,-143.218981044533,8.40163410173556));
#14032=CARTESIAN_POINT('Ctrl Pts',(1.5129067582862E-11,-143.043981044533,
8.40163410172683));
#14033=CARTESIAN_POINT('Ctrl Pts',(4.85068571027985,-142.868981044533,8.40163410171809));
#14034=CARTESIAN_POINT('Ctrl Pts',(7.27602856540465,-142.693981044533,4.20081705085031));
#14035=CARTESIAN_POINT('Ctrl Pts',(9.70137142052945,-142.518981044533,-1.7468948445434E-11));
#14036=CARTESIAN_POINT('Ctrl Pts',(7.27602856538952,-142.343981044533,-4.20081705087651));
#14037=CARTESIAN_POINT('Ctrl Pts',(4.8506857102496,-142.168981044533,-8.40163410173556));
#14038=CARTESIAN_POINT('Ctrl Pts',(-1.5130096486293E-11,-141.993981044533,
-8.40163410172683));
#14039=CARTESIAN_POINT('Ctrl Pts',(-4.85068571027985,-141.818981044533,
-8.40163410171809));
#14040=CARTESIAN_POINT('Ctrl Pts',(-7.27602856540465,-141.643981044533,
-4.20081705085031));
#14041=CARTESIAN_POINT('Ctrl Pts',(-9.70137142052945,-141.468981044533,
1.74701365207797E-11));
#14042=CARTESIAN_POINT('Ctrl Pts',(-7.27602856538952,-141.293981044533,
4.20081705087652));
#14043=CARTESIAN_POINT('Ctrl Pts',(-4.8506857102496,-141.118981044533,8.40163410173556));
#14044=CARTESIAN_POINT('Ctrl Pts',(1.5129067582862E-11,-140.943981044533,
8.40163410172683));
#14045=CARTESIAN_POINT('Ctrl Pts',(4.85068571027985,-140.768981044533,8.40163410171809));
#14046=CARTESIAN_POINT('Ctrl Pts',(7.27602856540465,-140.593981044533,4.20081705085031));
#14047=CARTESIAN_POINT('Ctrl Pts',(9.70137142052945,-140.418981044533,-1.7468948445434E-11));
#14048=CARTESIAN_POINT('Ctrl Pts',(7.27602856538952,-140.243981044533,-4.20081705087651));
#14049=CARTESIAN_POINT('Ctrl Pts',(4.8506857102496,-140.068981044533,-8.40163410173556));
#14050=CARTESIAN_POINT('Ctrl Pts',(-1.5130096486293E-11,-139.893981044533,
-8.40163410172683));
#14051=CARTESIAN_POINT('Ctrl Pts',(-4.85068571027985,-139.718981044533,
-8.40163410171809));
#14052=CARTESIAN_POINT('Ctrl Pts',(-7.27602856540465,-139.543981044533,
-4.20081705085031));
#14053=CARTESIAN_POINT('Ctrl Pts',(-9.70137142052945,-139.368981044533,
1.74701365207797E-11));
#14054=CARTESIAN_POINT('Ctrl Pts',(-7.27602856538952,-139.193981044533,
4.20081705087652));
#14055=CARTESIAN_POINT('Ctrl Pts',(-4.8506857102496,-139.018981044533,8.40163410173556));
#14056=CARTESIAN_POINT('Ctrl Pts',(1.5129067582862E-11,-138.843981044533,
8.40163410172683));
#14057=CARTESIAN_POINT('Ctrl Pts',(4.85068571027985,-138.668981044533,8.40163410171809));
#14058=CARTESIAN_POINT('Ctrl Pts',(7.27602856540465,-138.493981044533,4.20081705085031));
#14059=CARTESIAN_POINT('Ctrl Pts',(9.70137142052945,-138.318981044533,-1.7468948445434E-11));
#14060=CARTESIAN_POINT('Ctrl Pts',(7.27602856538952,-138.143981044533,-4.20081705087651));
#14061=CARTESIAN_POINT('Ctrl Pts',(4.8506857102496,-137.968981044533,-8.40163410173556));
#14062=CARTESIAN_POINT('Ctrl Pts',(-1.5130096486293E-11,-137.793981044533,
-8.40163410172683));
#14063=CARTESIAN_POINT('Ctrl Pts',(-4.85068571027985,-137.618981044533,
-8.40163410171809));
#14064=CARTESIAN_POINT('Ctrl Pts',(-7.27602856540465,-137.443981044533,
-4.20081705085031));
#14065=CARTESIAN_POINT('Ctrl Pts',(-9.70137142052945,-137.268981044533,
1.74701365207797E-11));
#14066=CARTESIAN_POINT('Ctrl Pts',(-7.27602856538952,-137.093981044533,
4.20081705087652));
#14067=CARTESIAN_POINT('Ctrl Pts',(-4.8506857102496,-136.918981044533,8.40163410173556));
#14068=CARTESIAN_POINT('Ctrl Pts',(1.5129067582862E-11,-136.743981044533,
8.40163410172683));
#14069=CARTESIAN_POINT('Ctrl Pts',(4.85068571027985,-136.568981044533,8.40163410171809));
#14070=CARTESIAN_POINT('Ctrl Pts',(7.27602856540465,-136.393981044533,4.20081705085031));
#14071=CARTESIAN_POINT('Ctrl Pts',(9.70137142052945,-136.218981044533,-1.7468948445434E-11));
#14072=CARTESIAN_POINT('Ctrl Pts',(7.27602856538952,-136.043981044533,-4.20081705087651));
#14073=CARTESIAN_POINT('Ctrl Pts',(4.8506857102496,-135.868981044533,-8.40163410173556));
#14074=CARTESIAN_POINT('Ctrl Pts',(-1.5130096486293E-11,-135.693981044533,
-8.40163410172683));
#14075=CARTESIAN_POINT('Ctrl Pts',(-4.85068571027985,-135.518981044533,
-8.40163410171809));
#14076=CARTESIAN_POINT('Ctrl Pts',(-7.27602856540465,-135.343981044533,
-4.20081705085031));
#14077=CARTESIAN_POINT('Ctrl Pts',(-9.70137142052945,-135.168981044533,
1.74701365207797E-11));
#14078=CARTESIAN_POINT('Ctrl Pts',(-7.27602856538952,-134.993981044533,
4.20081705087652));
#14079=CARTESIAN_POINT('Ctrl Pts',(-4.8506857102496,-134.818981044533,8.40163410173556));
#14080=CARTESIAN_POINT('Ctrl Pts',(1.5129067582862E-11,-134.643981044533,
8.40163410172683));
#14081=CARTESIAN_POINT('Ctrl Pts',(4.85068571027985,-134.468981044533,8.40163410171809));
#14082=CARTESIAN_POINT('Ctrl Pts',(7.27602856540465,-134.293981044533,4.20081705085031));
#14083=CARTESIAN_POINT('Ctrl Pts',(9.70137142052945,-134.118981044533,-1.7468948445434E-11));
#14084=CARTESIAN_POINT('Ctrl Pts',(7.27602856538952,-133.943981044533,-4.20081705087651));
#14085=CARTESIAN_POINT('Ctrl Pts',(4.8506857102496,-133.768981044533,-8.40163410173556));
#14086=CARTESIAN_POINT('Ctrl Pts',(-1.5130096486293E-11,-133.593981044533,
-8.40163410172683));
#14087=CARTESIAN_POINT('Ctrl Pts',(-4.85068571027985,-133.418981044533,
-8.40163410171809));
#14088=CARTESIAN_POINT('Ctrl Pts',(-7.27602856540465,-133.243981044533,
-4.20081705085031));
#14089=CARTESIAN_POINT('Ctrl Pts',(-9.70137142052945,-133.068981044533,
1.74701365207797E-11));
#14090=CARTESIAN_POINT('Ctrl Pts',(-7.27602856538952,-132.893981044533,
4.20081705087652));
#14091=CARTESIAN_POINT('Ctrl Pts',(-4.8506857102496,-132.718981044533,8.40163410173556));
#14092=CARTESIAN_POINT('Ctrl Pts',(1.5129067582862E-11,-132.543981044533,
8.40163410172683));
#14093=CARTESIAN_POINT('Ctrl Pts',(4.85068571027985,-132.368981044533,8.40163410171809));
#14094=CARTESIAN_POINT('Ctrl Pts',(7.27602856540465,-132.193981044533,4.20081705085031));
#14095=CARTESIAN_POINT('Ctrl Pts',(9.70137142052945,-132.018981044533,-1.7468948445434E-11));
#14096=CARTESIAN_POINT('Ctrl Pts',(7.27602856538952,-131.843981044533,-4.20081705087651));
#14097=CARTESIAN_POINT('Ctrl Pts',(4.8506857102496,-131.668981044533,-8.40163410173556));
#14098=CARTESIAN_POINT('Ctrl Pts',(-1.5130096486293E-11,-131.493981044533,
-8.40163410172683));
#14099=CARTESIAN_POINT('Ctrl Pts',(-4.85068571027985,-131.318981044533,
-8.40163410171809));
#14100=CARTESIAN_POINT('Ctrl Pts',(-7.27602856540465,-131.143981044533,
-4.20081705085031));
#14101=CARTESIAN_POINT('Ctrl Pts',(-9.70137142052945,-130.968981044533,
1.74701365207797E-11));
#14102=CARTESIAN_POINT('Ctrl Pts',(-7.27602856538952,-130.793981044533,
4.20081705087652));
#14103=CARTESIAN_POINT('Ctrl Pts',(-4.8506857102496,-130.618981044533,8.40163410173556));
#14104=CARTESIAN_POINT('Ctrl Pts',(1.5129067582862E-11,-130.443981044533,
8.40163410172683));
#14105=CARTESIAN_POINT('Ctrl Pts',(4.85068571027985,-130.268981044533,8.40163410171809));
#14106=CARTESIAN_POINT('Ctrl Pts',(7.27602856540465,-130.093981044533,4.20081705085031));
#14107=CARTESIAN_POINT('Ctrl Pts',(9.70137142052945,-129.918981044533,-1.7468948445434E-11));
#14108=CARTESIAN_POINT('Ctrl Pts',(7.27602856538952,-129.743981044533,-4.20081705087651));
#14109=CARTESIAN_POINT('Ctrl Pts',(4.8506857102496,-129.568981044533,-8.40163410173556));
#14110=CARTESIAN_POINT('Ctrl Pts',(-1.5130096486293E-11,-129.393981044533,
-8.40163410172683));
#14111=CARTESIAN_POINT('Ctrl Pts',(-4.85068571027985,-129.218981044533,
-8.40163410171809));
#14112=CARTESIAN_POINT('Ctrl Pts',(-7.27602856540465,-129.043981044533,
-4.20081705085031));
#14113=CARTESIAN_POINT('Ctrl Pts',(-9.70137142052945,-128.868981044533,
1.74701365207797E-11));
#14114=CARTESIAN_POINT('Ctrl Pts',(-7.27602856538952,-128.693981044533,
4.20081705087652));
#14115=CARTESIAN_POINT('Ctrl Pts',(-4.8506857102496,-128.518981044533,8.40163410173556));
#14116=CARTESIAN_POINT('Ctrl Pts',(1.5129067582862E-11,-128.343981044533,
8.40163410172683));
#14117=CARTESIAN_POINT('Ctrl Pts',(4.85068571027985,-128.168981044533,8.40163410171809));
#14118=CARTESIAN_POINT('Ctrl Pts',(7.27602856540465,-127.993981044533,4.20081705085031));
#14119=CARTESIAN_POINT('Ctrl Pts',(9.70137142052945,-127.818981044533,-1.7468948445434E-11));
#14120=CARTESIAN_POINT('Ctrl Pts',(7.27602856538952,-127.643981044533,-4.20081705087651));
#14121=CARTESIAN_POINT('Ctrl Pts',(4.8506857102496,-127.468981044533,-8.40163410173556));
#14122=CARTESIAN_POINT('Ctrl Pts',(-1.5130096486293E-11,-127.293981044533,
-8.40163410172683));
#14123=CARTESIAN_POINT('Ctrl Pts',(-4.85068571027985,-127.118981044533,
-8.40163410171809));
#14124=CARTESIAN_POINT('Ctrl Pts',(-7.27602856540465,-126.943981044533,
-4.20081705085031));
#14125=CARTESIAN_POINT('Ctrl Pts',(-9.70137142052945,-126.768981044533,
1.74701365207797E-11));
#14126=CARTESIAN_POINT('Ctrl Pts',(-7.27602856538952,-126.593981044533,
4.20081705087652));
#14127=CARTESIAN_POINT('Ctrl Pts',(-4.8506857102496,-126.418981044533,8.40163410173556));
#14128=CARTESIAN_POINT('Ctrl Pts',(1.5129067582862E-11,-126.243981044533,
8.40163410172683));
#14129=CARTESIAN_POINT('Ctrl Pts',(4.85068571027985,-126.068981044533,8.40163410171809));
#14130=CARTESIAN_POINT('Ctrl Pts',(7.27602856540465,-125.893981044533,4.20081705085031));
#14131=CARTESIAN_POINT('Ctrl Pts',(9.70137142052945,-125.718981044533,-1.7468948445434E-11));
#14132=CARTESIAN_POINT('Ctrl Pts',(7.27602856538952,-125.543981044533,-4.20081705087651));
#14133=CARTESIAN_POINT('Ctrl Pts',(4.8506857102496,-125.368981044533,-8.40163410173556));
#14134=CARTESIAN_POINT('Ctrl Pts',(-1.5130096486293E-11,-125.193981044533,
-8.40163410172683));
#14135=CARTESIAN_POINT('Ctrl Pts',(-4.85068571027985,-125.018981044533,
-8.40163410171809));
#14136=CARTESIAN_POINT('Ctrl Pts',(-7.27602856540465,-124.843981044533,
-4.20081705085031));
#14137=CARTESIAN_POINT('Ctrl Pts',(-9.70137142052945,-124.668981044533,
1.74701365207797E-11));
#14138=CARTESIAN_POINT('Ctrl Pts',(-7.27602856538952,-124.493981044533,
4.20081705087652));
#14139=CARTESIAN_POINT('Ctrl Pts',(-4.8506857102496,-124.318981044533,8.40163410173556));
#14140=CARTESIAN_POINT('Ctrl Pts',(1.5129067582862E-11,-124.143981044533,
8.40163410172683));
#14141=CARTESIAN_POINT('Ctrl Pts',(4.85068571027985,-123.968981044533,8.40163410171809));
#14142=CARTESIAN_POINT('Ctrl Pts',(7.27602856540465,-123.793981044533,4.20081705085031));
#14143=CARTESIAN_POINT('Ctrl Pts',(9.70137142052945,-123.618981044533,-1.7468948445434E-11));
#14144=CARTESIAN_POINT('Ctrl Pts',(7.27602856538952,-123.443981044533,-4.20081705087651));
#14145=CARTESIAN_POINT('Ctrl Pts',(4.8506857102496,-123.268981044533,-8.40163410173556));
#14146=CARTESIAN_POINT('Ctrl Pts',(-1.5130096486293E-11,-123.093981044533,
-8.40163410172683));
#14147=CARTESIAN_POINT('Ctrl Pts',(-4.85068571027985,-122.918981044533,
-8.40163410171809));
#14148=CARTESIAN_POINT('Ctrl Pts',(-7.27602856540465,-122.743981044533,
-4.20081705085031));
#14149=CARTESIAN_POINT('Ctrl Pts',(-9.70137142052945,-122.568981044533,
1.74701365207797E-11));
#14150=CARTESIAN_POINT('Ctrl Pts',(-7.27602856538952,-122.393981044533,
4.20081705087652));
#14151=CARTESIAN_POINT('Ctrl Pts',(-4.8506857102496,-122.218981044533,8.40163410173556));
#14152=CARTESIAN_POINT('Ctrl Pts',(1.5129067582862E-11,-122.043981044533,
8.40163410172683));
#14153=CARTESIAN_POINT('Ctrl Pts',(4.85068571027985,-121.868981044533,8.40163410171809));
#14154=CARTESIAN_POINT('Ctrl Pts',(7.27602856540465,-121.693981044533,4.20081705085031));
#14155=CARTESIAN_POINT('Ctrl Pts',(9.70137142052945,-121.518981044533,-1.7468948445434E-11));
#14156=CARTESIAN_POINT('Ctrl Pts',(7.27602856538952,-121.343981044533,-4.20081705087651));
#14157=CARTESIAN_POINT('Ctrl Pts',(4.8506857102496,-121.168981044533,-8.40163410173556));
#14158=CARTESIAN_POINT('Ctrl Pts',(-1.5130096486293E-11,-120.993981044533,
-8.40163410172683));
#14159=CARTESIAN_POINT('Ctrl Pts',(-4.85068571027985,-120.818981044533,
-8.40163410171809));
#14160=CARTESIAN_POINT('Ctrl Pts',(-7.27602856540465,-120.643981044533,
-4.20081705085031));
#14161=CARTESIAN_POINT('Ctrl Pts',(-9.70137142052945,-120.468981044533,
1.74701365207797E-11));
#14162=CARTESIAN_POINT('Ctrl Pts',(-7.27602856538952,-120.293981044533,
4.20081705087652));
#14163=CARTESIAN_POINT('Ctrl Pts',(-4.8506857102496,-120.118981044533,8.40163410173556));
#14164=CARTESIAN_POINT('Ctrl Pts',(1.5129067582862E-11,-119.943981044533,
8.40163410172683));
#14165=CARTESIAN_POINT('Ctrl Pts',(4.85068571027985,-119.768981044533,8.40163410171809));
#14166=CARTESIAN_POINT('Ctrl Pts',(7.27602856540465,-119.593981044533,4.20081705085031));
#14167=CARTESIAN_POINT('Ctrl Pts',(9.70137142052945,-119.418981044533,-1.7468948445434E-11));
#14168=CARTESIAN_POINT('Ctrl Pts',(7.27602856538952,-119.243981044533,-4.20081705087651));
#14169=CARTESIAN_POINT('Ctrl Pts',(4.8506857102496,-119.068981044533,-8.40163410173556));
#14170=CARTESIAN_POINT('Ctrl Pts',(-1.5130096486293E-11,-118.893981044533,
-8.40163410172683));
#14171=CARTESIAN_POINT('Ctrl Pts',(-4.85068571027985,-118.718981044533,
-8.40163410171809));
#14172=CARTESIAN_POINT('Ctrl Pts',(-7.27602856540465,-118.543981044533,
-4.20081705085031));
#14173=CARTESIAN_POINT('Ctrl Pts',(-9.70137142052945,-118.368981044533,
1.74701365207797E-11));
#14174=CARTESIAN_POINT('Ctrl Pts',(-7.27602856538952,-118.193981044533,
4.20081705087652));
#14175=CARTESIAN_POINT('Ctrl Pts',(-4.8506857102496,-118.018981044533,8.40163410173556));
#14176=CARTESIAN_POINT('Ctrl Pts',(1.5129067582862E-11,-117.843981044533,
8.40163410172683));
#14177=CARTESIAN_POINT('Ctrl Pts',(4.85068571027985,-117.668981044533,8.40163410171809));
#14178=CARTESIAN_POINT('Ctrl Pts',(7.27602856540465,-117.493981044533,4.20081705085031));
#14179=CARTESIAN_POINT('Ctrl Pts',(9.70137142052945,-117.318981044533,-1.7468948445434E-11));
#14180=CARTESIAN_POINT('Ctrl Pts',(7.27602856538952,-117.143981044533,-4.20081705087651));
#14181=CARTESIAN_POINT('Ctrl Pts',(4.8506857102496,-116.968981044533,-8.40163410173556));
#14182=CARTESIAN_POINT('Ctrl Pts',(-1.5130096486293E-11,-116.793981044533,
-8.40163410172683));
#14183=CARTESIAN_POINT('Ctrl Pts',(-4.85068571027985,-116.618981044533,
-8.40163410171809));
#14184=CARTESIAN_POINT('Ctrl Pts',(-7.27602856540465,-116.443981044533,
-4.20081705085031));
#14185=CARTESIAN_POINT('Ctrl Pts',(-9.70137142052945,-116.268981044533,
1.74701365207797E-11));
#14186=CARTESIAN_POINT('Ctrl Pts',(-7.27602856538952,-116.093981044533,
4.20081705087652));
#14187=CARTESIAN_POINT('Ctrl Pts',(-4.8506857102496,-115.918981044533,8.40163410173556));
#14188=CARTESIAN_POINT('Ctrl Pts',(1.5129067582862E-11,-115.743981044533,
8.40163410172683));
#14189=CARTESIAN_POINT('Ctrl Pts',(4.85068571027985,-115.568981044533,8.40163410171809));
#14190=CARTESIAN_POINT('Ctrl Pts',(7.27602856540465,-115.393981044533,4.20081705085031));
#14191=CARTESIAN_POINT('Ctrl Pts',(9.70137142052945,-115.218981044533,-1.7468948445434E-11));
#14192=CARTESIAN_POINT('Ctrl Pts',(7.27602856538952,-115.043981044533,-4.20081705087651));
#14193=CARTESIAN_POINT('Ctrl Pts',(4.8506857102496,-114.868981044533,-8.40163410173556));
#14194=CARTESIAN_POINT('Ctrl Pts',(-1.5130096486293E-11,-114.693981044533,
-8.40163410172683));
#14195=CARTESIAN_POINT('Ctrl Pts',(-4.85068571027985,-114.518981044533,
-8.40163410171809));
#14196=CARTESIAN_POINT('Ctrl Pts',(-7.27602856540465,-114.343981044533,
-4.20081705085031));
#14197=CARTESIAN_POINT('Ctrl Pts',(-9.70137142052945,-114.168981044533,
1.74701365207797E-11));
#14198=CARTESIAN_POINT('Ctrl Pts',(-7.27602856538952,-113.993981044533,
4.20081705087652));
#14199=CARTESIAN_POINT('Ctrl Pts',(-4.8506857102496,-113.818981044533,8.40163410173556));
#14200=CARTESIAN_POINT('Ctrl Pts',(1.5129067582862E-11,-113.643981044533,
8.40163410172683));
#14201=CARTESIAN_POINT('Ctrl Pts',(4.85068571027985,-113.468981044533,8.40163410171809));
#14202=CARTESIAN_POINT('Ctrl Pts',(7.27602856540465,-113.293981044533,4.20081705085031));
#14203=CARTESIAN_POINT('Ctrl Pts',(9.70137142052945,-113.118981044533,-1.7468948445434E-11));
#14204=CARTESIAN_POINT('Ctrl Pts',(7.27602856538952,-112.943981044533,-4.20081705087651));
#14205=CARTESIAN_POINT('Ctrl Pts',(4.8506857102496,-112.768981044533,-8.40163410173556));
#14206=CARTESIAN_POINT('Ctrl Pts',(-1.5130096486293E-11,-112.593981044533,
-8.40163410172683));
#14207=CARTESIAN_POINT('Ctrl Pts',(-4.85068571027985,-112.418981044533,
-8.40163410171809));
#14208=CARTESIAN_POINT('Ctrl Pts',(-7.27602856540465,-112.243981044533,
-4.20081705085031));
#14209=CARTESIAN_POINT('Ctrl Pts',(-9.70137142052945,-112.068981044533,
1.74701365207797E-11));
#14210=CARTESIAN_POINT('Ctrl Pts',(-7.27602856538952,-111.893981044533,
4.20081705087652));
#14211=CARTESIAN_POINT('Ctrl Pts',(-4.8506857102496,-111.718981044533,8.40163410173556));
#14212=CARTESIAN_POINT('Ctrl Pts',(1.5129067582862E-11,-111.543981044533,
8.40163410172683));
#14213=CARTESIAN_POINT('Ctrl Pts',(4.85068571027985,-111.368981044533,8.40163410171809));
#14214=CARTESIAN_POINT('Ctrl Pts',(7.27602856540465,-111.193981044533,4.20081705085031));
#14215=CARTESIAN_POINT('Ctrl Pts',(9.70137142052945,-111.018981044533,-1.7468948445434E-11));
#14216=CARTESIAN_POINT('Ctrl Pts',(7.27602856538952,-110.843981044533,-4.20081705087651));
#14217=CARTESIAN_POINT('Ctrl Pts',(4.8506857102496,-110.668981044533,-8.40163410173556));
#14218=CARTESIAN_POINT('Ctrl Pts',(-1.5130096486293E-11,-110.493981044533,
-8.40163410172683));
#14219=CARTESIAN_POINT('Ctrl Pts',(-4.85068571027985,-110.318981044533,
-8.40163410171809));
#14220=CARTESIAN_POINT('Ctrl Pts',(-7.27602856540465,-110.143981044533,
-4.20081705085031));
#14221=CARTESIAN_POINT('Ctrl Pts',(-9.70137142052945,-109.968981044533,
1.74701365207797E-11));
#14222=CARTESIAN_POINT('Ctrl Pts',(-7.27602856538952,-109.793981044533,
4.20081705087652));
#14223=CARTESIAN_POINT('Ctrl Pts',(-4.8506857102496,-109.618981044533,8.40163410173556));
#14224=CARTESIAN_POINT('Ctrl Pts',(1.5129067582862E-11,-109.443981044533,
8.40163410172683));
#14225=CARTESIAN_POINT('Ctrl Pts',(4.85068571027985,-109.268981044533,8.40163410171809));
#14226=CARTESIAN_POINT('Ctrl Pts',(7.27602856540465,-109.093981044533,4.20081705085031));
#14227=CARTESIAN_POINT('Ctrl Pts',(9.70137142052945,-108.918981044533,-1.7468948445434E-11));
#14228=CARTESIAN_POINT('Ctrl Pts',(7.27602856538952,-108.743981044533,-4.20081705087651));
#14229=CARTESIAN_POINT('Ctrl Pts',(4.8506857102496,-108.568981044533,-8.40163410173556));
#14230=CARTESIAN_POINT('Ctrl Pts',(-1.5130096486293E-11,-108.393981044533,
-8.40163410172683));
#14231=CARTESIAN_POINT('Ctrl Pts',(-4.85068571027985,-108.218981044533,
-8.40163410171809));
#14232=CARTESIAN_POINT('Ctrl Pts',(-7.27602856540465,-108.043981044533,
-4.20081705085031));
#14233=CARTESIAN_POINT('Ctrl Pts',(-9.70137142052945,-107.868981044533,
1.74701365207797E-11));
#14234=CARTESIAN_POINT('Ctrl Pts',(-7.27602856538952,-107.693981044533,
4.20081705087652));
#14235=CARTESIAN_POINT('Ctrl Pts',(-4.8506857102496,-107.518981044533,8.40163410173556));
#14236=CARTESIAN_POINT('Ctrl Pts',(1.5129067582862E-11,-107.343981044533,
8.40163410172683));
#14237=CARTESIAN_POINT('Ctrl Pts',(4.85068571027985,-107.168981044533,8.40163410171809));
#14238=CARTESIAN_POINT('Ctrl Pts',(7.27602856540465,-106.993981044533,4.20081705085031));
#14239=CARTESIAN_POINT('Ctrl Pts',(9.70137142052945,-106.818981044533,-1.7468948445434E-11));
#14240=CARTESIAN_POINT('Ctrl Pts',(7.27602856538952,-106.643981044533,-4.20081705087651));
#14241=CARTESIAN_POINT('Ctrl Pts',(4.8506857102496,-106.468981044533,-8.40163410173556));
#14242=CARTESIAN_POINT('Ctrl Pts',(-1.5130096486293E-11,-106.293981044533,
-8.40163410172683));
#14243=CARTESIAN_POINT('Ctrl Pts',(-4.85068571027985,-106.118981044533,
-8.40163410171809));
#14244=CARTESIAN_POINT('Ctrl Pts',(-7.27602856540465,-105.943981044533,
-4.20081705085031));
#14245=CARTESIAN_POINT('Ctrl Pts',(-9.70137142052945,-105.768981044533,
1.74701365207797E-11));
#14246=CARTESIAN_POINT('Ctrl Pts',(-7.27602856538952,-105.593981044533,
4.20081705087652));
#14247=CARTESIAN_POINT('Ctrl Pts',(-4.8506857102496,-105.418981044533,8.40163410173556));
#14248=CARTESIAN_POINT('Ctrl Pts',(1.5129067582862E-11,-105.243981044533,
8.40163410172683));
#14249=CARTESIAN_POINT('Ctrl Pts',(4.85068571027985,-105.068981044533,8.40163410171809));
#14250=CARTESIAN_POINT('Ctrl Pts',(7.27602856540465,-104.893981044533,4.20081705085031));
#14251=CARTESIAN_POINT('Ctrl Pts',(9.70137142052945,-104.718981044533,-1.7468948445434E-11));
#14252=CARTESIAN_POINT('Ctrl Pts',(7.27602856538952,-104.543981044533,-4.20081705087651));
#14253=CARTESIAN_POINT('Ctrl Pts',(4.8506857102496,-104.368981044533,-8.40163410173556));
#14254=CARTESIAN_POINT('Ctrl Pts',(-1.5130096486293E-11,-104.193981044533,
-8.40163410172683));
#14255=CARTESIAN_POINT('Ctrl Pts',(-4.85068571027985,-104.018981044533,
-8.40163410171809));
#14256=CARTESIAN_POINT('Ctrl Pts',(-7.27602856540465,-103.843981044533,
-4.20081705085031));
#14257=CARTESIAN_POINT('Ctrl Pts',(-9.70137142052945,-103.668981044533,
1.74701365207797E-11));
#14258=CARTESIAN_POINT('Ctrl Pts',(-7.27602856538952,-103.493981044533,
4.20081705087652));
#14259=CARTESIAN_POINT('Ctrl Pts',(-4.8506857102496,-103.318981044533,8.40163410173556));
#14260=CARTESIAN_POINT('Ctrl Pts',(1.5129067582862E-11,-103.143981044533,
8.40163410172683));
#14261=CARTESIAN_POINT('Ctrl Pts',(4.85068571027985,-102.968981044533,8.40163410171809));
#14262=CARTESIAN_POINT('Ctrl Pts',(7.27602856540465,-102.793981044533,4.20081705085031));
#14263=CARTESIAN_POINT('Ctrl Pts',(9.70137142052945,-102.618981044533,-1.7468948445434E-11));
#14264=CARTESIAN_POINT('Ctrl Pts',(7.27602856538952,-102.443981044533,-4.20081705087651));
#14265=CARTESIAN_POINT('Ctrl Pts',(4.8506857102496,-102.268981044533,-8.40163410173556));
#14266=CARTESIAN_POINT('Ctrl Pts',(-1.5130096486293E-11,-102.093981044533,
-8.40163410172683));
#14267=CARTESIAN_POINT('Ctrl Pts',(-4.85068571027985,-101.918981044533,
-8.40163410171809));
#14268=CARTESIAN_POINT('Ctrl Pts',(-7.27602856540465,-101.743981044533,
-4.20081705085031));
#14269=CARTESIAN_POINT('Ctrl Pts',(-9.70137142052945,-101.568981044533,
1.74701365207797E-11));
#14270=CARTESIAN_POINT('Ctrl Pts',(-7.27602856538952,-101.393981044533,
4.20081705087652));
#14271=CARTESIAN_POINT('Ctrl Pts',(-4.8506857102496,-101.218981044533,8.40163410173556));
#14272=CARTESIAN_POINT('Ctrl Pts',(1.5129067582862E-11,-101.043981044533,
8.40163410172683));
#14273=CARTESIAN_POINT('Ctrl Pts',(4.85068571027985,-100.868981044533,8.40163410171809));
#14274=CARTESIAN_POINT('Ctrl Pts',(7.27602856540465,-100.693981044533,4.20081705085031));
#14275=CARTESIAN_POINT('Ctrl Pts',(9.70137142052945,-100.518981044533,-1.7468948445434E-11));
#14276=CARTESIAN_POINT('Ctrl Pts',(7.27602856538952,-100.343981044533,-4.20081705087651));
#14277=CARTESIAN_POINT('Ctrl Pts',(4.8506857102496,-100.168981044533,-8.40163410173556));
#14278=CARTESIAN_POINT('Ctrl Pts',(-1.5130096486293E-11,-99.9939810445332,
-8.40163410172683));
#14279=CARTESIAN_POINT('Ctrl Pts',(-4.85068571027985,-99.8189810445332,
-8.40163410171809));
#14280=CARTESIAN_POINT('Ctrl Pts',(-7.27602856540465,-99.6439810445332,
-4.20081705085031));
#14281=CARTESIAN_POINT('Ctrl Pts',(-9.70137142052945,-99.4689810445332,
1.74701365207797E-11));
#14282=CARTESIAN_POINT('Ctrl Pts',(-7.27602856538952,-99.2939810445332,
4.20081705087652));
#14283=CARTESIAN_POINT('Ctrl Pts',(-4.8506857102496,-99.1189810445332,8.40163410173556));
#14284=CARTESIAN_POINT('Ctrl Pts',(1.5129067582862E-11,-98.9439810445332,
8.40163410172683));
#14285=CARTESIAN_POINT('Ctrl Pts',(4.85068571027985,-98.7689810445332,8.40163410171809));
#14286=CARTESIAN_POINT('Ctrl Pts',(7.27602856540465,-98.5939810445332,4.20081705085031));
#14287=CARTESIAN_POINT('Ctrl Pts',(9.70137142052945,-98.4189810445332,-1.7468948445434E-11));
#14288=CARTESIAN_POINT('Ctrl Pts',(7.27602856538952,-98.2439810445332,-4.20081705087651));
#14289=CARTESIAN_POINT('Ctrl Pts',(4.8506857102496,-98.0689810445332,-8.40163410173556));
#14290=CARTESIAN_POINT('Ctrl Pts',(-1.5130096486293E-11,-97.8939810445332,
-8.40163410172683));
#14291=CARTESIAN_POINT('Ctrl Pts',(-4.85068571027985,-97.7189810445332,
-8.40163410171809));
#14292=CARTESIAN_POINT('Ctrl Pts',(-7.27602856540465,-97.5439810445332,
-4.20081705085031));
#14293=CARTESIAN_POINT('Ctrl Pts',(-9.70137142052945,-97.3689810445332,
1.74701365207797E-11));
#14294=CARTESIAN_POINT('Ctrl Pts',(-7.27602856538952,-97.1939810445332,
4.20081705087652));
#14295=CARTESIAN_POINT('Ctrl Pts',(-4.8506857102496,-97.0189810445332,8.40163410173556));
#14296=CARTESIAN_POINT('Ctrl Pts',(1.5129067582862E-11,-96.8439810445332,
8.40163410172683));
#14297=CARTESIAN_POINT('Ctrl Pts',(4.85068571027985,-96.6689810445332,8.40163410171809));
#14298=CARTESIAN_POINT('Ctrl Pts',(7.27602856540465,-96.4939810445332,4.20081705085031));
#14299=CARTESIAN_POINT('Ctrl Pts',(9.70137142052945,-96.3189810445332,-1.7468948445434E-11));
#14300=CARTESIAN_POINT('Ctrl Pts',(7.27602856538952,-96.1439810445332,-4.20081705087651));
#14301=CARTESIAN_POINT('Ctrl Pts',(4.8506857102496,-95.9689810445332,-8.40163410173556));
#14302=CARTESIAN_POINT('Ctrl Pts',(-1.5130096486293E-11,-95.7939810445332,
-8.40163410172683));
#14303=CARTESIAN_POINT('Ctrl Pts',(-4.85068571027985,-95.6189810445332,
-8.40163410171809));
#14304=CARTESIAN_POINT('Ctrl Pts',(-7.27602856540465,-95.4439810445332,
-4.20081705085031));
#14305=CARTESIAN_POINT('Ctrl Pts',(-9.70137142052945,-95.2689810445332,
1.74701365207797E-11));
#14306=CARTESIAN_POINT('Ctrl Pts',(-7.27602856538952,-95.0939810445332,
4.20081705087652));
#14307=CARTESIAN_POINT('Ctrl Pts',(-4.8506857102496,-94.9189810445332,8.40163410173556));
#14308=CARTESIAN_POINT('Ctrl Pts',(1.5129067582862E-11,-94.7439810445332,
8.40163410172683));
#14309=CARTESIAN_POINT('Ctrl Pts',(4.85068571027985,-94.5689810445332,8.40163410171809));
#14310=CARTESIAN_POINT('Ctrl Pts',(7.27602856540465,-94.3939810445332,4.20081705085031));
#14311=CARTESIAN_POINT('Ctrl Pts',(9.70137142052945,-94.2189810445331,-1.7468948445434E-11));
#14312=CARTESIAN_POINT('Ctrl Pts',(7.27602856538952,-94.0439810445332,-4.20081705087651));
#14313=CARTESIAN_POINT('Ctrl Pts',(4.8506857102496,-93.8689810445332,-8.40163410173556));
#14314=CARTESIAN_POINT('Ctrl Pts',(-1.5130096486293E-11,-93.6939810445332,
-8.40163410172683));
#14315=CARTESIAN_POINT('Ctrl Pts',(-4.85068571027985,-93.5189810445332,
-8.40163410171809));
#14316=CARTESIAN_POINT('Ctrl Pts',(-7.27602856540465,-93.3439810445332,
-4.20081705085031));
#14317=CARTESIAN_POINT('Ctrl Pts',(-9.70137142052945,-93.1689810445332,
1.74701365207797E-11));
#14318=CARTESIAN_POINT('Ctrl Pts',(-7.27602856538952,-92.9939810445332,
4.20081705087652));
#14319=CARTESIAN_POINT('Ctrl Pts',(-4.8506857102496,-92.8189810445332,8.40163410173556));
#14320=CARTESIAN_POINT('Ctrl Pts',(1.5129067582862E-11,-92.6439810445332,
8.40163410172683));
#14321=CARTESIAN_POINT('Ctrl Pts',(4.85068571027985,-92.4689810445332,8.40163410171809));
#14322=CARTESIAN_POINT('Ctrl Pts',(7.27602856540465,-92.2939810445332,4.20081705085031));
#14323=CARTESIAN_POINT('Ctrl Pts',(9.70137142052945,-92.1189810445332,-1.7468948445434E-11));
#14324=CARTESIAN_POINT('Ctrl Pts',(7.27602856538952,-91.9439810445332,-4.20081705087651));
#14325=CARTESIAN_POINT('Ctrl Pts',(4.8506857102496,-91.7689810445332,-8.40163410173556));
#14326=CARTESIAN_POINT('Ctrl Pts',(-1.5130096486293E-11,-91.5939810445332,
-8.40163410172683));
#14327=CARTESIAN_POINT('Ctrl Pts',(-4.85068571027985,-91.4189810445332,
-8.40163410171809));
#14328=CARTESIAN_POINT('Ctrl Pts',(-7.27602856540465,-91.2439810445332,
-4.20081705085031));
#14329=CARTESIAN_POINT('Ctrl Pts',(-9.70137142052945,-91.0689810445332,
1.74701365207797E-11));
#14330=CARTESIAN_POINT('Ctrl Pts',(-7.27602856538952,-90.8939810445332,
4.20081705087652));
#14331=CARTESIAN_POINT('Ctrl Pts',(-4.8506857102496,-90.7189810445332,8.40163410173556));
#14332=CARTESIAN_POINT('Ctrl Pts',(1.5129067582862E-11,-90.5439810445332,
8.40163410172683));
#14333=CARTESIAN_POINT('Ctrl Pts',(4.85068571027985,-90.3689810445332,8.40163410171809));
#14334=CARTESIAN_POINT('Ctrl Pts',(7.27602856540465,-90.1939810445332,4.20081705085031));
#14335=CARTESIAN_POINT('Ctrl Pts',(9.70137142052945,-90.0189810445332,-1.7468948445434E-11));
#14336=CARTESIAN_POINT('Ctrl Pts',(7.27602856538952,-89.8439810445332,-4.20081705087651));
#14337=CARTESIAN_POINT('Ctrl Pts',(4.8506857102496,-89.6689810445332,-8.40163410173556));
#14338=CARTESIAN_POINT('Ctrl Pts',(-1.5130096486293E-11,-89.4939810445332,
-8.40163410172683));
#14339=CARTESIAN_POINT('Ctrl Pts',(-4.85068571027985,-89.3189810445332,
-8.40163410171809));
#14340=CARTESIAN_POINT('Ctrl Pts',(-7.27602856540465,-89.1439810445332,
-4.20081705085031));
#14341=CARTESIAN_POINT('Ctrl Pts',(-9.70137142052945,-88.9689810445332,
1.74701365207797E-11));
#14342=CARTESIAN_POINT('Ctrl Pts',(-7.27602856538952,-88.7939810445332,
4.20081705087652));
#14343=CARTESIAN_POINT('Ctrl Pts',(-4.8506857102496,-88.6189810445332,8.40163410173556));
#14344=CARTESIAN_POINT('Ctrl Pts',(1.5129067582862E-11,-88.4439810445332,
8.40163410172683));
#14345=CARTESIAN_POINT('Ctrl Pts',(4.85068571027985,-88.2689810445332,8.40163410171809));
#14346=CARTESIAN_POINT('Ctrl Pts',(7.27602856540465,-88.0939810445332,4.20081705085031));
#14347=CARTESIAN_POINT('Ctrl Pts',(9.70137142052945,-87.9189810445332,-1.7468948445434E-11));
#14348=CARTESIAN_POINT('Ctrl Pts',(7.27602856538952,-87.7439810445332,-4.20081705087651));
#14349=CARTESIAN_POINT('Ctrl Pts',(4.8506857102496,-87.5689810445332,-8.40163410173556));
#14350=CARTESIAN_POINT('Ctrl Pts',(-1.5130096486293E-11,-87.3939810445332,
-8.40163410172683));
#14351=CARTESIAN_POINT('Ctrl Pts',(-4.85068571027985,-87.2189810445332,
-8.40163410171809));
#14352=CARTESIAN_POINT('Ctrl Pts',(-7.27602856540465,-87.0439810445332,
-4.20081705085031));
#14353=CARTESIAN_POINT('Ctrl Pts',(-9.70137142052945,-86.8689810445332,
1.74701365207797E-11));
#14354=CARTESIAN_POINT('Ctrl Pts',(-7.27602856538952,-86.6939810445332,
4.20081705087652));
#14355=CARTESIAN_POINT('Ctrl Pts',(-4.8506857102496,-86.5189810445332,8.40163410173556));
#14356=CARTESIAN_POINT('Ctrl Pts',(1.5129067582862E-11,-86.3439810445332,
8.40163410172683));
#14357=CARTESIAN_POINT('Ctrl Pts',(4.85068571027985,-86.1689810445332,8.40163410171809));
#14358=CARTESIAN_POINT('Ctrl Pts',(7.27602856540465,-85.9939810445332,4.20081705085031));
#14359=CARTESIAN_POINT('Ctrl Pts',(9.70137142052945,-85.8189810445332,-1.7468948445434E-11));
#14360=CARTESIAN_POINT('Ctrl Pts',(7.27602856538952,-85.6439810445332,-4.20081705087651));
#14361=CARTESIAN_POINT('Ctrl Pts',(4.8506857102496,-85.4689810445332,-8.40163410173556));
#14362=CARTESIAN_POINT('Ctrl Pts',(-1.5130096486293E-11,-85.2939810445332,
-8.40163410172683));
#14363=CARTESIAN_POINT('Ctrl Pts',(-4.85068571027985,-85.1189810445332,
-8.40163410171809));
#14364=CARTESIAN_POINT('Ctrl Pts',(-7.27602856540465,-84.9439810445332,
-4.20081705085031));
#14365=CARTESIAN_POINT('Ctrl Pts',(-9.70137142052945,-84.7689810445332,
1.74701365207797E-11));
#14366=CARTESIAN_POINT('Ctrl Pts',(-7.27602856538952,-84.5939810445332,
4.20081705087652));
#14367=CARTESIAN_POINT('Ctrl Pts',(-4.8506857102496,-84.4189810445332,8.40163410173556));
#14368=CARTESIAN_POINT('Ctrl Pts',(1.5129067582862E-11,-84.2439810445332,
8.40163410172683));
#14369=CARTESIAN_POINT('Ctrl Pts',(4.85068571027985,-84.0689810445332,8.40163410171809));
#14370=CARTESIAN_POINT('Ctrl Pts',(7.27602856540465,-83.8939810445332,4.20081705085031));
#14371=CARTESIAN_POINT('Ctrl Pts',(9.70137142052945,-83.7189810445332,-1.7468948445434E-11));
#14372=CARTESIAN_POINT('Ctrl Pts',(7.27602856538952,-83.5439810445332,-4.20081705087651));
#14373=CARTESIAN_POINT('Ctrl Pts',(4.8506857102496,-83.3689810445332,-8.40163410173556));
#14374=CARTESIAN_POINT('Ctrl Pts',(-1.5130096486293E-11,-83.1939810445332,
-8.40163410172683));
#14375=CARTESIAN_POINT('Ctrl Pts',(-4.85068571027985,-83.0189810445332,
-8.40163410171809));
#14376=CARTESIAN_POINT('Ctrl Pts',(-7.27602856540465,-82.8439810445332,
-4.20081705085031));
#14377=CARTESIAN_POINT('Ctrl Pts',(-9.70137142052945,-82.6689810445332,
1.74701365207797E-11));
#14378=CARTESIAN_POINT('Ctrl Pts',(-7.27602856538952,-82.4939810445332,
4.20081705087652));
#14379=CARTESIAN_POINT('Ctrl Pts',(-4.8506857102496,-82.3189810445332,8.40163410173556));
#14380=CARTESIAN_POINT('Ctrl Pts',(1.5129067582862E-11,-82.1439810445332,
8.40163410172683));
#14381=CARTESIAN_POINT('Ctrl Pts',(4.85068571027985,-81.9689810445332,8.40163410171809));
#14382=CARTESIAN_POINT('Ctrl Pts',(7.27602856540465,-81.7939810445332,4.20081705085031));
#14383=CARTESIAN_POINT('Ctrl Pts',(9.70137142052945,-81.6189810445332,-1.7468948445434E-11));
#14384=CARTESIAN_POINT('Ctrl Pts',(7.27602856538952,-81.4439810445332,-4.20081705087651));
#14385=CARTESIAN_POINT('Ctrl Pts',(4.8506857102496,-81.2689810445332,-8.40163410173556));
#14386=CARTESIAN_POINT('Ctrl Pts',(-1.5130096486293E-11,-81.0939810445332,
-8.40163410172683));
#14387=CARTESIAN_POINT('Ctrl Pts',(-4.85068571027985,-80.9189810445332,
-8.40163410171809));
#14388=CARTESIAN_POINT('Ctrl Pts',(-7.27602856540465,-80.7439810445332,
-4.20081705085031));
#14389=CARTESIAN_POINT('Ctrl Pts',(-9.70137142052945,-80.5689810445332,
1.74701365207797E-11));
#14390=CARTESIAN_POINT('Ctrl Pts',(-7.27602856538952,-80.3939810445332,
4.20081705087652));
#14391=CARTESIAN_POINT('Ctrl Pts',(-4.8506857102496,-80.2189810445333,8.40163410173556));
#14392=CARTESIAN_POINT('Ctrl Pts',(1.5129067582862E-11,-80.0439810445332,
8.40163410172683));
#14393=CARTESIAN_POINT('Ctrl Pts',(4.85068571027985,-79.8689810445333,8.40163410171809));
#14394=CARTESIAN_POINT('Ctrl Pts',(7.27602856540465,-79.6939810445332,4.20081705085031));
#14395=CARTESIAN_POINT('Ctrl Pts',(9.70137142052945,-79.5189810445332,-1.7468948445434E-11));
#14396=CARTESIAN_POINT('Ctrl Pts',(7.27602856538952,-79.3439810445332,-4.20081705087651));
#14397=CARTESIAN_POINT('Ctrl Pts',(4.8506857102496,-79.1689810445332,-8.40163410173556));
#14398=CARTESIAN_POINT('Ctrl Pts',(-1.5130096486293E-11,-78.9939810445332,
-8.40163410172683));
#14399=CARTESIAN_POINT('Ctrl Pts',(-4.85068571027985,-78.8189810445332,
-8.40163410171809));
#14400=CARTESIAN_POINT('Ctrl Pts',(-7.27602856540465,-78.6439810445332,
-4.20081705085031));
#14401=CARTESIAN_POINT('Ctrl Pts',(-9.70137142052945,-78.4689810445332,
1.74701365207797E-11));
#14402=CARTESIAN_POINT('Ctrl Pts',(-7.27602856538952,-78.2939810445332,
4.20081705087652));
#14403=CARTESIAN_POINT('Ctrl Pts',(-4.8506857102496,-78.1189810445332,8.40163410173556));
#14404=CARTESIAN_POINT('Ctrl Pts',(1.5129067582862E-11,-77.9439810445332,
8.40163410172683));
#14405=CARTESIAN_POINT('Ctrl Pts',(4.85068571027985,-77.7689810445333,8.40163410171809));
#14406=CARTESIAN_POINT('Ctrl Pts',(7.27602856540465,-77.5939810445332,4.20081705085031));
#14407=CARTESIAN_POINT('Ctrl Pts',(9.70137142052945,-77.4189810445332,-1.7468948445434E-11));
#14408=CARTESIAN_POINT('Ctrl Pts',(7.27602856538952,-77.2439810445332,-4.20081705087651));
#14409=CARTESIAN_POINT('Ctrl Pts',(4.8506857102496,-77.0689810445332,-8.40163410173556));
#14410=CARTESIAN_POINT('Ctrl Pts',(-1.5130096486293E-11,-76.8939810445332,
-8.40163410172683));
#14411=CARTESIAN_POINT('Ctrl Pts',(-4.85068571027985,-76.7189810445333,
-8.40163410171809));
#14412=CARTESIAN_POINT('Ctrl Pts',(-7.27602856540465,-76.5439810445332,
-4.20081705085031));
#14413=CARTESIAN_POINT('Ctrl Pts',(-9.70137142052945,-76.3689810445332,
1.74701365207797E-11));
#14414=CARTESIAN_POINT('Ctrl Pts',(-7.27602856538952,-76.1939810445332,
4.20081705087652));
#14415=CARTESIAN_POINT('Ctrl Pts',(-4.8506857102496,-76.0189810445332,8.40163410173556));
#14416=CARTESIAN_POINT('Ctrl Pts',(1.5129067582862E-11,-75.8439810445332,
8.40163410172683));
#14417=CARTESIAN_POINT('Ctrl Pts',(4.85068571027985,-75.6689810445332,8.40163410171809));
#14418=CARTESIAN_POINT('Ctrl Pts',(7.27602856540465,-75.4939810445332,4.20081705085031));
#14419=CARTESIAN_POINT('Ctrl Pts',(9.70137142052945,-75.3189810445332,-1.7468948445434E-11));
#14420=CARTESIAN_POINT('Ctrl Pts',(7.27602856538952,-75.1439810445332,-4.20081705087651));
#14421=CARTESIAN_POINT('Ctrl Pts',(4.8506857102496,-74.9689810445332,-8.40163410173556));
#14422=CARTESIAN_POINT('Ctrl Pts',(-1.5130096486293E-11,-74.7939810445332,
-8.40163410172683));
#14423=CARTESIAN_POINT('Ctrl Pts',(-4.85068571027985,-74.6189810445332,
-8.40163410171809));
#14424=CARTESIAN_POINT('Ctrl Pts',(-7.27602856540465,-74.4439810445332,
-4.20081705085031));
#14425=CARTESIAN_POINT('Ctrl Pts',(-9.70137142052945,-74.2689810445332,
1.74701365207797E-11));
#14426=CARTESIAN_POINT('Ctrl Pts',(-7.27602856538952,-74.0939810445332,
4.20081705087652));
#14427=CARTESIAN_POINT('Ctrl Pts',(-4.8506857102496,-73.9189810445332,8.40163410173556));
#14428=CARTESIAN_POINT('Ctrl Pts',(1.5129067582862E-11,-73.7439810445332,
8.40163410172683));
#14429=CARTESIAN_POINT('Ctrl Pts',(4.85068571027985,-73.5689810445332,8.40163410171809));
#14430=CARTESIAN_POINT('Ctrl Pts',(7.27602856540465,-73.3939810445332,4.20081705085031));
#14431=CARTESIAN_POINT('Ctrl Pts',(9.70137142052945,-73.2189810445333,-1.7468948445434E-11));
#14432=CARTESIAN_POINT('Ctrl Pts',(7.27602856538952,-73.0439810445332,-4.20081705087651));
#14433=CARTESIAN_POINT('Ctrl Pts',(4.8506857102496,-72.8689810445332,-8.40163410173556));
#14434=CARTESIAN_POINT('Ctrl Pts',(-1.5130096486293E-11,-72.6939810445332,
-8.40163410172683));
#14435=CARTESIAN_POINT('Ctrl Pts',(-4.85068571027985,-72.5189810445332,
-8.40163410171809));
#14436=CARTESIAN_POINT('Ctrl Pts',(-7.27602856540465,-72.3439810445332,
-4.20081705085031));
#14437=CARTESIAN_POINT('Ctrl Pts',(-9.70137142052945,-72.1689810445333,
1.74701365207797E-11));
#14438=CARTESIAN_POINT('Ctrl Pts',(-7.27602856538952,-71.9939810445332,
4.20081705087652));
#14439=CARTESIAN_POINT('Ctrl Pts',(-4.8506857102496,-71.8189810445332,8.40163410173556));
#14440=CARTESIAN_POINT('Ctrl Pts',(1.5129067582862E-11,-71.6439810445332,
8.40163410172683));
#14441=CARTESIAN_POINT('Ctrl Pts',(4.85068571027985,-71.4689810445332,8.40163410171809));
#14442=CARTESIAN_POINT('Ctrl Pts',(7.27602856540465,-71.2939810445332,4.20081705085031));
#14443=CARTESIAN_POINT('Ctrl Pts',(9.70137142052945,-71.1189810445332,-1.7468948445434E-11));
#14444=CARTESIAN_POINT('Ctrl Pts',(7.27602856538952,-70.9439810445332,-4.20081705087651));
#14445=CARTESIAN_POINT('Ctrl Pts',(4.8506857102496,-70.7689810445332,-8.40163410173556));
#14446=CARTESIAN_POINT('Ctrl Pts',(-1.5130096486293E-11,-70.5939810445332,
-8.40163410172683));
#14447=CARTESIAN_POINT('Ctrl Pts',(-4.85068571027985,-70.4189810445332,
-8.40163410171809));
#14448=CARTESIAN_POINT('Ctrl Pts',(-7.27602856540465,-70.2439810445332,
-4.20081705085031));
#14449=CARTESIAN_POINT('Ctrl Pts',(-9.70137142052945,-70.0689810445332,
1.74701365207797E-11));
#14450=CARTESIAN_POINT('Ctrl Pts',(-7.27602856538952,-69.8939810445332,
4.20081705087652));
#14451=CARTESIAN_POINT('Ctrl Pts',(-4.8506857102496,-69.7189810445333,8.40163410173556));
#14452=CARTESIAN_POINT('Ctrl Pts',(1.5129067582862E-11,-69.5439810445333,
8.40163410172683));
#14453=CARTESIAN_POINT('Ctrl Pts',(4.85068571027985,-69.3689810445332,8.40163410171809));
#14454=CARTESIAN_POINT('Ctrl Pts',(7.27602856540465,-69.1939810445332,4.20081705085031));
#14455=CARTESIAN_POINT('Ctrl Pts',(9.70137142052945,-69.0189810445333,-1.7468948445434E-11));
#14456=CARTESIAN_POINT('Ctrl Pts',(7.27602856538952,-68.8439810445332,-4.20081705087651));
#14457=CARTESIAN_POINT('Ctrl Pts',(4.8506857102496,-68.6689810445332,-8.40163410173556));
#14458=CARTESIAN_POINT('Ctrl Pts',(-1.5130096486293E-11,-68.4939810445333,
-8.40163410172683));
#14459=CARTESIAN_POINT('Ctrl Pts',(-4.85068571027985,-68.3189810445332,
-8.40163410171809));
#14460=CARTESIAN_POINT('Ctrl Pts',(-7.27602856540465,-68.1439810445332,
-4.20081705085031));
#14461=CARTESIAN_POINT('Ctrl Pts',(-9.70137142052945,-67.9689810445333,
1.74701365207797E-11));
#14462=CARTESIAN_POINT('Ctrl Pts',(-7.27602856538952,-67.7939810445332,
4.20081705087652));
#14463=CARTESIAN_POINT('Ctrl Pts',(-4.8506857102496,-67.6189810445333,8.40163410173556));
#14464=CARTESIAN_POINT('Ctrl Pts',(1.5129067582862E-11,-67.4439810445333,
8.40163410172683));
#14465=CARTESIAN_POINT('Ctrl Pts',(4.85068571027985,-67.2689810445332,8.40163410171809));
#14466=CARTESIAN_POINT('Ctrl Pts',(7.27602856540465,-67.0939810445333,4.20081705085031));
#14467=CARTESIAN_POINT('Ctrl Pts',(9.70137142052945,-66.9189810445333,-1.7468948445434E-11));
#14468=CARTESIAN_POINT('Ctrl Pts',(7.27602856538952,-66.7439810445332,-4.20081705087651));
#14469=CARTESIAN_POINT('Ctrl Pts',(4.8506857102496,-66.5689810445333,-8.40163410173556));
#14470=CARTESIAN_POINT('Ctrl Pts',(-1.5130096486293E-11,-66.3939810445332,
-8.40163410172683));
#14471=CARTESIAN_POINT('Ctrl Pts',(-4.85068571027985,-66.2189810445332,
-8.40163410171809));
#14472=CARTESIAN_POINT('Ctrl Pts',(-7.27602856540465,-66.0439810445333,
-4.20081705085031));
#14473=CARTESIAN_POINT('Ctrl Pts',(-9.70137142052945,-65.8689810445332,
1.74701365207797E-11));
#14474=CARTESIAN_POINT('Ctrl Pts',(-7.27602856538952,-65.6939810445332,
4.20081705087652));
#14475=CARTESIAN_POINT('Ctrl Pts',(-4.8506857102496,-65.5189810445333,8.40163410173556));
#14476=CARTESIAN_POINT('Ctrl Pts',(1.5129067582862E-11,-65.3439810445333,
8.40163410172683));
#14477=CARTESIAN_POINT('Ctrl Pts',(4.85068571027985,-65.1689810445333,8.40163410171809));
#14478=CARTESIAN_POINT('Ctrl Pts',(7.27602856540465,-64.9939810445333,4.20081705085031));
#14479=CARTESIAN_POINT('Ctrl Pts',(9.70137142052945,-64.8189810445332,-1.7468948445434E-11));
#14480=CARTESIAN_POINT('Ctrl Pts',(7.27602856538952,-64.6439810445332,-4.20081705087651));
#14481=CARTESIAN_POINT('Ctrl Pts',(4.8506857102496,-64.4689810445333,-8.40163410173556));
#14482=CARTESIAN_POINT('Ctrl Pts',(-1.5130096486293E-11,-64.2939810445333,
-8.40163410172683));
#14483=CARTESIAN_POINT('Ctrl Pts',(-4.85068571027985,-64.1189810445333,
-8.40163410171809));
#14484=CARTESIAN_POINT('Ctrl Pts',(-7.27602856540465,-63.9439810445333,
-4.20081705085031));
#14485=CARTESIAN_POINT('Ctrl Pts',(-9.70137142052945,-63.7689810445333,
1.74701365207797E-11));
#14486=CARTESIAN_POINT('Ctrl Pts',(-7.27602856538952,-63.5939810445333,
4.20081705087652));
#14487=CARTESIAN_POINT('Ctrl Pts',(-4.8506857102496,-63.4189810445333,8.40163410173556));
#14488=CARTESIAN_POINT('Ctrl Pts',(1.5129067582862E-11,-63.2439810445333,
8.40163410172683));
#14489=CARTESIAN_POINT('Ctrl Pts',(4.85068571027985,-63.0689810445333,8.40163410171809));
#14490=CARTESIAN_POINT('Ctrl Pts',(7.27602856540465,-62.8939810445333,4.20081705085031));
#14491=CARTESIAN_POINT('Ctrl Pts',(9.70137142052945,-62.7189810445333,-1.7468948445434E-11));
#14492=CARTESIAN_POINT('Ctrl Pts',(7.27602856538952,-62.5439810445333,-4.20081705087651));
#14493=CARTESIAN_POINT('Ctrl Pts',(4.8506857102496,-62.3689810445333,-8.40163410173556));
#14494=CARTESIAN_POINT('Ctrl Pts',(-1.5130096486293E-11,-62.1939810445333,
-8.40163410172683));
#14495=CARTESIAN_POINT('Ctrl Pts',(-4.85068571027985,-62.0189810445333,
-8.40163410171809));
#14496=CARTESIAN_POINT('Ctrl Pts',(-7.27602856540465,-61.8439810445333,
-4.20081705085031));
#14497=CARTESIAN_POINT('Ctrl Pts',(-9.70137142052945,-61.6689810445332,
1.74701365207797E-11));
#14498=CARTESIAN_POINT('Ctrl Pts',(-7.27602856538952,-61.4939810445333,
4.20081705087652));
#14499=CARTESIAN_POINT('Ctrl Pts',(-4.8506857102496,-61.3189810445333,8.40163410173556));
#14500=CARTESIAN_POINT('Ctrl Pts',(1.5129067582862E-11,-61.1439810445333,
8.40163410172683));
#14501=CARTESIAN_POINT('Ctrl Pts',(4.85068571027985,-60.9689810445333,8.40163410171809));
#14502=CARTESIAN_POINT('Ctrl Pts',(7.27602856540465,-60.7939810445333,4.20081705085031));
#14503=CARTESIAN_POINT('Ctrl Pts',(9.70137142052945,-60.6189810445333,-1.7468948445434E-11));
#14504=CARTESIAN_POINT('Ctrl Pts',(7.27602856538952,-60.4439810445333,-4.20081705087651));
#14505=CARTESIAN_POINT('Ctrl Pts',(4.8506857102496,-60.2689810445333,-8.40163410173556));
#14506=CARTESIAN_POINT('Ctrl Pts',(-1.5130096486293E-11,-60.0939810445333,
-8.40163410172683));
#14507=CARTESIAN_POINT('Ctrl Pts',(-4.85068571027985,-59.9189810445333,
-8.40163410171809));
#14508=CARTESIAN_POINT('Ctrl Pts',(-7.27602856540465,-59.7439810445333,
-4.20081705085031));
#14509=CARTESIAN_POINT('Ctrl Pts',(-9.70137142052945,-59.5689810445332,
1.74701365207797E-11));
#14510=CARTESIAN_POINT('Ctrl Pts',(-7.27602856538952,-59.3939810445333,
4.20081705087652));
#14511=CARTESIAN_POINT('Ctrl Pts',(-4.8506857102496,-59.2189810445333,8.40163410173556));
#14512=CARTESIAN_POINT('Ctrl Pts',(1.5129067582862E-11,-59.0439810445332,
8.40163410172683));
#14513=CARTESIAN_POINT('Ctrl Pts',(4.85068571027985,-58.8689810445333,8.40163410171809));
#14514=CARTESIAN_POINT('Ctrl Pts',(7.27602856540465,-58.6939810445333,4.20081705085031));
#14515=CARTESIAN_POINT('Ctrl Pts',(9.70137142052945,-58.5189810445332,-1.7468948445434E-11));
#14516=CARTESIAN_POINT('Ctrl Pts',(7.27602856538952,-58.3439810445333,-4.20081705087651));
#14517=CARTESIAN_POINT('Ctrl Pts',(4.8506857102496,-58.1689810445333,-8.40163410173556));
#14518=CARTESIAN_POINT('Ctrl Pts',(-1.5130096486293E-11,-57.9939810445333,
-8.40163410172683));
#14519=CARTESIAN_POINT('Ctrl Pts',(-4.85068571027985,-57.8189810445333,
-8.40163410171809));
#14520=CARTESIAN_POINT('Ctrl Pts',(-7.27602856540465,-57.6439810445333,
-4.20081705085031));
#14521=CARTESIAN_POINT('Ctrl Pts',(-9.70137142052945,-57.4689810445332,
1.74701365207797E-11));
#14522=CARTESIAN_POINT('Ctrl Pts',(-7.27602856538952,-57.2939810445333,
4.20081705087652));
#14523=CARTESIAN_POINT('Ctrl Pts',(-4.8506857102496,-57.1189810445333,8.40163410173556));
#14524=CARTESIAN_POINT('Ctrl Pts',(1.5129067582862E-11,-56.9439810445333,
8.40163410172683));
#14525=CARTESIAN_POINT('Ctrl Pts',(4.85068571027985,-56.7689810445333,8.40163410171809));
#14526=CARTESIAN_POINT('Ctrl Pts',(7.27602856540465,-56.5939810445333,4.20081705085031));
#14527=CARTESIAN_POINT('Ctrl Pts',(9.70137142052945,-56.4189810445332,-1.7468948445434E-11));
#14528=CARTESIAN_POINT('Ctrl Pts',(7.27602856538952,-56.2439810445333,-4.20081705087651));
#14529=CARTESIAN_POINT('Ctrl Pts',(4.8506857102496,-56.0689810445333,-8.40163410173556));
#14530=CARTESIAN_POINT('Ctrl Pts',(-1.5130096486293E-11,-55.8939810445333,
-8.40163410172683));
#14531=CARTESIAN_POINT('Ctrl Pts',(-4.85068571027985,-55.7189810445333,
-8.40163410171809));
#14532=CARTESIAN_POINT('Ctrl Pts',(-7.27602856540465,-55.5439810445333,
-4.20081705085031));
#14533=CARTESIAN_POINT('Ctrl Pts',(-9.70137142052945,-55.3689810445333,
1.74701365207797E-11));
#14534=CARTESIAN_POINT('Ctrl Pts',(-7.27602856538952,-55.1939810445333,
4.20081705087652));
#14535=CARTESIAN_POINT('Ctrl Pts',(-4.8506857102496,-55.0189810445333,8.40163410173556));
#14536=CARTESIAN_POINT('Ctrl Pts',(1.5129067582862E-11,-54.8439810445333,
8.40163410172683));
#14537=CARTESIAN_POINT('Ctrl Pts',(4.85068571027985,-54.6689810445333,8.40163410171809));
#14538=CARTESIAN_POINT('Ctrl Pts',(7.27602856540465,-54.4939810445333,4.20081705085031));
#14539=CARTESIAN_POINT('Ctrl Pts',(9.70137142052945,-54.3189810445333,-1.7468948445434E-11));
#14540=CARTESIAN_POINT('Ctrl Pts',(7.27602856538952,-54.1439810445333,-4.20081705087651));
#14541=CARTESIAN_POINT('Ctrl Pts',(4.8506857102496,-53.9689810445333,-8.40163410173556));
#14542=CARTESIAN_POINT('Ctrl Pts',(-1.5130096486293E-11,-53.7939810445333,
-8.40163410172683));
#14543=CARTESIAN_POINT('Ctrl Pts',(-4.85068571027985,-53.6189810445333,
-8.40163410171809));
#14544=CARTESIAN_POINT('Ctrl Pts',(-7.27602856540465,-53.4439810445333,
-4.20081705085031));
#14545=CARTESIAN_POINT('Ctrl Pts',(-9.70137142052945,-53.2689810445333,
1.74701365207797E-11));
#14546=CARTESIAN_POINT('Ctrl Pts',(-7.27602856538952,-53.0939810445333,
4.20081705087652));
#14547=CARTESIAN_POINT('Ctrl Pts',(-4.8506857102496,-52.9189810445333,8.40163410173556));
#14548=CARTESIAN_POINT('Ctrl Pts',(1.5129067582862E-11,-52.7439810445333,
8.40163410172683));
#14549=CARTESIAN_POINT('Ctrl Pts',(4.85068571027985,-52.5689810445333,8.40163410171809));
#14550=CARTESIAN_POINT('Ctrl Pts',(7.27602856540465,-52.3939810445333,4.20081705085031));
#14551=CARTESIAN_POINT('Ctrl Pts',(9.70137142052945,-52.2189810445333,-1.7468948445434E-11));
#14552=CARTESIAN_POINT('Ctrl Pts',(7.27602856538952,-52.0439810445333,-4.20081705087651));
#14553=CARTESIAN_POINT('Ctrl Pts',(4.8506857102496,-51.8689810445333,-8.40163410173556));
#14554=CARTESIAN_POINT('Ctrl Pts',(-1.5130096486293E-11,-51.6939810445333,
-8.40163410172683));
#14555=CARTESIAN_POINT('Ctrl Pts',(-4.85068571027985,-51.5189810445333,
-8.40163410171809));
#14556=CARTESIAN_POINT('Ctrl Pts',(-7.27602856540465,-51.3439810445333,
-4.20081705085031));
#14557=CARTESIAN_POINT('Ctrl Pts',(-9.70137142052945,-51.1689810445333,
1.74701365207797E-11));
#14558=CARTESIAN_POINT('Ctrl Pts',(-7.27602856538952,-50.9939810445333,
4.20081705087652));
#14559=CARTESIAN_POINT('Ctrl Pts',(-4.8506857102496,-50.8189810445333,8.40163410173556));
#14560=CARTESIAN_POINT('Ctrl Pts',(1.5129067582862E-11,-50.6439810445333,
8.40163410172683));
#14561=CARTESIAN_POINT('Ctrl Pts',(4.85068571027985,-50.4689810445333,8.40163410171809));
#14562=CARTESIAN_POINT('Ctrl Pts',(7.27602856540465,-50.2939810445333,4.20081705085031));
#14563=CARTESIAN_POINT('Ctrl Pts',(9.70137142052945,-50.1189810445333,-1.7468948445434E-11));
#14564=CARTESIAN_POINT('Ctrl Pts',(7.27602856538952,-49.9439810445333,-4.20081705087651));
#14565=CARTESIAN_POINT('Ctrl Pts',(4.8506857102496,-49.7689810445333,-8.40163410173556));
#14566=CARTESIAN_POINT('Ctrl Pts',(-1.5130096486293E-11,-49.5939810445333,
-8.40163410172683));
#14567=CARTESIAN_POINT('Ctrl Pts',(-4.85068571027985,-49.4189810445333,
-8.40163410171809));
#14568=CARTESIAN_POINT('Ctrl Pts',(-7.27602856540465,-49.2439810445333,
-4.20081705085031));
#14569=CARTESIAN_POINT('Ctrl Pts',(-9.70137142052945,-49.0689810445333,
1.74701365207797E-11));
#14570=CARTESIAN_POINT('Ctrl Pts',(-7.27602856538952,-48.8939810445333,
4.20081705087652));
#14571=CARTESIAN_POINT('Ctrl Pts',(-4.8506857102496,-48.7189810445333,8.40163410173556));
#14572=CARTESIAN_POINT('Ctrl Pts',(1.5129067582862E-11,-48.5439810445333,
8.40163410172683));
#14573=CARTESIAN_POINT('Ctrl Pts',(4.85068571027985,-48.3689810445333,8.40163410171809));
#14574=CARTESIAN_POINT('Ctrl Pts',(7.27602856540465,-48.1939810445333,4.20081705085031));
#14575=CARTESIAN_POINT('Ctrl Pts',(9.70137142052945,-48.0189810445333,-1.7468948445434E-11));
#14576=CARTESIAN_POINT('Ctrl Pts',(7.27602856538952,-47.8439810445333,-4.20081705087651));
#14577=CARTESIAN_POINT('Ctrl Pts',(4.8506857102496,-47.6689810445333,-8.40163410173556));
#14578=CARTESIAN_POINT('Ctrl Pts',(-1.5130096486293E-11,-47.4939810445333,
-8.40163410172683));
#14579=CARTESIAN_POINT('Ctrl Pts',(-4.85068571027985,-47.3189810445333,
-8.40163410171809));
#14580=CARTESIAN_POINT('Ctrl Pts',(-7.27602856540465,-47.1439810445333,
-4.20081705085031));
#14581=CARTESIAN_POINT('Ctrl Pts',(-9.70137142052945,-46.9689810445333,
1.74701365207797E-11));
#14582=CARTESIAN_POINT('Ctrl Pts',(-7.27602856538952,-46.7939810445333,
4.20081705087652));
#14583=CARTESIAN_POINT('Ctrl Pts',(-4.8506857102496,-46.6189810445333,8.40163410173556));
#14584=CARTESIAN_POINT('Ctrl Pts',(1.5129067582862E-11,-46.4439810445333,
8.40163410172683));
#14585=CARTESIAN_POINT('Ctrl Pts',(4.85068571027985,-46.2689810445333,8.40163410171809));
#14586=CARTESIAN_POINT('Ctrl Pts',(7.27602856540465,-46.0939810445333,4.20081705085031));
#14587=CARTESIAN_POINT('Ctrl Pts',(9.70137142052945,-45.9189810445333,-1.7468948445434E-11));
#14588=CARTESIAN_POINT('Ctrl Pts',(7.27602856538952,-45.7439810445333,-4.20081705087651));
#14589=CARTESIAN_POINT('Ctrl Pts',(4.8506857102496,-45.5689810445333,-8.40163410173556));
#14590=CARTESIAN_POINT('Ctrl Pts',(-1.5130096486293E-11,-45.3939810445333,
-8.40163410172683));
#14591=CARTESIAN_POINT('Ctrl Pts',(-4.85068571027985,-45.2189810445333,
-8.40163410171809));
#14592=CARTESIAN_POINT('Ctrl Pts',(-7.27602856540465,-45.0439810445333,
-4.20081705085031));
#14593=CARTESIAN_POINT('Ctrl Pts',(-9.70137142052945,-44.8689810445333,
1.74701365207797E-11));
#14594=CARTESIAN_POINT('Ctrl Pts',(-7.27602856538952,-44.6939810445333,
4.20081705087652));
#14595=CARTESIAN_POINT('Ctrl Pts',(-4.8506857102496,-44.5189810445333,8.40163410173556));
#14596=CARTESIAN_POINT('Ctrl Pts',(1.5129067582862E-11,-44.3439810445333,
8.40163410172683));
#14597=CARTESIAN_POINT('Ctrl Pts',(4.85068571027985,-44.1689810445333,8.40163410171809));
#14598=CARTESIAN_POINT('Ctrl Pts',(7.27602856540465,-43.9939810445333,4.20081705085031));
#14599=CARTESIAN_POINT('Ctrl Pts',(9.70137142052945,-43.8189810445333,-1.7468948445434E-11));
#14600=CARTESIAN_POINT('Ctrl Pts',(7.27602856538952,-43.6439810445333,-4.20081705087651));
#14601=CARTESIAN_POINT('Ctrl Pts',(4.8506857102496,-43.4689810445333,-8.40163410173556));
#14602=CARTESIAN_POINT('Ctrl Pts',(-1.5130096486293E-11,-43.2939810445333,
-8.40163410172683));
#14603=CARTESIAN_POINT('Ctrl Pts',(-4.85068571027985,-43.1189810445333,
-8.40163410171809));
#14604=CARTESIAN_POINT('Ctrl Pts',(-7.27602856540465,-42.9439810445333,
-4.20081705085031));
#14605=CARTESIAN_POINT('Ctrl Pts',(-9.70137142052945,-42.7689810445333,
1.74701365207797E-11));
#14606=CARTESIAN_POINT('Ctrl Pts',(-7.27602856538952,-42.5939810445333,
4.20081705087652));
#14607=CARTESIAN_POINT('Ctrl Pts',(-4.8506857102496,-42.4189810445333,8.40163410173556));
#14608=CARTESIAN_POINT('Ctrl Pts',(1.5129067582862E-11,-42.2439810445333,
8.40163410172683));
#14609=CARTESIAN_POINT('Ctrl Pts',(4.85068571027985,-42.0689810445333,8.40163410171809));
#14610=CARTESIAN_POINT('Ctrl Pts',(7.27602856540465,-41.8939810445333,4.20081705085031));
#14611=CARTESIAN_POINT('Ctrl Pts',(9.70137142052945,-41.7189810445333,-1.7468948445434E-11));
#14612=CARTESIAN_POINT('Ctrl Pts',(7.27602856538952,-41.5439810445333,-4.20081705087651));
#14613=CARTESIAN_POINT('Ctrl Pts',(4.8506857102496,-41.3689810445333,-8.40163410173556));
#14614=CARTESIAN_POINT('Ctrl Pts',(-1.5130096486293E-11,-41.1939810445333,
-8.40163410172683));
#14615=CARTESIAN_POINT('Ctrl Pts',(-4.85068571027985,-41.0189810445333,
-8.40163410171809));
#14616=CARTESIAN_POINT('Ctrl Pts',(-7.27602856540465,-40.8439810445333,
-4.20081705085031));
#14617=CARTESIAN_POINT('Ctrl Pts',(-9.70137142052945,-40.6689810445333,
1.74701365207797E-11));
#14618=CARTESIAN_POINT('Ctrl Pts',(-7.27602856538952,-40.4939810445333,
4.20081705087652));
#14619=CARTESIAN_POINT('Ctrl Pts',(-4.8506857102496,-40.3189810445333,8.40163410173556));
#14620=CARTESIAN_POINT('Ctrl Pts',(1.5129067582862E-11,-40.1439810445333,
8.40163410172683));
#14621=CARTESIAN_POINT('Ctrl Pts',(4.85068571027985,-39.9689810445333,8.40163410171809));
#14622=CARTESIAN_POINT('Ctrl Pts',(7.27602856540465,-39.7939810445333,4.20081705085031));
#14623=CARTESIAN_POINT('Ctrl Pts',(9.70137142052945,-39.6189810445333,-1.7468948445434E-11));
#14624=CARTESIAN_POINT('Ctrl Pts',(7.27602856538952,-39.4439810445333,-4.20081705087651));
#14625=CARTESIAN_POINT('Ctrl Pts',(4.8506857102496,-39.2689810445333,-8.40163410173556));
#14626=CARTESIAN_POINT('Ctrl Pts',(-1.5130096486293E-11,-39.0939810445333,
-8.40163410172683));
#14627=CARTESIAN_POINT('Ctrl Pts',(-4.85068571027985,-38.9189810445333,
-8.40163410171809));
#14628=CARTESIAN_POINT('Ctrl Pts',(-7.27602856540465,-38.7439810445333,
-4.20081705085031));
#14629=CARTESIAN_POINT('Ctrl Pts',(-9.70137142052945,-38.5689810445333,
1.74701365207797E-11));
#14630=CARTESIAN_POINT('Ctrl Pts',(-7.27602856538952,-38.3939810445333,
4.20081705087652));
#14631=CARTESIAN_POINT('Ctrl Pts',(-4.8506857102496,-38.2189810445333,8.40163410173556));
#14632=CARTESIAN_POINT('Ctrl Pts',(1.5129067582862E-11,-38.0439810445333,
8.40163410172683));
#14633=CARTESIAN_POINT('Ctrl Pts',(4.85068571027985,-37.8689810445333,8.40163410171809));
#14634=CARTESIAN_POINT('Ctrl Pts',(7.27602856540465,-37.6939810445333,4.20081705085031));
#14635=CARTESIAN_POINT('Ctrl Pts',(9.70137142052945,-37.5189810445333,-1.7468948445434E-11));
#14636=CARTESIAN_POINT('Ctrl Pts',(7.27602856538952,-37.3439810445333,-4.20081705087651));
#14637=CARTESIAN_POINT('Ctrl Pts',(4.8506857102496,-37.1689810445333,-8.40163410173556));
#14638=CARTESIAN_POINT('Ctrl Pts',(-1.5130096486293E-11,-36.9939810445333,
-8.40163410172683));
#14639=CARTESIAN_POINT('Ctrl Pts',(-4.85068571027985,-36.8189810445333,
-8.40163410171809));
#14640=CARTESIAN_POINT('Ctrl Pts',(-7.27602856540465,-36.6439810445333,
-4.20081705085031));
#14641=CARTESIAN_POINT('Ctrl Pts',(-9.70137142052945,-36.4689810445333,
1.74701365207797E-11));
#14642=CARTESIAN_POINT('Ctrl Pts',(-7.27602856538952,-36.2939810445333,
4.20081705087652));
#14643=CARTESIAN_POINT('Ctrl Pts',(-4.8506857102496,-36.1189810445333,8.40163410173556));
#14644=CARTESIAN_POINT('Ctrl Pts',(1.5129067582862E-11,-35.9439810445333,
8.40163410172683));
#14645=CARTESIAN_POINT('Ctrl Pts',(4.85068571027985,-35.7689810445333,8.40163410171809));
#14646=CARTESIAN_POINT('Ctrl Pts',(7.27602856540465,-35.5939810445333,4.20081705085031));
#14647=CARTESIAN_POINT('Ctrl Pts',(9.70137142052945,-35.4189810445333,-1.7468948445434E-11));
#14648=CARTESIAN_POINT('Ctrl Pts',(7.27602856538952,-35.2439810445333,-4.20081705087651));
#14649=CARTESIAN_POINT('Ctrl Pts',(4.8506857102496,-35.0689810445333,-8.40163410173556));
#14650=CARTESIAN_POINT('Ctrl Pts',(-1.5130096486293E-11,-34.8939810445333,
-8.40163410172683));
#14651=CARTESIAN_POINT('Ctrl Pts',(-4.85068571027985,-34.7189810445333,
-8.40163410171809));
#14652=CARTESIAN_POINT('Ctrl Pts',(-7.27602856540465,-34.5439810445333,
-4.20081705085031));
#14653=CARTESIAN_POINT('Ctrl Pts',(-9.70137142052945,-34.3689810445333,
1.74701365207797E-11));
#14654=CARTESIAN_POINT('Ctrl Pts',(-7.27602856538952,-34.1939810445333,
4.20081705087652));
#14655=CARTESIAN_POINT('Ctrl Pts',(-4.8506857102496,-34.0189810445333,8.40163410173556));
#14656=CARTESIAN_POINT('Ctrl Pts',(1.5129067582862E-11,-33.8439810445333,
8.40163410172683));
#14657=CARTESIAN_POINT('Ctrl Pts',(4.85068571027985,-33.6689810445333,8.40163410171809));
#14658=CARTESIAN_POINT('Ctrl Pts',(7.27602856540465,-33.4939810445333,4.20081705085031));
#14659=CARTESIAN_POINT('Ctrl Pts',(9.70137142052945,-33.3189810445333,-1.7468948445434E-11));
#14660=CARTESIAN_POINT('Ctrl Pts',(7.27602856538952,-33.1439810445333,-4.20081705087651));
#14661=CARTESIAN_POINT('Ctrl Pts',(4.8506857102496,-32.9689810445333,-8.40163410173556));
#14662=CARTESIAN_POINT('Ctrl Pts',(-1.5130096486293E-11,-32.7939810445333,
-8.40163410172683));
#14663=CARTESIAN_POINT('Ctrl Pts',(-4.85068571027985,-32.6189810445333,
-8.40163410171809));
#14664=CARTESIAN_POINT('Ctrl Pts',(-7.27602856540465,-32.4439810445333,
-4.20081705085031));
#14665=CARTESIAN_POINT('Ctrl Pts',(-9.70137142052945,-32.2689810445333,
1.74701365207797E-11));
#14666=CARTESIAN_POINT('Ctrl Pts',(-7.27602856538952,-32.0939810445333,
4.20081705087652));
#14667=CARTESIAN_POINT('Ctrl Pts',(-4.8506857102496,-31.9189810445333,8.40163410173556));
#14668=CARTESIAN_POINT('Ctrl Pts',(1.5129067582862E-11,-31.7439810445333,
8.40163410172683));
#14669=CARTESIAN_POINT('Ctrl Pts',(4.85068571027985,-31.5689810445333,8.40163410171809));
#14670=CARTESIAN_POINT('Ctrl Pts',(7.27602856540465,-31.3939810445333,4.20081705085031));
#14671=CARTESIAN_POINT('Ctrl Pts',(9.70137142052945,-31.2189810445333,-1.7468948445434E-11));
#14672=CARTESIAN_POINT('Ctrl Pts',(7.27602856538952,-31.0439810445333,-4.20081705087651));
#14673=CARTESIAN_POINT('Ctrl Pts',(4.8506857102496,-30.8689810445333,-8.40163410173556));
#14674=CARTESIAN_POINT('Ctrl Pts',(-1.5130096486293E-11,-30.6939810445333,
-8.40163410172683));
#14675=CARTESIAN_POINT('Ctrl Pts',(-4.85068571027985,-30.5189810445333,
-8.40163410171809));
#14676=CARTESIAN_POINT('Ctrl Pts',(-7.27602856540465,-30.3439810445333,
-4.20081705085031));
#14677=CARTESIAN_POINT('Ctrl Pts',(-9.70137142052945,-30.1689810445333,
1.74701365207797E-11));
#14678=CARTESIAN_POINT('Ctrl Pts',(-7.27602856538952,-29.9939810445333,
4.20081705087652));
#14679=CARTESIAN_POINT('Ctrl Pts',(-4.8506857102496,-29.8189810445333,8.40163410173556));
#14680=CARTESIAN_POINT('Ctrl Pts',(1.5129067582862E-11,-29.6439810445333,
8.40163410172683));
#14681=CARTESIAN_POINT('Ctrl Pts',(4.85068571027985,-29.4689810445333,8.40163410171809));
#14682=CARTESIAN_POINT('Ctrl Pts',(7.27602856540465,-29.2939810445333,4.20081705085031));
#14683=CARTESIAN_POINT('Ctrl Pts',(9.70137142052945,-29.1189810445333,-1.7468948445434E-11));
#14684=CARTESIAN_POINT('Ctrl Pts',(7.27602856538952,-28.9439810445333,-4.20081705087651));
#14685=CARTESIAN_POINT('Ctrl Pts',(4.8506857102496,-28.7689810445333,-8.40163410173556));
#14686=CARTESIAN_POINT('Ctrl Pts',(-1.5130096486293E-11,-28.5939810445333,
-8.40163410172683));
#14687=CARTESIAN_POINT('Ctrl Pts',(-4.85068571027985,-28.4189810445333,
-8.40163410171809));
#14688=CARTESIAN_POINT('Ctrl Pts',(-7.27602856540465,-28.2439810445333,
-4.20081705085031));
#14689=CARTESIAN_POINT('Ctrl Pts',(-9.70137142052945,-28.0689810445333,
1.74701365207797E-11));
#14690=CARTESIAN_POINT('Ctrl Pts',(-7.27602856538952,-27.8939810445333,
4.20081705087652));
#14691=CARTESIAN_POINT('Ctrl Pts',(-4.8506857102496,-27.7189810445334,8.40163410173556));
#14692=CARTESIAN_POINT('Ctrl Pts',(1.5129067582862E-11,-27.5439810445333,
8.40163410172683));
#14693=CARTESIAN_POINT('Ctrl Pts',(4.85068571027985,-27.3689810445333,8.40163410171809));
#14694=CARTESIAN_POINT('Ctrl Pts',(7.27602856540465,-27.1939810445333,4.20081705085031));
#14695=CARTESIAN_POINT('Ctrl Pts',(9.70137142052945,-27.0189810445333,-1.7468948445434E-11));
#14696=CARTESIAN_POINT('Ctrl Pts',(7.27602856538952,-26.8439810445333,-4.20081705087651));
#14697=CARTESIAN_POINT('Ctrl Pts',(4.8506857102496,-26.6689810445333,-8.40163410173556));
#14698=CARTESIAN_POINT('Ctrl Pts',(-1.5130096486293E-11,-26.4939810445333,
-8.40163410172683));
#14699=CARTESIAN_POINT('Ctrl Pts',(-4.85068571027985,-26.3189810445333,
-8.40163410171809));
#14700=CARTESIAN_POINT('Ctrl Pts',(-7.27602856540465,-26.1439810445333,
-4.20081705085031));
#14701=CARTESIAN_POINT('Ctrl Pts',(-9.70137142052945,-25.9689810445333,
1.74701365207797E-11));
#14702=CARTESIAN_POINT('Ctrl Pts',(-7.27602856538952,-25.7939810445333,
4.20081705087652));
#14703=CARTESIAN_POINT('Ctrl Pts',(-4.8506857102496,-25.6189810445334,8.40163410173556));
#14704=CARTESIAN_POINT('Ctrl Pts',(1.5129067582862E-11,-25.4439810445333,
8.40163410172683));
#14705=CARTESIAN_POINT('Ctrl Pts',(4.85068571027985,-25.2689810445333,8.40163410171809));
#14706=CARTESIAN_POINT('Ctrl Pts',(7.27602856540465,-25.0939810445334,4.20081705085031));
#14707=CARTESIAN_POINT('Ctrl Pts',(9.70137142052945,-24.9189810445333,-1.7468948445434E-11));
#14708=CARTESIAN_POINT('Ctrl Pts',(7.27602856538952,-24.7439810445333,-4.20081705087651));
#14709=CARTESIAN_POINT('Ctrl Pts',(4.8506857102496,-24.5689810445334,-8.40163410173556));
#14710=CARTESIAN_POINT('Ctrl Pts',(-1.5130096486293E-11,-24.3939810445333,
-8.40163410172683));
#14711=CARTESIAN_POINT('Ctrl Pts',(-4.85068571027985,-24.2189810445334,
-8.40163410171809));
#14712=CARTESIAN_POINT('Ctrl Pts',(-7.27602856540465,-24.0439810445333,
-4.20081705085031));
#14713=CARTESIAN_POINT('Ctrl Pts',(-9.70137142052945,-23.8689810445333,
1.74701365207797E-11));
#14714=CARTESIAN_POINT('Ctrl Pts',(-7.27602856538952,-23.6939810445334,
4.20081705087652));
#14715=CARTESIAN_POINT('Ctrl Pts',(-4.8506857102496,-23.5189810445334,8.40163410173556));
#14716=CARTESIAN_POINT('Ctrl Pts',(1.5129067582862E-11,-23.3439810445333,
8.40163410172683));
#14717=CARTESIAN_POINT('Ctrl Pts',(4.85068571027985,-23.1689810445334,8.40163410171809));
#14718=CARTESIAN_POINT('Ctrl Pts',(7.27602856540465,-22.9939810445333,4.20081705085031));
#14719=CARTESIAN_POINT('Ctrl Pts',(9.70137142052945,-22.8189810445333,-1.7468948445434E-11));
#14720=CARTESIAN_POINT('Ctrl Pts',(7.27602856538952,-22.6439810445334,-4.20081705087651));
#14721=CARTESIAN_POINT('Ctrl Pts',(4.8506857102496,-22.4689810445334,-8.40163410173556));
#14722=CARTESIAN_POINT('Ctrl Pts',(-1.5130096486293E-11,-22.2939810445333,
-8.40163410172683));
#14723=CARTESIAN_POINT('Ctrl Pts',(-4.85068571027985,-22.1189810445334,
-8.40163410171809));
#14724=CARTESIAN_POINT('Ctrl Pts',(-7.27602856540465,-21.9439810445333,
-4.20081705085031));
#14725=CARTESIAN_POINT('Ctrl Pts',(-9.70137142052945,-21.7689810445334,
1.74701365207797E-11));
#14726=CARTESIAN_POINT('Ctrl Pts',(-7.27602856538952,-21.5939810445333,
4.20081705087652));
#14727=CARTESIAN_POINT('Ctrl Pts',(-4.8506857102496,-21.4189810445334,8.40163410173556));
#14728=CARTESIAN_POINT('Ctrl Pts',(1.5129067582862E-11,-21.2439810445334,
8.40163410172683));
#14729=CARTESIAN_POINT('Ctrl Pts',(4.85068571027985,-21.0689810445333,8.40163410171809));
#14730=CARTESIAN_POINT('Ctrl Pts',(7.27602856540465,-20.8939810445334,4.20081705085031));
#14731=CARTESIAN_POINT('Ctrl Pts',(9.70137142052945,-20.7189810445334,-1.7468948445434E-11));
#14732=CARTESIAN_POINT('Ctrl Pts',(7.27602856538952,-20.5439810445333,-4.20081705087651));
#14733=CARTESIAN_POINT('Ctrl Pts',(4.8506857102496,-20.3689810445334,-8.40163410173556));
#14734=CARTESIAN_POINT('Ctrl Pts',(-1.5130096486293E-11,-20.1939810445334,
-8.40163410172683));
#14735=CARTESIAN_POINT('Ctrl Pts',(-4.85068571027985,-20.0189810445333,
-8.40163410171809));
#14736=CARTESIAN_POINT('Ctrl Pts',(-7.27602856540465,-19.8439810445334,
-4.20081705085031));
#14737=CARTESIAN_POINT('Ctrl Pts',(-9.70137142052945,-19.6689810445333,
1.74701365207797E-11));
#14738=CARTESIAN_POINT('Ctrl Pts',(-7.27602856538952,-19.4939810445334,
4.20081705087652));
#14739=CARTESIAN_POINT('Ctrl Pts',(-4.8506857102496,-19.3189810445334,8.40163410173556));
#14740=CARTESIAN_POINT('Ctrl Pts',(1.5129067582862E-11,-19.1439810445333,
8.40163410172683));
#14741=CARTESIAN_POINT('Ctrl Pts',(4.85068571027985,-18.9689810445334,8.40163410171809));
#14742=CARTESIAN_POINT('Ctrl Pts',(7.27602856540465,-18.7939810445333,4.20081705085031));
#14743=CARTESIAN_POINT('Ctrl Pts',(9.70137142052945,-18.6189810445334,-1.7468948445434E-11));
#14744=CARTESIAN_POINT('Ctrl Pts',(7.27602856538952,-18.4439810445334,-4.20081705087651));
#14745=CARTESIAN_POINT('Ctrl Pts',(4.8506857102496,-18.2689810445334,-8.40163410173556));
#14746=CARTESIAN_POINT('Ctrl Pts',(-1.5130096486293E-11,-18.0939810445334,
-8.40163410172683));
#14747=CARTESIAN_POINT('Ctrl Pts',(-4.85068571027985,-17.9189810445334,
-8.40163410171809));
#14748=CARTESIAN_POINT('Ctrl Pts',(-7.27602856540465,-17.7439810445334,
-4.20081705085031));
#14749=CARTESIAN_POINT('Ctrl Pts',(-9.70137142052945,-17.5689810445334,
1.74701365207797E-11));
#14750=CARTESIAN_POINT('Ctrl Pts',(-7.27602856538952,-17.3939810445334,
4.20081705087652));
#14751=CARTESIAN_POINT('Ctrl Pts',(-4.8506857102496,-17.2189810445334,8.40163410173556));
#14752=CARTESIAN_POINT('Ctrl Pts',(1.5129067582862E-11,-17.0439810445334,
8.40163410172683));
#14753=CARTESIAN_POINT('Ctrl Pts',(4.85068571027985,-16.8689810445334,8.40163410171809));
#14754=CARTESIAN_POINT('Ctrl Pts',(7.27602856540465,-16.6939810445334,4.20081705085031));
#14755=CARTESIAN_POINT('Ctrl Pts',(9.70137142052945,-16.5189810445334,-1.7468948445434E-11));
#14756=CARTESIAN_POINT('Ctrl Pts',(7.27602856538952,-16.3439810445334,-4.20081705087651));
#14757=CARTESIAN_POINT('Ctrl Pts',(4.8506857102496,-16.1689810445334,-8.40163410173556));
#14758=CARTESIAN_POINT('Ctrl Pts',(-1.5130096486293E-11,-15.9939810445334,
-8.40163410172683));
#14759=CARTESIAN_POINT('Ctrl Pts',(-4.85068571027985,-15.8189810445334,
-8.40163410171809));
#14760=CARTESIAN_POINT('Ctrl Pts',(-7.27602856540465,-15.6439810445334,
-4.20081705085031));
#14761=CARTESIAN_POINT('Ctrl Pts',(-9.70137142052945,-15.4689810445334,
1.74701365207797E-11));
#14762=CARTESIAN_POINT('Ctrl Pts',(-7.27602856538952,-15.2939810445334,
4.20081705087652));
#14763=CARTESIAN_POINT('Ctrl Pts',(-4.8506857102496,-15.1189810445334,8.40163410173556));
#14764=CARTESIAN_POINT('Ctrl Pts',(1.5129067582862E-11,-14.9439810445334,
8.40163410172683));
#14765=CARTESIAN_POINT('Ctrl Pts',(4.85068571027985,-14.7689810445334,8.40163410171809));
#14766=CARTESIAN_POINT('Ctrl Pts',(7.27602856540465,-14.5939810445334,4.20081705085031));
#14767=CARTESIAN_POINT('Ctrl Pts',(9.70137142052945,-14.4189810445334,-1.7468948445434E-11));
#14768=CARTESIAN_POINT('Ctrl Pts',(7.27602856538952,-14.2439810445334,-4.20081705087651));
#14769=CARTESIAN_POINT('Ctrl Pts',(4.8506857102496,-14.0689810445334,-8.40163410173556));
#14770=CARTESIAN_POINT('Ctrl Pts',(-1.5130096486293E-11,-13.8939810445334,
-8.40163410172683));
#14771=CARTESIAN_POINT('Ctrl Pts',(-4.85068571027985,-13.7189810445334,
-8.40163410171809));
#14772=CARTESIAN_POINT('Ctrl Pts',(-7.27602856540465,-13.5439810445334,
-4.20081705085031));
#14773=CARTESIAN_POINT('Ctrl Pts',(-9.70137142052945,-13.3689810445334,
1.74701365207797E-11));
#14774=CARTESIAN_POINT('Ctrl Pts',(-7.27602856538952,-13.1939810445334,
4.20081705087652));
#14775=CARTESIAN_POINT('Ctrl Pts',(-4.8506857102496,-13.0189810445334,8.40163410173556));
#14776=CARTESIAN_POINT('Ctrl Pts',(1.5129067582862E-11,-12.8439810445334,
8.40163410172683));
#14777=CARTESIAN_POINT('Ctrl Pts',(4.85068571027985,-12.6689810445334,8.40163410171809));
#14778=CARTESIAN_POINT('Ctrl Pts',(7.27602856540465,-12.4939810445334,4.20081705085031));
#14779=CARTESIAN_POINT('Ctrl Pts',(9.70137142052945,-12.3189810445334,-1.7468948445434E-11));
#14780=CARTESIAN_POINT('Ctrl Pts',(7.27602856538952,-12.1439810445334,-4.20081705087651));
#14781=CARTESIAN_POINT('Ctrl Pts',(4.8506857102496,-11.9689810445334,-8.40163410173556));
#14782=CARTESIAN_POINT('Ctrl Pts',(-1.5130096486293E-11,-11.7939810445334,
-8.40163410172683));
#14783=CARTESIAN_POINT('Ctrl Pts',(-4.85068571027985,-11.6189810445334,
-8.40163410171809));
#14784=CARTESIAN_POINT('Ctrl Pts',(-7.27602856540465,-11.4439810445334,
-4.20081705085031));
#14785=CARTESIAN_POINT('Ctrl Pts',(-9.70137142052945,-11.2689810445334,
1.74701365207797E-11));
#14786=CARTESIAN_POINT('Ctrl Pts',(-7.27602856538952,-11.0939810445334,
4.20081705087652));
#14787=CARTESIAN_POINT('Ctrl Pts',(-4.8506857102496,-10.9189810445334,8.40163410173556));
#14788=CARTESIAN_POINT('Ctrl Pts',(1.5129067582862E-11,-10.7439810445334,
8.40163410172683));
#14789=CARTESIAN_POINT('Ctrl Pts',(4.85068571027985,-10.5689810445334,8.40163410171809));
#14790=CARTESIAN_POINT('Ctrl Pts',(7.27602856540465,-10.3939810445334,4.20081705085031));
#14791=CARTESIAN_POINT('Ctrl Pts',(9.70137142052945,-10.2189810445334,-1.7468948445434E-11));
#14792=CARTESIAN_POINT('Ctrl Pts',(7.27602856538952,-10.0439810445334,-4.20081705087651));
#14793=CARTESIAN_POINT('Ctrl Pts',(4.8506857102496,-9.86898104453339,-8.40163410173556));
#14794=CARTESIAN_POINT('Ctrl Pts',(-1.5130096486293E-11,-9.69398104453338,
-8.40163410172683));
#14795=CARTESIAN_POINT('Ctrl Pts',(-4.85068571027985,-9.51898104453338,
-8.40163410171809));
#14796=CARTESIAN_POINT('Ctrl Pts',(-7.27602856540465,-9.34398104453339,
-4.20081705085031));
#14797=CARTESIAN_POINT('Ctrl Pts',(-9.70137142052945,-9.16898104453338,
1.74701365207797E-11));
#14798=CARTESIAN_POINT('Ctrl Pts',(-7.27602856538952,-8.99398104453337,
4.20081705087652));
#14799=CARTESIAN_POINT('Ctrl Pts',(-4.8506857102496,-8.8189810445334,8.40163410173556));
#14800=CARTESIAN_POINT('Ctrl Pts',(1.5129067582862E-11,-8.64398104453338,
8.40163410172683));
#14801=CARTESIAN_POINT('Ctrl Pts',(4.85068571027985,-8.46898104453338,8.40163410171809));
#14802=CARTESIAN_POINT('Ctrl Pts',(7.27602856540465,-8.29398104453339,4.20081705085031));
#14803=CARTESIAN_POINT('Ctrl Pts',(9.70137142052945,-8.11898104453338,-1.7468948445434E-11));
#14804=CARTESIAN_POINT('Ctrl Pts',(7.27602856538952,-7.94398104453338,-4.20081705087651));
#14805=CARTESIAN_POINT('Ctrl Pts',(4.8506857102496,-7.7689810445334,-8.40163410173556));
#14806=CARTESIAN_POINT('Ctrl Pts',(-1.5130096486293E-11,-7.59398104453339,
-8.40163410172683));
#14807=CARTESIAN_POINT('Ctrl Pts',(-4.85068571027985,-7.41898104453339,
-8.40163410171809));
#14808=CARTESIAN_POINT('Ctrl Pts',(-7.27602856540465,-7.24398104453337,
-4.20081705085031));
#14809=CARTESIAN_POINT('Ctrl Pts',(-9.70137142052945,-7.06898104453339,
1.74701365207797E-11));
#14810=CARTESIAN_POINT('Ctrl Pts',(-7.27602856538952,-6.89398104453338,
4.20081705087652));
#14811=CARTESIAN_POINT('Ctrl Pts',(-4.8506857102496,-6.71898104453338,8.40163410173556));
#14812=CARTESIAN_POINT('Ctrl Pts',(1.5129067582862E-11,-6.54398104453339,
8.40163410172683));
#14813=CARTESIAN_POINT('Ctrl Pts',(4.85068571027985,-6.36898104453339,8.40163410171809));
#14814=CARTESIAN_POINT('Ctrl Pts',(7.27602856540465,-6.19398104453338,4.20081705085031));
#14815=CARTESIAN_POINT('Ctrl Pts',(9.70137142052945,-6.01898104453339,-1.7468948445434E-11));
#14816=CARTESIAN_POINT('Ctrl Pts',(7.27602856538952,-5.84398104453339,-4.20081705087651));
#14817=CARTESIAN_POINT('Ctrl Pts',(4.8506857102496,-5.66898104453338,-8.40163410173556));
#14818=CARTESIAN_POINT('Ctrl Pts',(-1.5130096486293E-11,-5.4939810445334,
-8.40163410172683));
#14819=CARTESIAN_POINT('Ctrl Pts',(-4.85068571027985,-5.3189810445334,-8.40163410171809));
#14820=CARTESIAN_POINT('Ctrl Pts',(-7.27602856540465,-5.14398104453338,
-4.20081705085031));
#14821=CARTESIAN_POINT('Ctrl Pts',(-9.70137142052945,-4.9689810445334,1.74701365207797E-11));
#14822=CARTESIAN_POINT('Ctrl Pts',(-7.27602856538952,-4.79398104453339,
4.20081705087652));
#14823=CARTESIAN_POINT('Ctrl Pts',(-4.8506857102496,-4.61898104453338,8.40163410173556));
#14824=CARTESIAN_POINT('Ctrl Pts',(1.5129067582862E-11,-4.4439810445334,
8.40163410172683));
#14825=CARTESIAN_POINT('Ctrl Pts',(4.85068571027985,-4.2689810445334,8.40163410171809));
#14826=CARTESIAN_POINT('Ctrl Pts',(7.27602856540465,-4.09398104453338,4.20081705085031));
#14827=CARTESIAN_POINT('Ctrl Pts',(9.70137142052945,-3.9189810445334,-1.7468948445434E-11));
#14828=CARTESIAN_POINT('Ctrl Pts',(7.27602856538952,-3.74398104453339,-4.20081705087651));
#14829=CARTESIAN_POINT('Ctrl Pts',(4.8506857102496,-3.56898104453339,-8.40163410173556));
#14830=CARTESIAN_POINT('Ctrl Pts',(-1.5130096486293E-11,-3.39398104453341,
-8.40163410172683));
#14831=CARTESIAN_POINT('Ctrl Pts',(-4.85068571027985,-3.21898104453341,
-8.40163410171809));
#14832=CARTESIAN_POINT('Ctrl Pts',(-7.27602856540465,-3.04398104453339,
-4.20081705085031));
#14833=CARTESIAN_POINT('Ctrl Pts',(-9.70137142052945,-2.86898104453339,
1.74701365207797E-11));
#14834=CARTESIAN_POINT('Ctrl Pts',(-7.27602856538952,-2.6939810445334,4.20081705087652));
#14835=CARTESIAN_POINT('Ctrl Pts',(-4.8506857102496,-2.51898104453339,8.40163410173556));
#14836=CARTESIAN_POINT('Ctrl Pts',(1.5129067582862E-11,-2.34398104453338,
8.40163410172683));
#14837=CARTESIAN_POINT('Ctrl Pts',(4.85068571027985,-2.1689810445334,8.40163410171809));
#14838=CARTESIAN_POINT('Ctrl Pts',(7.27602856540465,-1.99398104453339,4.20081705085031));
#14839=CARTESIAN_POINT('Ctrl Pts',(9.70137142052945,-1.81898104453339,-1.7468948445434E-11));
#14840=CARTESIAN_POINT('Ctrl Pts',(7.27602856538952,-1.6439810445334,-4.20081705087651));
#14841=CARTESIAN_POINT('Ctrl Pts',(4.8506857102496,-1.4689810445334,-8.40163410173556));
#14842=CARTESIAN_POINT('Ctrl Pts',(-1.5130096486293E-11,-1.29398104453339,
-8.40163410172683));
#14843=CARTESIAN_POINT('Ctrl Pts',(-4.85068571027985,-1.11898104453341,
-8.40163410171809));
#14844=CARTESIAN_POINT('Ctrl Pts',(-7.27602856540465,-0.943981044533398,
-4.20081705085031));
#14845=CARTESIAN_POINT('Ctrl Pts',(-9.70137142052945,-0.768981044533393,
1.74701365207797E-11));
#14846=CARTESIAN_POINT('Ctrl Pts',(-7.27602856538952,-0.593981044533408,
4.20081705087652));
#14847=CARTESIAN_POINT('Ctrl Pts',(-4.8506857102496,-0.418981044533402,
8.40163410173556));
#14848=CARTESIAN_POINT('Ctrl Pts',(1.5129067582862E-11,-0.243981044533391,
8.40163410172683));
#14849=CARTESIAN_POINT('Ctrl Pts',(4.85068571027985,-0.0689810445334119,
8.40163410171809));
#14850=CARTESIAN_POINT('Ctrl Pts',(7.27602856540465,0.106018955466598,4.20081705085031));
#14851=CARTESIAN_POINT('Ctrl Pts',(9.70137142052945,0.281018955466602,-1.7468948445434E-11));
#14852=CARTESIAN_POINT('Ctrl Pts',(7.27602856538952,0.456018955466587,-4.20081705087651));
#14853=CARTESIAN_POINT('Ctrl Pts',(4.8506857102496,0.631018955466593,-8.40163410173556));
#14854=CARTESIAN_POINT('Ctrl Pts',(-1.5130096486293E-11,0.806018955466604,
-8.40163410172683));
#14855=CARTESIAN_POINT('Ctrl Pts',(-4.85068571027985,0.981018955466583,
-8.40163410171809));
#14856=CARTESIAN_POINT('Ctrl Pts',(-7.27602856540465,1.15601895546659,-4.20081705085031));
#14857=CARTESIAN_POINT('Ctrl Pts',(-9.70137142052945,1.3310189554666,1.74701365207797E-11));
#14858=CARTESIAN_POINT('Ctrl Pts',(-7.27602856538952,1.50601895546661,4.20081705087652));
#14859=CARTESIAN_POINT('Ctrl Pts',(-4.8506857102496,1.68101895546659,8.40163410173556));
#14860=CARTESIAN_POINT('Ctrl Pts',(1.5129067582862E-11,1.8560189554666,
8.40163410172683));
#14861=CARTESIAN_POINT('Ctrl Pts',(4.85068571027985,2.0310189554666,8.40163410171809));
#14862=CARTESIAN_POINT('Ctrl Pts',(7.27602856540465,2.20601895546659,4.20081705085031));
#14863=CARTESIAN_POINT('Ctrl Pts',(9.70137142052945,2.38101895546659,-1.7468948445434E-11));
#14864=CARTESIAN_POINT('Ctrl Pts',(7.27602856538952,2.55601895546661,-4.20081705087651));
#14865=CARTESIAN_POINT('Ctrl Pts',(4.8506857102496,2.73101895546658,-8.40163410173556));
#14866=CARTESIAN_POINT('Ctrl Pts',(-1.5130096486293E-11,2.9060189554666,
-8.40163410172683));
#14867=CARTESIAN_POINT('Ctrl Pts',(-4.85068571027985,3.0810189554666,-8.40163410171809));
#14868=CARTESIAN_POINT('Ctrl Pts',(-7.27602856540465,3.25601895546658,-4.20081705085031));
#14869=CARTESIAN_POINT('Ctrl Pts',(-9.70137142052945,3.43101895546659,1.74701365207797E-11));
#14870=CARTESIAN_POINT('Ctrl Pts',(-7.27602856538952,3.6060189554666,4.20081705087652));
#14871=CARTESIAN_POINT('Ctrl Pts',(-4.8506857102496,3.78101895546658,8.40163410173556));
#14872=CARTESIAN_POINT('Ctrl Pts',(1.5129067582862E-11,3.95601895546659,
8.40163410172683));
#14873=CARTESIAN_POINT('Ctrl Pts',(4.85068571027985,4.13101895546659,8.40163410171809));
#14874=CARTESIAN_POINT('Ctrl Pts',(7.27602856540465,4.30601895546658,4.20081705085031));
#14875=CARTESIAN_POINT('Ctrl Pts',(9.70137142052945,4.48101895546658,-1.7468948445434E-11));
#14876=CARTESIAN_POINT('Ctrl Pts',(7.27602856538952,4.6560189554666,-4.20081705087651));
#14877=CARTESIAN_POINT('Ctrl Pts',(4.8506857102496,4.83101895546658,-8.40163410173556));
#14878=CARTESIAN_POINT('Ctrl Pts',(-1.5130096486293E-11,5.00601895546659,
-8.40163410172683));
#14879=CARTESIAN_POINT('Ctrl Pts',(-4.85068571027985,5.18101895546659,-8.40163410171809));
#14880=CARTESIAN_POINT('Ctrl Pts',(-7.27602856540465,5.35601895546657,-4.20081705085031));
#14881=CARTESIAN_POINT('Ctrl Pts',(-9.70137142052945,5.53101895546658,1.74701365207797E-11));
#14882=CARTESIAN_POINT('Ctrl Pts',(-7.27602856538952,5.70601895546659,4.20081705087652));
#14883=CARTESIAN_POINT('Ctrl Pts',(-4.8506857102496,5.88101895546657,8.40163410173556));
#14884=CARTESIAN_POINT('Ctrl Pts',(1.5129067582862E-11,6.05601895546658,
8.40163410172683));
#14885=CARTESIAN_POINT('Ctrl Pts',(4.85068571027985,6.23101895546658,8.40163410171809));
#14886=CARTESIAN_POINT('Ctrl Pts',(7.27602856540465,6.4060189554666,4.20081705085031));
#14887=CARTESIAN_POINT('Ctrl Pts',(9.70137142052945,6.58101895546657,-1.7468948445434E-11));
#14888=CARTESIAN_POINT('Ctrl Pts',(7.27602856538952,6.75601895546659,-4.20081705087651));
#14889=CARTESIAN_POINT('Ctrl Pts',(4.8506857102496,6.93101895546659,-8.40163410173556));
#14890=CARTESIAN_POINT('Ctrl Pts',(-1.5130096486293E-11,7.10601895546658,
-8.40163410172683));
#14891=CARTESIAN_POINT('Ctrl Pts',(-4.85068571027985,7.28101895546658,-8.40163410171809));
#14892=CARTESIAN_POINT('Ctrl Pts',(-7.27602856540465,7.45601895546659,-4.20081705085031));
#14893=CARTESIAN_POINT('Ctrl Pts',(-9.70137142052945,7.63101895546657,1.74701365207797E-11));
#14894=CARTESIAN_POINT('Ctrl Pts',(-7.27602856538952,7.80601895546658,4.20081705087652));
#14895=CARTESIAN_POINT('Ctrl Pts',(-4.8506857102496,7.98101895546658,8.40163410173556));
#14896=CARTESIAN_POINT('Ctrl Pts',(1.5129067582862E-11,8.15601895546657,
8.40163410172683));
#14897=CARTESIAN_POINT('Ctrl Pts',(4.85068571027985,8.33101895546658,8.40163410171809));
#14898=CARTESIAN_POINT('Ctrl Pts',(7.27602856540465,8.50601895546659,4.20081705085031));
#14899=CARTESIAN_POINT('Ctrl Pts',(9.70137142052945,8.68101895546657,-1.7468948445434E-11));
#14900=CARTESIAN_POINT('Ctrl Pts',(7.27602856538952,8.85601895546658,-4.20081705087651));
#14901=CARTESIAN_POINT('Ctrl Pts',(4.8506857102496,9.03101895546658,-8.40163410173556));
#14902=CARTESIAN_POINT('Ctrl Pts',(-1.5130096486293E-11,9.20601895546657,
-8.40163410172683));
#14903=CARTESIAN_POINT('Ctrl Pts',(-4.85068571027985,9.38101895546657,-8.40163410171809));
#14904=CARTESIAN_POINT('Ctrl Pts',(-7.27602856540465,9.55601895546659,-4.20081705085031));
#14905=CARTESIAN_POINT('Ctrl Pts',(-9.70137142052945,9.73101895546656,1.74701365207797E-11));
#14906=CARTESIAN_POINT('Ctrl Pts',(-7.27602856538952,9.90601895546657,4.20081705087652));
#14907=CARTESIAN_POINT('Ctrl Pts',(-4.8506857102496,10.0810189554666,8.40163410173556));
#14908=CARTESIAN_POINT('Ctrl Pts',(1.5129067582862E-11,10.2560189554666,
8.40163410172683));
#14909=CARTESIAN_POINT('Ctrl Pts',(4.85068571027985,10.4310189554666,8.40163410171809));
#14910=CARTESIAN_POINT('Ctrl Pts',(7.27602856540465,10.6060189554666,4.20081705085031));
#14911=CARTESIAN_POINT('Ctrl Pts',(9.70137142052945,10.7810189554666,-1.7468948445434E-11));
#14912=CARTESIAN_POINT('Ctrl Pts',(7.27602856538952,10.9560189554666,-4.20081705087651));
#14913=CARTESIAN_POINT('Ctrl Pts',(4.8506857102496,11.1310189554666,-8.40163410173556));
#14914=CARTESIAN_POINT('Ctrl Pts',(-1.5130096486293E-11,11.3060189554666,
-8.40163410172683));
#14915=CARTESIAN_POINT('Ctrl Pts',(-4.85068571027985,11.4810189554666,-8.40163410171809));
#14916=CARTESIAN_POINT('Ctrl Pts',(-7.27602856540465,11.6560189554666,-4.20081705085031));
#14917=CARTESIAN_POINT('Ctrl Pts',(-9.70137142052945,11.8310189554666,1.74701365207797E-11));
#14918=CARTESIAN_POINT('Ctrl Pts',(-7.27602856538952,12.0060189554666,4.20081705087652));
#14919=CARTESIAN_POINT('Ctrl Pts',(-4.8506857102496,12.1810189554666,8.40163410173556));
#14920=CARTESIAN_POINT('Ctrl Pts',(1.5129067582862E-11,12.3560189554666,
8.40163410172683));
#14921=CARTESIAN_POINT('Ctrl Pts',(4.85068571027985,12.5310189554666,8.40163410171809));
#14922=CARTESIAN_POINT('Ctrl Pts',(7.27602856540465,12.7060189554666,4.20081705085031));
#14923=CARTESIAN_POINT('Ctrl Pts',(9.70137142052945,12.8810189554666,-1.7468948445434E-11));
#14924=CARTESIAN_POINT('Ctrl Pts',(7.27602856538952,13.0560189554666,-4.20081705087651));
#14925=CARTESIAN_POINT('Ctrl Pts',(4.8506857102496,13.2310189554666,-8.40163410173556));
#14926=CARTESIAN_POINT('Ctrl Pts',(-1.5130096486293E-11,13.4060189554666,
-8.40163410172683));
#14927=CARTESIAN_POINT('Ctrl Pts',(-4.85068571027985,13.5810189554666,-8.40163410171809));
#14928=CARTESIAN_POINT('Ctrl Pts',(-7.27602856540465,13.7560189554666,-4.20081705085031));
#14929=CARTESIAN_POINT('Ctrl Pts',(-9.70137142052945,13.9310189554666,1.74701365207797E-11));
#14930=CARTESIAN_POINT('Ctrl Pts',(-7.27602856538952,14.1060189554666,4.20081705087652));
#14931=CARTESIAN_POINT('Ctrl Pts',(-4.8506857102496,14.2810189554666,8.40163410173556));
#14932=CARTESIAN_POINT('Ctrl Pts',(1.5129067582862E-11,14.4560189554666,
8.40163410172683));
#14933=CARTESIAN_POINT('Ctrl Pts',(4.85068571027985,14.6310189554665,8.40163410171809));
#14934=CARTESIAN_POINT('Ctrl Pts',(7.27602856540465,14.8060189554666,4.20081705085031));
#14935=CARTESIAN_POINT('Ctrl Pts',(9.70137142052945,14.9810189554666,-1.7468948445434E-11));
#14936=CARTESIAN_POINT('Ctrl Pts',(7.27602856538952,15.1560189554666,-4.20081705087651));
#14937=CARTESIAN_POINT('Ctrl Pts',(4.8506857102496,15.3310189554666,-8.40163410173556));
#14938=CARTESIAN_POINT('Ctrl Pts',(-1.5130096486293E-11,15.5060189554666,
-8.40163410172683));
#14939=CARTESIAN_POINT('Ctrl Pts',(-4.85068571027985,15.6810189554666,-8.40163410171809));
#14940=CARTESIAN_POINT('Ctrl Pts',(-7.27602856540465,15.8560189554666,-4.20081705085031));
#14941=CARTESIAN_POINT('Ctrl Pts',(-9.70137142052945,16.0310189554666,1.74701365207797E-11));
#14942=CARTESIAN_POINT('Ctrl Pts',(-7.27602856538952,16.2060189554666,4.20081705087652));
#14943=CARTESIAN_POINT('Ctrl Pts',(-4.8506857102496,16.3810189554665,8.40163410173556));
#14944=CARTESIAN_POINT('Ctrl Pts',(1.5129067582862E-11,16.5560189554666,
8.40163410172683));
#14945=CARTESIAN_POINT('Ctrl Pts',(4.85068571027985,16.7310189554666,8.40163410171809));
#14946=CARTESIAN_POINT('Ctrl Pts',(7.27602856540465,16.9060189554666,4.20081705085031));
#14947=CARTESIAN_POINT('Ctrl Pts',(9.70137142052945,17.0810189554666,-1.7468948445434E-11));
#14948=CARTESIAN_POINT('Ctrl Pts',(7.27602856538952,17.2560189554666,-4.20081705087651));
#14949=CARTESIAN_POINT('Ctrl Pts',(4.8506857102496,17.4310189554665,-8.40163410173556));
#14950=CARTESIAN_POINT('Ctrl Pts',(-1.5130096486293E-11,17.6060189554666,
-8.40163410172683));
#14951=CARTESIAN_POINT('Ctrl Pts',(-4.85068571027985,17.7810189554666,-8.40163410171809));
#14952=CARTESIAN_POINT('Ctrl Pts',(-7.27602856540465,17.9560189554665,-4.20081705085031));
#14953=CARTESIAN_POINT('Ctrl Pts',(-9.70137142052945,18.1310189554665,1.74701365207797E-11));
#14954=CARTESIAN_POINT('Ctrl Pts',(-7.27602856538952,18.3060189554666,4.20081705087652));
#14955=CARTESIAN_POINT('Ctrl Pts',(-4.8506857102496,18.4810189554665,8.40163410173556));
#14956=CARTESIAN_POINT('Ctrl Pts',(1.5129067582862E-11,18.6560189554666,
8.40163410172683));
#14957=CARTESIAN_POINT('Ctrl Pts',(4.85068571027985,18.8310189554666,8.40163410171809));
#14958=CARTESIAN_POINT('Ctrl Pts',(7.27602856540465,19.0060189554665,4.20081705085031));
#14959=CARTESIAN_POINT('Ctrl Pts',(9.70137142052945,19.1810189554665,-1.7468948445434E-11));
#14960=CARTESIAN_POINT('Ctrl Pts',(7.27602856538952,19.3560189554666,-4.20081705087651));
#14961=CARTESIAN_POINT('Ctrl Pts',(4.8506857102496,19.5310189554666,-8.40163410173556));
#14962=CARTESIAN_POINT('Ctrl Pts',(-1.5130096486293E-11,19.7060189554665,
-8.40163410172683));
#14963=CARTESIAN_POINT('Ctrl Pts',(-4.85068571027985,19.8810189554666,-8.40163410171809));
#14964=CARTESIAN_POINT('Ctrl Pts',(-7.27602856540465,20.0560189554666,-4.20081705085031));
#14965=CARTESIAN_POINT('Ctrl Pts',(-9.70137142052945,20.2310189554665,1.74701365207797E-11));
#14966=CARTESIAN_POINT('Ctrl Pts',(-7.27602856538952,20.4060189554666,4.20081705087652));
#14967=CARTESIAN_POINT('Ctrl Pts',(-4.8506857102496,20.5810189554666,8.40163410173556));
#14968=CARTESIAN_POINT('Ctrl Pts',(1.5129067582862E-11,20.7560189554665,
8.40163410172683));
#14969=CARTESIAN_POINT('Ctrl Pts',(4.85068571027985,20.9310189554666,8.40163410171809));
#14970=CARTESIAN_POINT('Ctrl Pts',(7.27602856540465,21.1060189554666,4.20081705085031));
#14971=CARTESIAN_POINT('Ctrl Pts',(9.70137142052945,21.2810189554665,-1.7468948445434E-11));
#14972=CARTESIAN_POINT('Ctrl Pts',(7.27602856538952,21.4560189554666,-4.20081705087651));
#14973=CARTESIAN_POINT('Ctrl Pts',(4.8506857102496,21.6310189554666,-8.40163410173556));
#14974=CARTESIAN_POINT('Ctrl Pts',(-1.5130096486293E-11,21.8060189554665,
-8.40163410172683));
#14975=CARTESIAN_POINT('Ctrl Pts',(-4.85068571027985,21.9810189554665,-8.40163410171809));
#14976=CARTESIAN_POINT('Ctrl Pts',(-7.27602856540465,22.1560189554666,-4.20081705085031));
#14977=CARTESIAN_POINT('Ctrl Pts',(-9.70137142052945,22.3310189554665,1.74701365207797E-11));
#14978=CARTESIAN_POINT('Ctrl Pts',(-7.27602856538952,22.5060189554665,4.20081705087652));
#14979=CARTESIAN_POINT('Ctrl Pts',(-4.8506857102496,22.6810189554666,8.40163410173556));
#14980=CARTESIAN_POINT('Ctrl Pts',(1.5129067582862E-11,22.8560189554665,
8.40163410172683));
#14981=CARTESIAN_POINT('Ctrl Pts',(4.85068571027985,23.0310189554665,8.40163410171809));
#14982=CARTESIAN_POINT('Ctrl Pts',(7.27602856540465,23.2060189554666,4.20081705085031));
#14983=CARTESIAN_POINT('Ctrl Pts',(9.70137142052945,23.3810189554665,-1.7468948445434E-11));
#14984=CARTESIAN_POINT('Ctrl Pts',(7.27602856538952,23.5560189554665,-4.20081705087651));
#14985=CARTESIAN_POINT('Ctrl Pts',(4.8506857102496,23.7310189554665,-8.40163410173556));
#14986=CARTESIAN_POINT('Ctrl Pts',(-1.5130096486293E-11,23.9060189554665,
-8.40163410172683));
#14987=CARTESIAN_POINT('Ctrl Pts',(-4.85068571027985,24.0810189554665,-8.40163410171809));
#14988=CARTESIAN_POINT('Ctrl Pts',(-7.27602856540465,24.2560189554665,-4.20081705085031));
#14989=CARTESIAN_POINT('Ctrl Pts',(-9.70137142052945,24.4310189554665,1.74701365207797E-11));
#14990=CARTESIAN_POINT('Ctrl Pts',(-7.27602856538952,24.6060189554665,4.20081705087652));
#14991=CARTESIAN_POINT('Ctrl Pts',(-4.8506857102496,24.7810189554665,8.40163410173556));
#14992=CARTESIAN_POINT('Ctrl Pts',(1.5129067582862E-11,24.9560189554666,
8.40163410172683));
#14993=CARTESIAN_POINT('Ctrl Pts',(4.85068571027985,25.1310189554665,8.40163410171809));
#14994=CARTESIAN_POINT('Ctrl Pts',(7.27602856540465,25.3060189554665,4.20081705085031));
#14995=CARTESIAN_POINT('Ctrl Pts',(9.70137142052945,25.4810189554665,-1.7468948445434E-11));
#14996=CARTESIAN_POINT('Ctrl Pts',(7.27602856538952,25.6560189554665,-4.20081705087651));
#14997=CARTESIAN_POINT('Ctrl Pts',(4.8506857102496,25.8310189554665,-8.40163410173556));
#14998=CARTESIAN_POINT('Ctrl Pts',(-1.5130096486293E-11,26.0060189554665,
-8.40163410172683));
#14999=CARTESIAN_POINT('Ctrl Pts',(8.29083424217445,-24.9756402675196,1.3600098358447));
#15000=CARTESIAN_POINT('Ctrl Pts',(8.77665986763609,-24.8522614613838,-1.60165972355344));
#15001=CARTESIAN_POINT('Ctrl Pts',(7.27603390512277,-24.7439842542419,-4.20082013377283));
#15002=CARTESIAN_POINT('Ctrl Pts',(4.85068927007217,-24.5689842542419,-8.40164026752811));
#15003=CARTESIAN_POINT('Ctrl Pts',(-1.48337207789367E-11,-24.3939842542419,
-8.40164026751963));
#15004=CARTESIAN_POINT('Ctrl Pts',(-4.85068927010184,-24.2189842542419,
-8.40164026751098));
#15005=CARTESIAN_POINT('Ctrl Pts',(-7.27603390513761,-24.0439842542419,
-4.20082013374713));
#15006=CARTESIAN_POINT('Ctrl Pts',(-9.70137854017372,-23.8689842542419,
1.70762120011325E-11));
#15007=CARTESIAN_POINT('Ctrl Pts',(-7.27603390512282,-23.6939842542419,
4.20082013377275));
#15008=CARTESIAN_POINT('Ctrl Pts',(-4.85068927007226,-23.5189842542419,
8.40164026752806));
#15009=CARTESIAN_POINT('Ctrl Pts',(1.47431460078422E-11,-23.3439842542419,
8.40164026751963));
#15010=CARTESIAN_POINT('Ctrl Pts',(4.85068927010175,-23.1689842542419,8.40164026751103));
#15011=CARTESIAN_POINT('Ctrl Pts',(7.2760339051378,-22.9939842542419,4.2008201337468));
#15012=CARTESIAN_POINT('Ctrl Pts',(9.70137854017372,-22.8189842542419,-1.69716252641861E-11));
#15013=CARTESIAN_POINT('Ctrl Pts',(7.27603390512287,-22.6439842542419,-4.20082013377267));
#15014=CARTESIAN_POINT('Ctrl Pts',(4.85068927007187,-22.4689842542419,-8.40164026752828));
#15015=CARTESIAN_POINT('Ctrl Pts',(-1.46525712367478E-11,-22.2939842542419,
-8.40164026751963));
#15016=CARTESIAN_POINT('Ctrl Pts',(-4.85068927010165,-22.1189842542419,
-8.40164026751109));
#15017=CARTESIAN_POINT('Ctrl Pts',(-7.27603390513776,-21.9439842542419,
-4.20082013374688));
#15018=CARTESIAN_POINT('Ctrl Pts',(-9.70137854017372,-21.7689842542419,
1.68670385272398E-11));
#15019=CARTESIAN_POINT('Ctrl Pts',(-7.27603390512291,-21.5939842542419,
4.20082013377259));
#15020=CARTESIAN_POINT('Ctrl Pts',(-4.85068927007196,-21.4189842542419,
8.40164026752823));
#15021=CARTESIAN_POINT('Ctrl Pts',(1.45619964656533E-11,-21.2439842542419,
8.40164026751963));
#15022=CARTESIAN_POINT('Ctrl Pts',(4.85068927010157,-21.0689842542419,8.40164026751114));
#15023=CARTESIAN_POINT('Ctrl Pts',(7.27603390513771,-20.8939842542419,4.20082013374695));
#15024=CARTESIAN_POINT('Ctrl Pts',(9.70137854017372,-20.7189842542419,-1.73139113141798E-11));
#15025=CARTESIAN_POINT('Ctrl Pts',(7.27603390512296,-20.5439842542419,-4.20082013377251));
#15026=CARTESIAN_POINT('Ctrl Pts',(4.85068927007205,-20.3689842542419,-8.40164026752818));
#15027=CARTESIAN_POINT('Ctrl Pts',(-1.49489996514033E-11,-20.1939842542419,
-8.40164026751963));
#15028=CARTESIAN_POINT('Ctrl Pts',(-4.85068927010147,-20.0189842542419,
-8.40164026751119));
#15029=CARTESIAN_POINT('Ctrl Pts',(-7.27603390513767,-19.8439842542419,
-4.20082013374703));
#15030=CARTESIAN_POINT('Ctrl Pts',(-9.70137854017372,-19.6689842542419,
1.72093245772335E-11));
#15031=CARTESIAN_POINT('Ctrl Pts',(-7.276033905123,-19.4939842542419,4.20082013377243));
#15032=CARTESIAN_POINT('Ctrl Pts',(-4.85068927007214,-19.3189842542419,
8.40164026752813));
#15033=CARTESIAN_POINT('Ctrl Pts',(1.48584248803088E-11,-19.1439842542419,
8.40164026751963));
#15034=CARTESIAN_POINT('Ctrl Pts',(4.85068927010186,-18.9689842542419,8.40164026751097));
#15035=CARTESIAN_POINT('Ctrl Pts',(7.27603390513762,-18.7939842542419,4.20082013374711));
#15036=CARTESIAN_POINT('Ctrl Pts',(9.70137854017372,-18.6189842542419,-1.71047378402871E-11));
#15037=CARTESIAN_POINT('Ctrl Pts',(7.27603390512281,-18.4439842542419,-4.20082013377277));
#15038=CARTESIAN_POINT('Ctrl Pts',(4.85068927007223,-18.2689842542419,-8.40164026752807));
#15039=CARTESIAN_POINT('Ctrl Pts',(-1.47678501092144E-11,-18.0939842542419,
-8.40164026751963));
#15040=CARTESIAN_POINT('Ctrl Pts',(-4.85068927010177,-17.9189842542419,
-8.40164026751102));
#15041=CARTESIAN_POINT('Ctrl Pts',(-7.27603390513758,-17.7439842542419,
-4.20082013374719));
#15042=CARTESIAN_POINT('Ctrl Pts',(-9.70137854017372,-17.5689842542419,
1.70001511033408E-11));
#15043=CARTESIAN_POINT('Ctrl Pts',(-7.27603390512285,-17.3939842542419,
4.20082013377269));
#15044=CARTESIAN_POINT('Ctrl Pts',(-4.85068927007185,-17.2189842542419,
8.4016402675283));
#15045=CARTESIAN_POINT('Ctrl Pts',(1.46772753381199E-11,-17.0439842542419,
8.40164026751963));
#15046=CARTESIAN_POINT('Ctrl Pts',(4.85068927010168,-16.8689842542419,8.40164026751107));
#15047=CARTESIAN_POINT('Ctrl Pts',(7.27603390513777,-16.6939842542419,4.20082013374685));
#15048=CARTESIAN_POINT('Ctrl Pts',(9.70137854017372,-16.5189842542419,-1.68955643663944E-11));
#15049=CARTESIAN_POINT('Ctrl Pts',(7.2760339051229,-16.3439842542419,-4.20082013377261));
#15050=CARTESIAN_POINT('Ctrl Pts',(4.85068927007194,-16.1689842542419,-8.40164026752825));
#15051=CARTESIAN_POINT('Ctrl Pts',(-1.45867005670255E-11,-15.9939842542419,
-8.40164026751963));
#15052=CARTESIAN_POINT('Ctrl Pts',(-4.85068927010159,-15.8189842542419,
-8.40164026751112));
#15053=CARTESIAN_POINT('Ctrl Pts',(-7.27603390513773,-15.6439842542419,
-4.20082013374693));
#15054=CARTESIAN_POINT('Ctrl Pts',(-9.70137854017372,-15.4689842542419,
1.67909776294481E-11));
#15055=CARTESIAN_POINT('Ctrl Pts',(-7.27603390512294,-15.2939842542419,
4.20082013377253));
#15056=CARTESIAN_POINT('Ctrl Pts',(-4.85068927007203,-15.1189842542419,
8.40164026752819));
#15057=CARTESIAN_POINT('Ctrl Pts',(1.49737037527755E-11,-14.9439842542419,
8.40164026751963));
#15058=CARTESIAN_POINT('Ctrl Pts',(4.8506892701015,-14.7689842542419,8.40164026751117));
#15059=CARTESIAN_POINT('Ctrl Pts',(7.27603390513768,-14.5939842542419,4.20082013374701));
#15060=CARTESIAN_POINT('Ctrl Pts',(9.70137854017372,-14.4189842542419,-1.72378504163881E-11));
#15061=CARTESIAN_POINT('Ctrl Pts',(7.27603390512299,-14.2439842542419,-4.20082013377245));
#15062=CARTESIAN_POINT('Ctrl Pts',(4.85068927007212,-14.0689842542419,-8.40164026752814));
#15063=CARTESIAN_POINT('Ctrl Pts',(-1.4883128981681E-11,-13.8939842542419,
-8.40164026751963));
#15064=CARTESIAN_POINT('Ctrl Pts',(-4.85068927010141,-13.7189842542419,
-8.40164026751123));
#15065=CARTESIAN_POINT('Ctrl Pts',(-7.27603390513763,-13.5439842542419,
-4.20082013374709));
#15066=CARTESIAN_POINT('Ctrl Pts',(-9.70137854017372,-13.3689842542419,
1.71332636794417E-11));
#15067=CARTESIAN_POINT('Ctrl Pts',(-7.2760339051228,-13.193984254242,4.20082013377279));
#15068=CARTESIAN_POINT('Ctrl Pts',(-4.85068927007221,-13.018984254242,8.40164026752809));
#15069=CARTESIAN_POINT('Ctrl Pts',(1.47925542105866E-11,-12.8439842542419,
8.40164026751963));
#15070=CARTESIAN_POINT('Ctrl Pts',(4.85068927010179,-12.668984254242,8.401640267511));
#15071=CARTESIAN_POINT('Ctrl Pts',(7.27603390513759,-12.4939842542419,4.20082013374717));
#15072=CARTESIAN_POINT('Ctrl Pts',(9.70137854017372,-12.3189842542419,-1.70286769424954E-11));
#15073=CARTESIAN_POINT('Ctrl Pts',(7.27603390512284,-12.143984254242,-4.20082013377271));
#15074=CARTESIAN_POINT('Ctrl Pts',(4.8506892700723,-11.968984254242,-8.40164026752804));
#15075=CARTESIAN_POINT('Ctrl Pts',(-1.47019794394921E-11,-11.7939842542419,
-8.40164026751963));
#15076=CARTESIAN_POINT('Ctrl Pts',(-4.8506892701017,-11.6189842542419,-8.40164026751106));
#15077=CARTESIAN_POINT('Ctrl Pts',(-7.27603390513778,-11.443984254242,-4.20082013374683));
#15078=CARTESIAN_POINT('Ctrl Pts',(-9.70137854017372,-11.2689842542419,
1.69240902055491E-11));
#15079=CARTESIAN_POINT('Ctrl Pts',(-7.27603390512289,-11.0939842542419,
4.20082013377263));
#15080=CARTESIAN_POINT('Ctrl Pts',(-4.85068927007191,-10.918984254242,8.40164026752826));
#15081=CARTESIAN_POINT('Ctrl Pts',(1.46114046683977E-11,-10.7439842542419,
8.40164026751963));
#15082=CARTESIAN_POINT('Ctrl Pts',(4.85068927010161,-10.5689842542419,8.40164026751111));
#15083=CARTESIAN_POINT('Ctrl Pts',(7.27603390513774,-10.393984254242,4.20082013374691));
#15084=CARTESIAN_POINT('Ctrl Pts',(9.70137854017372,-10.2189842542419,-1.68195034686027E-11));
#15085=CARTESIAN_POINT('Ctrl Pts',(7.27603390512293,-10.0439842542419,-4.20082013377256));
#15086=CARTESIAN_POINT('Ctrl Pts',(4.850689270072,-9.86898425424196,-8.40164026752821));
#15087=CARTESIAN_POINT('Ctrl Pts',(-1.49984078541476E-11,-9.69398425424195,
-8.40164026751963));
#15088=CARTESIAN_POINT('Ctrl Pts',(-4.85068927010152,-9.51898425424195,
-8.40164026751116));
#15089=CARTESIAN_POINT('Ctrl Pts',(-7.27603390513769,-9.34398425424196,
-4.20082013374699));
#15090=CARTESIAN_POINT('Ctrl Pts',(-9.70137854017372,-9.16898425424195,
1.72663762555427E-11));
#15091=CARTESIAN_POINT('Ctrl Pts',(-7.27603390512298,-8.99398425424194,
4.20082013377248));
#15092=CARTESIAN_POINT('Ctrl Pts',(-4.85068927007209,-8.81898425424197,
8.40164026752815));
#15093=CARTESIAN_POINT('Ctrl Pts',(1.49078330830532E-11,-8.64398425424195,
8.40164026751963));
#15094=CARTESIAN_POINT('Ctrl Pts',(4.85068927010143,-8.46898425424195,8.40164026751122));
#15095=CARTESIAN_POINT('Ctrl Pts',(7.27603390513765,-8.29398425424196,4.20082013374707));
#15096=CARTESIAN_POINT('Ctrl Pts',(9.70137854017372,-8.11898425424196,-1.71617895185964E-11));
#15097=CARTESIAN_POINT('Ctrl Pts',(7.27603390512302,-7.94398425424195,-4.2008201337724));
#15098=CARTESIAN_POINT('Ctrl Pts',(4.85068927007219,-7.76898425424197,-8.4016402675281));
#15099=CARTESIAN_POINT('Ctrl Pts',(-1.48172583119587E-11,-7.59398425424196,
-8.40164026751963));
#15100=CARTESIAN_POINT('Ctrl Pts',(-4.85068927010182,-7.41898425424196,
-8.40164026751099));
#15101=CARTESIAN_POINT('Ctrl Pts',(-7.2760339051376,-7.24398425424194,-4.20082013374715));
#15102=CARTESIAN_POINT('Ctrl Pts',(-9.70137854017372,-7.06898425424196,
1.705720278165E-11));
#15103=CARTESIAN_POINT('Ctrl Pts',(-7.27603390512283,-6.89398425424195,
4.20082013377273));
#15104=CARTESIAN_POINT('Ctrl Pts',(-4.85068927007227,-6.71898425424195,
8.40164026752805));
#15105=CARTESIAN_POINT('Ctrl Pts',(1.47266835408643E-11,-6.54398425424196,
8.40164026751963));
#15106=CARTESIAN_POINT('Ctrl Pts',(4.85068927010173,-6.36898425424197,8.40164026751104));
#15107=CARTESIAN_POINT('Ctrl Pts',(7.27603390513756,-6.19398425424195,4.20082013374722));
#15108=CARTESIAN_POINT('Ctrl Pts',(9.70137854017372,-6.01898425424197,-1.69526160447037E-11));
#15109=CARTESIAN_POINT('Ctrl Pts',(7.27603390512287,-5.84398425424196,-4.20082013377265));
#15110=CARTESIAN_POINT('Ctrl Pts',(4.85068927007189,-5.66898425424195,-8.40164026752827));
#15111=CARTESIAN_POINT('Ctrl Pts',(-1.46361087697698E-11,-5.49398425424197,
-8.40164026751963));
#15112=CARTESIAN_POINT('Ctrl Pts',(-4.85068927010164,-5.31898425424197,
-8.40164026751109));
#15113=CARTESIAN_POINT('Ctrl Pts',(-7.27603390513775,-5.14398425424195,
-4.20082013374689));
#15114=CARTESIAN_POINT('Ctrl Pts',(-9.70137854017372,-4.96898425424197,
1.68480293077573E-11));
#15115=CARTESIAN_POINT('Ctrl Pts',(-7.27603390512292,-4.79398425424196,
4.20082013377258));
#15116=CARTESIAN_POINT('Ctrl Pts',(-4.85068927007198,-4.61898425424196,
8.40164026752822));
#15117=CARTESIAN_POINT('Ctrl Pts',(1.45455339986754E-11,-4.44398425424197,
8.40164026751963));
#15118=CARTESIAN_POINT('Ctrl Pts',(4.85068927010155,-4.26898425424197,8.40164026751115));
#15119=CARTESIAN_POINT('Ctrl Pts',(7.2760339051377,-4.09398425424196,4.20082013374697));
#15120=CARTESIAN_POINT('Ctrl Pts',(9.70137854017372,-3.91898425424198,-1.72949020946973E-11));
#15121=CARTESIAN_POINT('Ctrl Pts',(7.27603390512296,-3.74398425424197,-4.2008201337725));
#15122=CARTESIAN_POINT('Ctrl Pts',(4.85068927007207,-3.56898425424196,-8.40164026752817));
#15123=CARTESIAN_POINT('Ctrl Pts',(-1.49325371844254E-11,-3.39398425424198,
-8.40164026751963));
#15124=CARTESIAN_POINT('Ctrl Pts',(-4.85068927010146,-3.21898425424198,
-8.4016402675112));
#15125=CARTESIAN_POINT('Ctrl Pts',(-7.27603390513766,-3.04398425424196,
-4.20082013374705));
#15126=CARTESIAN_POINT('Ctrl Pts',(-9.70137854017372,-2.86898425424196,
1.7190315357751E-11));
#15127=CARTESIAN_POINT('Ctrl Pts',(-7.27603390512301,-2.69398425424197,
4.20082013377242));
#15128=CARTESIAN_POINT('Ctrl Pts',(-4.85068927007216,-2.51898425424197,
8.40164026752812));
#15129=CARTESIAN_POINT('Ctrl Pts',(1.48419624133309E-11,-2.34398425424195,
8.40164026751963));
#15130=CARTESIAN_POINT('Ctrl Pts',(4.85068927010137,-2.16898425424197,8.40164026751125));
#15131=CARTESIAN_POINT('Ctrl Pts',(7.27603390513761,-1.99398425424197,4.20082013374713));
#15132=CARTESIAN_POINT('Ctrl Pts',(9.70137854017372,-1.81898425424196,-1.70857286208046E-11));
#15133=CARTESIAN_POINT('Ctrl Pts',(7.27603390512282,-1.64398425424198,-4.20082013377275));
#15134=CARTESIAN_POINT('Ctrl Pts',(4.85068927007225,-1.46898425424197,-8.40164026752806));
#15135=CARTESIAN_POINT('Ctrl Pts',(-1.47513876422365E-11,-1.29398425424196,
-8.40164026751963));
#15136=CARTESIAN_POINT('Ctrl Pts',(-4.85068927010175,-1.11898425424198,
-8.40164026751103));
#15137=CARTESIAN_POINT('Ctrl Pts',(-7.27603390513757,-0.94398425424197,
-4.2008201337472));
#15138=CARTESIAN_POINT('Ctrl Pts',(-9.70137854017372,-0.768984254241965,
1.69811418838583E-11));
#15139=CARTESIAN_POINT('Ctrl Pts',(-7.27603390512286,-0.59398425424198,
4.20082013377267));
#15140=CARTESIAN_POINT('Ctrl Pts',(-4.85068927007234,-0.418984254241974,
8.40164026752801));
#15141=CARTESIAN_POINT('Ctrl Pts',(1.4660812871142E-11,-0.243984254241963,
8.40164026751963));
#15142=CARTESIAN_POINT('Ctrl Pts',(4.85068927010166,-0.068984254241984,
8.40164026751108));
#15143=CARTESIAN_POINT('Ctrl Pts',(7.27603390513776,0.106015745758026,4.20082013374687));
#15144=CARTESIAN_POINT('Ctrl Pts',(9.70137854017372,0.28101574575803,-1.6876555146912E-11));
#15145=CARTESIAN_POINT('Ctrl Pts',(7.27603390512291,0.456015745758015,-4.2008201337726));
#15146=CARTESIAN_POINT('Ctrl Pts',(4.85068927007195,0.631015745758021,-8.40164026752823));
#15147=CARTESIAN_POINT('Ctrl Pts',(-1.45702381000475E-11,0.806015745758032,
-8.40164026751963));
#15148=CARTESIAN_POINT('Ctrl Pts',(-4.85068927010157,0.981015745758011,
-8.40164026751113));
#15149=CARTESIAN_POINT('Ctrl Pts',(-7.27603390513772,1.15601574575802,-4.20082013374695));
#15150=CARTESIAN_POINT('Ctrl Pts',(-9.70137854017372,1.33101574575803,1.67719684099656E-11));
#15151=CARTESIAN_POINT('Ctrl Pts',(-7.27603390512295,1.50601574575804,4.20082013377252));
#15152=CARTESIAN_POINT('Ctrl Pts',(-4.85068927007204,1.68101574575802,8.40164026752818));
#15153=CARTESIAN_POINT('Ctrl Pts',(1.49572412857975E-11,1.85601574575803,
8.40164026751963));
#15154=CARTESIAN_POINT('Ctrl Pts',(4.85068927010148,2.03101574575803,8.40164026751119));
#15155=CARTESIAN_POINT('Ctrl Pts',(7.27603390513767,2.20601574575802,4.20082013374703));
#15156=CARTESIAN_POINT('Ctrl Pts',(9.70137854017372,2.38101574575802,-1.72188411969056E-11));
#15157=CARTESIAN_POINT('Ctrl Pts',(7.276033905123,2.55601574575803,-4.20082013377244));
#15158=CARTESIAN_POINT('Ctrl Pts',(4.85068927007213,2.73101574575801,-8.40164026752813));
#15159=CARTESIAN_POINT('Ctrl Pts',(-1.48666665147031E-11,2.90601574575802,
-8.40164026751963));
#15160=CARTESIAN_POINT('Ctrl Pts',(-4.85068927010139,3.08101574575803,-8.40164026751124));
#15161=CARTESIAN_POINT('Ctrl Pts',(-7.27603390513763,3.25601574575801,-4.2008201337471));
#15162=CARTESIAN_POINT('Ctrl Pts',(-9.70137854017372,3.43101574575802,1.71142544599593E-11));
#15163=CARTESIAN_POINT('Ctrl Pts',(-7.27603390512304,3.60601574575803,4.20082013377236));
#15164=CARTESIAN_POINT('Ctrl Pts',(-4.85068927007222,3.78101574575801,8.40164026752808));
#15165=CARTESIAN_POINT('Ctrl Pts',(1.47760917436086E-11,3.95601574575802,
8.40164026751963));
#15166=CARTESIAN_POINT('Ctrl Pts',(4.85068927010178,4.13101574575802,8.40164026751101));
#15167=CARTESIAN_POINT('Ctrl Pts',(7.27603390513758,4.30601574575801,4.20082013374718));
#15168=CARTESIAN_POINT('Ctrl Pts',(9.70137854017372,4.48101574575801,-1.70096677230129E-11));
#15169=CARTESIAN_POINT('Ctrl Pts',(7.27603390512285,4.65601574575802,-4.2008201337727));
#15170=CARTESIAN_POINT('Ctrl Pts',(4.85068927007232,4.831015745758,-8.40164026752803));
#15171=CARTESIAN_POINT('Ctrl Pts',(-1.46855169725142E-11,5.00601574575801,
-8.40164026751963));
#15172=CARTESIAN_POINT('Ctrl Pts',(-4.85068927010169,5.18101574575802,-8.40164026751107));
#15173=CARTESIAN_POINT('Ctrl Pts',(-7.27603390513754,5.356015745758,-4.20082013374726));
#15174=CARTESIAN_POINT('Ctrl Pts',(-9.70137854017372,5.53101574575801,1.69050809860666E-11));
#15175=CARTESIAN_POINT('Ctrl Pts',(-7.27603390512289,5.70601574575802,4.20082013377262));
#15176=CARTESIAN_POINT('Ctrl Pts',(-4.85068927007193,5.881015745758,8.40164026752825));
#15177=CARTESIAN_POINT('Ctrl Pts',(1.45949422014197E-11,6.05601574575801,
8.40164026751963));
#15178=CARTESIAN_POINT('Ctrl Pts',(4.8506892701016,6.23101574575801,8.40164026751112));
#15179=CARTESIAN_POINT('Ctrl Pts',(7.27603390513773,6.40601574575803,4.20082013374692));
#15180=CARTESIAN_POINT('Ctrl Pts',(9.70137854017372,6.581015745758,-1.68004942491202E-11));
#15181=CARTESIAN_POINT('Ctrl Pts',(7.27603390512294,6.75601574575802,-4.20082013377254));
#15182=CARTESIAN_POINT('Ctrl Pts',(4.85068927007202,6.93101574575802,-8.4016402675282));
#15183=CARTESIAN_POINT('Ctrl Pts',(-1.45043674303253E-11,7.106015745758,
-8.40164026751963));
#15184=CARTESIAN_POINT('Ctrl Pts',(-4.85068927010151,7.28101574575801,-8.40164026751117));
#15185=CARTESIAN_POINT('Ctrl Pts',(-7.27603390513768,7.45601574575802,-4.200820133747));
#15186=CARTESIAN_POINT('Ctrl Pts',(-9.70137854017372,7.631015745758,1.72473670360602E-11));
#15187=CARTESIAN_POINT('Ctrl Pts',(-7.27603390512298,7.80601574575801,4.20082013377246));
#15188=CARTESIAN_POINT('Ctrl Pts',(-4.85068927007211,7.98101574575801,8.40164026752814));
#15189=CARTESIAN_POINT('Ctrl Pts',(1.48913706160753E-11,8.156015745758,
8.40164026751963));
#15190=CARTESIAN_POINT('Ctrl Pts',(4.85068927010141,8.331015745758,8.40164026751122));
#15191=CARTESIAN_POINT('Ctrl Pts',(7.27603390513764,8.50601574575802,4.20082013374708));
#15192=CARTESIAN_POINT('Ctrl Pts',(9.70137854017372,8.68101574575799,-1.71427802991139E-11));
#15193=CARTESIAN_POINT('Ctrl Pts',(7.27603390512303,8.85601574575801,-4.20082013377238));
#15194=CARTESIAN_POINT('Ctrl Pts',(4.8506892700722,9.03101574575801,-8.40164026752809));
#15195=CARTESIAN_POINT('Ctrl Pts',(-1.48007958449808E-11,9.20601574575799,
-8.40164026751963));
#15196=CARTESIAN_POINT('Ctrl Pts',(-4.8506892701018,9.381015745758,-8.401640267511));
#15197=CARTESIAN_POINT('Ctrl Pts',(-7.27603390513759,9.55601574575801,-4.20082013374716));
#15198=CARTESIAN_POINT('Ctrl Pts',(-9.70137854017372,9.73101574575799,1.70381935621676E-11));
#15199=CARTESIAN_POINT('Ctrl Pts',(-7.27603390512284,9.906015745758,4.20082013377272));
#15200=CARTESIAN_POINT('Ctrl Pts',(-4.85068927007229,10.081015745758,8.40164026752804));
#15201=CARTESIAN_POINT('Ctrl Pts',(1.47102210738864E-11,10.256015745758,
8.40164026751963));
#15202=CARTESIAN_POINT('Ctrl Pts',(4.85068927010171,10.431015745758,8.40164026751105));
#15203=CARTESIAN_POINT('Ctrl Pts',(7.27603390513755,10.606015745758,4.20082013374724));
#15204=CARTESIAN_POINT('Ctrl Pts',(9.70137854017372,10.781015745758,-1.69336068252212E-11));
#15205=CARTESIAN_POINT('Ctrl Pts',(7.27603390512288,10.956015745758,-4.20082013377264));
#15206=CARTESIAN_POINT('Ctrl Pts',(4.85068927007238,11.131015745758,-8.40164026752799));
#15207=CARTESIAN_POINT('Ctrl Pts',(-1.46196463027919E-11,11.306015745758,
-8.40164026751963));
#15208=CARTESIAN_POINT('Ctrl Pts',(-4.85068927010162,11.481015745758,-8.40164026751111));
#15209=CARTESIAN_POINT('Ctrl Pts',(-7.27603390513774,11.656015745758,-4.2008201337469));
#15210=CARTESIAN_POINT('Ctrl Pts',(-9.70137854017372,11.831015745758,1.68290200882749E-11));
#15211=CARTESIAN_POINT('Ctrl Pts',(-7.27603390512293,12.006015745758,4.20082013377256));
#15212=CARTESIAN_POINT('Ctrl Pts',(-4.85068927007199,12.181015745758,8.40164026752821));
#15213=CARTESIAN_POINT('Ctrl Pts',(1.45290715316974E-11,12.356015745758,
8.40164026751963));
#15214=CARTESIAN_POINT('Ctrl Pts',(4.85068927010153,12.531015745758,8.40164026751116));
#15215=CARTESIAN_POINT('Ctrl Pts',(7.2760339051377,12.706015745758,4.20082013374698));
#15216=CARTESIAN_POINT('Ctrl Pts',(9.70137854017372,12.881015745758,-1.67244333513285E-11));
#15217=CARTESIAN_POINT('Ctrl Pts',(7.27603390512297,13.056015745758,-4.20082013377248));
#15218=CARTESIAN_POINT('Ctrl Pts',(4.85068927007208,13.231015745758,-8.40164026752816));
#15219=CARTESIAN_POINT('Ctrl Pts',(-1.49160747174474E-11,13.406015745758,
-8.40164026751963));
#15220=CARTESIAN_POINT('Ctrl Pts',(-4.85068927010144,13.581015745758,-8.40164026751121));
#15221=CARTESIAN_POINT('Ctrl Pts',(-7.27603390513765,13.756015745758,-4.20082013374706));
#15222=CARTESIAN_POINT('Ctrl Pts',(-9.70137854017372,13.931015745758,1.71713061382685E-11));
#15223=CARTESIAN_POINT('Ctrl Pts',(-7.27603390512302,14.106015745758,4.2008201337724));
#15224=CARTESIAN_POINT('Ctrl Pts',(-4.85068927007218,14.281015745758,8.40164026752811));
#15225=CARTESIAN_POINT('Ctrl Pts',(1.4825499946353E-11,14.456015745758,
8.40164026751963));
#15226=CARTESIAN_POINT('Ctrl Pts',(4.85068927010135,14.631015745758,8.40164026751126));
#15227=CARTESIAN_POINT('Ctrl Pts',(7.27603390513761,14.806015745758,4.20082013374714));
#15228=CARTESIAN_POINT('Ctrl Pts',(9.70137854017372,14.981015745758,-1.70667194013222E-11));
#15229=CARTESIAN_POINT('Ctrl Pts',(7.27603390512282,15.156015745758,-4.20082013377274));
#15230=CARTESIAN_POINT('Ctrl Pts',(4.85068927007227,15.331015745758,-8.40164026752806));
#15231=CARTESIAN_POINT('Ctrl Pts',(-1.47349251752585E-11,15.506015745758,
-8.40164026751963));
#15232=CARTESIAN_POINT('Ctrl Pts',(-4.85068927010174,15.681015745758,-8.40164026751104));
#15233=CARTESIAN_POINT('Ctrl Pts',(-7.27603390513756,15.856015745758,-4.20082013374722));
#15234=CARTESIAN_POINT('Ctrl Pts',(-9.70137854017372,16.031015745758,1.69621326643758E-11));
#15235=CARTESIAN_POINT('Ctrl Pts',(-7.27603390512287,16.206015745758,4.20082013377266));
#15236=CARTESIAN_POINT('Ctrl Pts',(-4.85068927007236,16.381015745758,8.401640267528));
#15237=CARTESIAN_POINT('Ctrl Pts',(1.46443504041641E-11,16.556015745758,
8.40164026751963));
#15238=CARTESIAN_POINT('Ctrl Pts',(4.85068927010165,16.731015745758,8.40164026751109));
#15239=CARTESIAN_POINT('Ctrl Pts',(7.27603390513752,16.906015745758,4.2008201337473));
#15240=CARTESIAN_POINT('Ctrl Pts',(9.70137854017372,17.081015745758,-1.68575459274295E-11));
#15241=CARTESIAN_POINT('Ctrl Pts',(7.27603390512292,17.256015745758,-4.20082013377258));
#15242=CARTESIAN_POINT('Ctrl Pts',(4.85068927007197,17.431015745758,-8.40164026752823));
#15243=CARTESIAN_POINT('Ctrl Pts',(-1.45537756330696E-11,17.606015745758,
-8.40164026751963));
#15244=CARTESIAN_POINT('Ctrl Pts',(-4.85068927010155,17.781015745758,-8.40164026751114));
#15245=CARTESIAN_POINT('Ctrl Pts',(-7.27603390513771,17.956015745758,-4.20082013374696));
#15246=CARTESIAN_POINT('Ctrl Pts',(-9.70137854017372,18.131015745758,1.67529591904832E-11));
#15247=CARTESIAN_POINT('Ctrl Pts',(-7.27603390512296,18.306015745758,4.2008201337725));
#15248=CARTESIAN_POINT('Ctrl Pts',(-4.85068927007206,18.481015745758,8.40164026752817));
#15249=CARTESIAN_POINT('Ctrl Pts',(1.44632008619752E-11,18.656015745758,
8.40164026751963));
#15250=CARTESIAN_POINT('Ctrl Pts',(4.85068927010146,18.831015745758,8.4016402675112));
#15251=CARTESIAN_POINT('Ctrl Pts',(7.27603390513766,19.006015745758,4.20082013374704));
#15252=CARTESIAN_POINT('Ctrl Pts',(9.70137854017372,19.181015745758,-1.71998319774232E-11));
#15253=CARTESIAN_POINT('Ctrl Pts',(7.27603390512301,19.356015745758,-4.20082013377243));
#15254=CARTESIAN_POINT('Ctrl Pts',(4.85068927007215,19.531015745758,-8.40164026752812));
#15255=CARTESIAN_POINT('Ctrl Pts',(-1.48502040477252E-11,19.706015745758,
-8.40164026751963));
#15256=CARTESIAN_POINT('Ctrl Pts',(-4.85068927010137,19.881015745758,-8.40164026751125));
#15257=CARTESIAN_POINT('Ctrl Pts',(-7.27603390513762,20.056015745758,-4.20082013374712));
#15258=CARTESIAN_POINT('Ctrl Pts',(-9.70137854017372,20.231015745758,1.70952452404768E-11));
#15259=CARTESIAN_POINT('Ctrl Pts',(-7.27603390512305,20.406015745758,4.20082013377235));
#15260=CARTESIAN_POINT('Ctrl Pts',(-4.85068927007224,20.581015745758,8.40164026752807));
#15261=CARTESIAN_POINT('Ctrl Pts',(1.47596292766307E-11,20.756015745758,
8.40164026751963));
#15262=CARTESIAN_POINT('Ctrl Pts',(4.85068927010176,20.931015745758,8.40164026751102));
#15263=CARTESIAN_POINT('Ctrl Pts',(7.27603390513757,21.106015745758,4.2008201337472));
#15264=CARTESIAN_POINT('Ctrl Pts',(9.70137854017372,21.281015745758,-1.69906585035305E-11));
#15265=CARTESIAN_POINT('Ctrl Pts',(7.27603390512286,21.456015745758,-4.20082013377268));
#15266=CARTESIAN_POINT('Ctrl Pts',(4.85068927007233,21.631015745758,-8.40164026752802));
#15267=CARTESIAN_POINT('Ctrl Pts',(-1.46690545055362E-11,21.806015745758,
-8.40164026751963));
#15268=CARTESIAN_POINT('Ctrl Pts',(-4.85068927010167,21.981015745758,-8.40164026751108));
#15269=CARTESIAN_POINT('Ctrl Pts',(-7.27603390513753,22.156015745758,-4.20082013374728));
#15270=CARTESIAN_POINT('Ctrl Pts',(-7.69929559114725,22.1865560631964,-3.46770938867822));
#15271=CARTESIAN_POINT('Ctrl Pts',(-7.96780251527898,22.22,-2.66489817109789));
#15272=CARTESIAN_POINT('Ctrl Pts',(5.8718173029053,-25.4,-8.00113003034161));
#15273=CARTESIAN_POINT('Ctrl Pts',(3.25092800548582,-25.2860389439906,-9.92453123332517));
#15274=CARTESIAN_POINT('Ctrl Pts',(-1.76294905048704E-11,-25.1867511126202,
-9.92453123331945));
#15275=CARTESIAN_POINT('Ctrl Pts',(-5.72993077915507,-25.0117511126202,
-9.9245312333095));
#15276=CARTESIAN_POINT('Ctrl Pts',(-8.59489616871545,-24.8367511126202,
-4.96226561664465));
#15277=CARTESIAN_POINT('Ctrl Pts',(-11.4598615582757,-24.6617511126202,
2.02950100528141E-11));
#15278=CARTESIAN_POINT('Ctrl Pts',(-8.59489616869816,-24.4867511126202,
4.9622656166746));
#15279=CARTESIAN_POINT('Ctrl Pts',(-5.72993077912048,-24.3117511126203,
9.92453123332946));
#15280=CARTESIAN_POINT('Ctrl Pts',(1.75224980467247E-11,-24.1367511126202,
9.92453123331945));
#15281=CARTESIAN_POINT('Ctrl Pts',(5.72993077915496,-23.9617511126202,9.92453123330956));
#15282=CARTESIAN_POINT('Ctrl Pts',(8.5948961687154,-23.7867511126202,4.96226561664474));
#15283=CARTESIAN_POINT('Ctrl Pts',(11.4598615582757,-23.6117511126202,-2.01714658037908E-11));
#15284=CARTESIAN_POINT('Ctrl Pts',(8.59489616869793,-23.4367511126202,-4.962265616675));
#15285=CARTESIAN_POINT('Ctrl Pts',(5.72993077912059,-23.2617511126202,-9.9245312333294));
#15286=CARTESIAN_POINT('Ctrl Pts',(-1.74155055885791E-11,-23.0867511126202,
-9.92453123331945));
#15287=CARTESIAN_POINT('Ctrl Pts',(-5.72993077915542,-22.9117511126202,
-9.92453123330929));
#15288=CARTESIAN_POINT('Ctrl Pts',(-8.59489616871534,-22.7367511126202,
-4.96226561664484));
#15289=CARTESIAN_POINT('Ctrl Pts',(-11.4598615582757,-22.5617511126202,
2.00479215547674E-11));
#15290=CARTESIAN_POINT('Ctrl Pts',(-8.59489616869798,-22.3867511126202,
4.96226561667491));
#15291=CARTESIAN_POINT('Ctrl Pts',(-5.72993077912069,-22.2117511126202,
9.92453123332934));
#15292=CARTESIAN_POINT('Ctrl Pts',(1.73085131304334E-11,-22.0367511126202,
9.92453123331945));
#15293=CARTESIAN_POINT('Ctrl Pts',(5.72993077915531,-21.8617511126203,9.92453123330936));
#15294=CARTESIAN_POINT('Ctrl Pts',(8.59489616871557,-21.6867511126202,4.96226561664444));
#15295=CARTESIAN_POINT('Ctrl Pts',(11.4598615582757,-21.5117511126203,-1.99243773057441E-11));
#15296=CARTESIAN_POINT('Ctrl Pts',(8.59489616869803,-21.3367511126203,-4.96226561667481));
#15297=CARTESIAN_POINT('Ctrl Pts',(5.72993077912024,-21.1617511126202,-9.92453123332961));
#15298=CARTESIAN_POINT('Ctrl Pts',(-1.72015206722877E-11,-20.9867511126202,
-9.92453123331945));
#15299=CARTESIAN_POINT('Ctrl Pts',(-5.7299307791552,-20.8117511126203,-9.92453123330942));
#15300=CARTESIAN_POINT('Ctrl Pts',(-8.59489616871552,-20.6367511126202,
-4.96226561664453));
#15301=CARTESIAN_POINT('Ctrl Pts',(-11.4598615582757,-20.4617511126203,
1.98008330567208E-11));
#15302=CARTESIAN_POINT('Ctrl Pts',(-8.59489616869809,-20.2867511126202,
4.96226561667472));
#15303=CARTESIAN_POINT('Ctrl Pts',(-5.72993077912034,-20.1117511126202,
9.92453123332955));
#15304=CARTESIAN_POINT('Ctrl Pts',(1.7094528214142E-11,-19.9367511126203,
9.92453123331945));
#15305=CARTESIAN_POINT('Ctrl Pts',(5.7299307791551,-19.7617511126202,9.92453123330948));
#15306=CARTESIAN_POINT('Ctrl Pts',(8.59489616871547,-19.5867511126202,4.96226561664462));
#15307=CARTESIAN_POINT('Ctrl Pts',(11.4598615582757,-19.4117511126203,-2.03287065183413E-11));
#15308=CARTESIAN_POINT('Ctrl Pts',(8.59489616869814,-19.2367511126202,-4.96226561667463));
#15309=CARTESIAN_POINT('Ctrl Pts',(5.72993077912045,-19.0617511126202,-9.92453123332948));
#15310=CARTESIAN_POINT('Ctrl Pts',(-1.75516800418891E-11,-18.8867511126203,
-9.92453123331945));
#15311=CARTESIAN_POINT('Ctrl Pts',(-5.72993077915499,-18.7117511126202,
-9.92453123330954));
#15312=CARTESIAN_POINT('Ctrl Pts',(-8.59489616871541,-18.5367511126203,
-4.96226561664472));
#15313=CARTESIAN_POINT('Ctrl Pts',(-11.4598615582757,-18.3617511126203,
2.0205162269318E-11));
#15314=CARTESIAN_POINT('Ctrl Pts',(-8.5948961686982,-18.1867511126202,4.96226561667454));
#15315=CARTESIAN_POINT('Ctrl Pts',(-5.72993077912056,-18.0117511126203,
9.92453123332942));
#15316=CARTESIAN_POINT('Ctrl Pts',(1.74446875837434E-11,-17.8367511126202,
9.92453123331945));
#15317=CARTESIAN_POINT('Ctrl Pts',(5.72993077915545,-17.6617511126203,9.92453123330928));
#15318=CARTESIAN_POINT('Ctrl Pts',(8.59489616871536,-17.4867511126202,4.96226561664481));
#15319=CARTESIAN_POINT('Ctrl Pts',(11.4598615582757,-17.3117511126203,-2.00816180202947E-11));
#15320=CARTESIAN_POINT('Ctrl Pts',(8.59489616869797,-17.1367511126203,-4.96226561667493));
#15321=CARTESIAN_POINT('Ctrl Pts',(5.72993077912066,-16.9617511126202,-9.92453123332936));
#15322=CARTESIAN_POINT('Ctrl Pts',(-1.73376951255977E-11,-16.7867511126203,
-9.92453123331945));
#15323=CARTESIAN_POINT('Ctrl Pts',(-5.72993077915534,-16.6117511126203,
-9.92453123330934));
#15324=CARTESIAN_POINT('Ctrl Pts',(-8.59489616871531,-16.4367511126202,
-4.9622656166449));
#15325=CARTESIAN_POINT('Ctrl Pts',(-11.4598615582757,-16.2617511126203,
1.99580737712713E-11));
#15326=CARTESIAN_POINT('Ctrl Pts',(-8.59489616869802,-16.0867511126203,
4.96226561667484));
#15327=CARTESIAN_POINT('Ctrl Pts',(-5.72993077912021,-15.9117511126202,
9.92453123332962));
#15328=CARTESIAN_POINT('Ctrl Pts',(1.7230702667452E-11,-15.7367511126203,
9.92453123331945));
#15329=CARTESIAN_POINT('Ctrl Pts',(5.72993077915523,-15.5617511126203,9.9245312333094));
#15330=CARTESIAN_POINT('Ctrl Pts',(8.59489616871553,-15.3867511126203,4.96226561664451));
#15331=CARTESIAN_POINT('Ctrl Pts',(11.4598615582757,-15.2117511126203,-1.9834529522248E-11));
#15332=CARTESIAN_POINT('Ctrl Pts',(8.59489616869807,-15.0367511126203,-4.96226561667475));
#15333=CARTESIAN_POINT('Ctrl Pts',(5.72993077912031,-14.8617511126203,-9.92453123332956));
#15334=CARTESIAN_POINT('Ctrl Pts',(-1.71237102093063E-11,-14.6867511126202,
-9.92453123331945));
#15335=CARTESIAN_POINT('Ctrl Pts',(-5.72993077915512,-14.5117511126203,
-9.92453123330946));
#15336=CARTESIAN_POINT('Ctrl Pts',(-8.59489616871548,-14.3367511126203,
-4.9622656166446));
#15337=CARTESIAN_POINT('Ctrl Pts',(-11.4598615582757,-14.1617511126203,
1.97109852732247E-11));
#15338=CARTESIAN_POINT('Ctrl Pts',(-8.59489616869813,-13.9867511126203,
4.96226561667465));
#15339=CARTESIAN_POINT('Ctrl Pts',(-5.72993077912042,-13.8117511126203,
9.9245312333295));
#15340=CARTESIAN_POINT('Ctrl Pts',(1.75808620370534E-11,-13.6367511126203,
9.92453123331945));
#15341=CARTESIAN_POINT('Ctrl Pts',(5.72993077915502,-13.4617511126203,9.92453123330952));
#15342=CARTESIAN_POINT('Ctrl Pts',(8.59489616871543,-13.2867511126203,4.96226561664469));
#15343=CARTESIAN_POINT('Ctrl Pts',(11.4598615582757,-13.1117511126203,-2.02388587348453E-11));
#15344=CARTESIAN_POINT('Ctrl Pts',(8.59489616869818,-12.9367511126203,-4.96226561667456));
#15345=CARTESIAN_POINT('Ctrl Pts',(5.72993077912053,-12.7617511126203,-9.92453123332944));
#15346=CARTESIAN_POINT('Ctrl Pts',(-1.74738695789077E-11,-12.5867511126203,
-9.92453123331945));
#15347=CARTESIAN_POINT('Ctrl Pts',(-5.72993077915491,-12.4117511126203,
-9.92453123330959));
#15348=CARTESIAN_POINT('Ctrl Pts',(-8.59489616871537,-12.2367511126203,
-4.96226561664478));
#15349=CARTESIAN_POINT('Ctrl Pts',(-11.4598615582757,-12.0617511126203,
2.01153144858219E-11));
#15350=CARTESIAN_POINT('Ctrl Pts',(-8.59489616869795,-11.8867511126203,
4.96226561667496));
#15351=CARTESIAN_POINT('Ctrl Pts',(-5.72993077912063,-11.7117511126203,
9.92453123332938));
#15352=CARTESIAN_POINT('Ctrl Pts',(1.7366877120762E-11,-11.5367511126203,
9.92453123331945));
#15353=CARTESIAN_POINT('Ctrl Pts',(5.72993077915537,-11.3617511126203,9.92453123330932));
#15354=CARTESIAN_POINT('Ctrl Pts',(8.59489616871532,-11.1867511126203,4.96226561664488));
#15355=CARTESIAN_POINT('Ctrl Pts',(11.4598615582757,-11.0117511126203,-1.99917702367986E-11));
#15356=CARTESIAN_POINT('Ctrl Pts',(8.59489616869801,-10.8367511126203,-4.96226561667487));
#15357=CARTESIAN_POINT('Ctrl Pts',(5.72993077912074,-10.6617511126203,-9.92453123332931));
#15358=CARTESIAN_POINT('Ctrl Pts',(-1.72598846626164E-11,-10.4867511126203,
-9.92453123331945));
#15359=CARTESIAN_POINT('Ctrl Pts',(-5.72993077915526,-10.3117511126203,
-9.92453123330938));
#15360=CARTESIAN_POINT('Ctrl Pts',(-8.59489616871555,-10.1367511126203,
-4.96226561664448));
#15361=CARTESIAN_POINT('Ctrl Pts',(-11.4598615582757,-9.96175111262027,
1.98682259877752E-11));
#15362=CARTESIAN_POINT('Ctrl Pts',(-8.59489616869806,-9.78675111262026,
4.96226561667477));
#15363=CARTESIAN_POINT('Ctrl Pts',(-5.72993077912029,-9.61175111262028,
9.92453123332958));
#15364=CARTESIAN_POINT('Ctrl Pts',(1.71528922044707E-11,-9.43675111262027,
9.92453123331945));
#15365=CARTESIAN_POINT('Ctrl Pts',(5.72993077915515,-9.26175111262026,9.92453123330944));
#15366=CARTESIAN_POINT('Ctrl Pts',(8.59489616871549,-9.08675111262028,4.96226561664457));
#15367=CARTESIAN_POINT('Ctrl Pts',(11.4598615582757,-8.91175111262028,-1.97446817387519E-11));
#15368=CARTESIAN_POINT('Ctrl Pts',(8.59489616869811,-8.73675111262026,-4.96226561667468));
#15369=CARTESIAN_POINT('Ctrl Pts',(5.72993077912039,-8.56175111262028,-9.92453123332952));
#15370=CARTESIAN_POINT('Ctrl Pts',(-1.76100440322177E-11,-8.38675111262027,
-9.92453123331945));
#15371=CARTESIAN_POINT('Ctrl Pts',(-5.72993077915505,-8.21175111262026,
-9.92453123330951));
#15372=CARTESIAN_POINT('Ctrl Pts',(-8.59489616871544,-8.03675111262028,
-4.96226561664467));
#15373=CARTESIAN_POINT('Ctrl Pts',(-11.4598615582757,-7.86175111262028,
2.02725552003725E-11));
#15374=CARTESIAN_POINT('Ctrl Pts',(-8.59489616869817,-7.68675111262027,
4.96226561667459));
#15375=CARTESIAN_POINT('Ctrl Pts',(-5.7299307791205,-7.51175111262028,9.92453123332946));
#15376=CARTESIAN_POINT('Ctrl Pts',(1.75030515740721E-11,-7.33675111262028,
9.92453123331945));
#15377=CARTESIAN_POINT('Ctrl Pts',(5.72993077915494,-7.16175111262027,9.92453123330957));
#15378=CARTESIAN_POINT('Ctrl Pts',(8.59489616871539,-6.98675111262029,4.96226561664476));
#15379=CARTESIAN_POINT('Ctrl Pts',(11.4598615582757,-6.81175111262029,-2.01490109513492E-11));
#15380=CARTESIAN_POINT('Ctrl Pts',(8.59489616869822,-6.63675111262027,-4.96226561667449));
#15381=CARTESIAN_POINT('Ctrl Pts',(5.72993077912061,-6.46175111262029,-9.92453123332939));
#15382=CARTESIAN_POINT('Ctrl Pts',(-1.73960591159264E-11,-6.28675111262028,
-9.92453123331945));
#15383=CARTESIAN_POINT('Ctrl Pts',(-5.7299307791554,-6.11175111262027,-9.92453123330931));
#15384=CARTESIAN_POINT('Ctrl Pts',(-8.59489616871534,-5.93675111262026,
-4.96226561664485));
#15385=CARTESIAN_POINT('Ctrl Pts',(-11.4598615582757,-5.76175111262029,
2.00254667023258E-11));
#15386=CARTESIAN_POINT('Ctrl Pts',(-8.59489616869799,-5.58675111262028,
4.96226561667489));
#15387=CARTESIAN_POINT('Ctrl Pts',(-5.72993077912071,-5.41175111262028,
9.92453123332933));
#15388=CARTESIAN_POINT('Ctrl Pts',(1.72890666577807E-11,-5.23675111262029,
9.92453123331945));
#15389=CARTESIAN_POINT('Ctrl Pts',(5.72993077915529,-5.06175111262028,9.92453123330937));
#15390=CARTESIAN_POINT('Ctrl Pts',(8.59489616871528,-4.88675111262027,4.96226561664494));
#15391=CARTESIAN_POINT('Ctrl Pts',(11.4598615582757,-4.7117511126203,-1.99019224533025E-11));
#15392=CARTESIAN_POINT('Ctrl Pts',(8.59489616869805,-4.53675111262028,-4.9622656166748));
#15393=CARTESIAN_POINT('Ctrl Pts',(5.72993077912025,-4.36175111262028,-9.9245312333296));
#15394=CARTESIAN_POINT('Ctrl Pts',(-1.7182074199635E-11,-4.18675111262029,
-9.92453123331945));
#15395=CARTESIAN_POINT('Ctrl Pts',(-5.72993077915518,-4.01175111262028,
-9.92453123330943));
#15396=CARTESIAN_POINT('Ctrl Pts',(-8.59489616871551,-3.83675111262027,
-4.96226561664455));
#15397=CARTESIAN_POINT('Ctrl Pts',(-11.4598615582757,-3.6617511126203,1.97783782042791E-11));
#15398=CARTESIAN_POINT('Ctrl Pts',(-8.5948961686981,-3.48675111262029,4.9622656166747));
#15399=CARTESIAN_POINT('Ctrl Pts',(-5.72993077912036,-3.31175111262029,
9.92453123332954));
#15400=CARTESIAN_POINT('Ctrl Pts',(1.70750817414893E-11,-3.1367511126203,
9.92453123331945));
#15401=CARTESIAN_POINT('Ctrl Pts',(5.72993077915508,-2.96175111262029,9.92453123330949));
#15402=CARTESIAN_POINT('Ctrl Pts',(8.59489616871546,-2.78675111262028,4.96226561664464));
#15403=CARTESIAN_POINT('Ctrl Pts',(11.4598615582757,-2.61175111262031,-2.03062516658997E-11));
#15404=CARTESIAN_POINT('Ctrl Pts',(8.59489616869815,-2.43675111262029,-4.96226561667461));
#15405=CARTESIAN_POINT('Ctrl Pts',(5.72993077912047,-2.26175111262028,-9.92453123332947));
#15406=CARTESIAN_POINT('Ctrl Pts',(-1.75322335692364E-11,-2.0867511126203,
-9.92453123331945));
#15407=CARTESIAN_POINT('Ctrl Pts',(-5.72993077915497,-1.91175111262029,
-9.92453123330955));
#15408=CARTESIAN_POINT('Ctrl Pts',(-8.5948961687154,-1.73675111262028,-4.96226561664473));
#15409=CARTESIAN_POINT('Ctrl Pts',(-11.4598615582757,-1.56175111262028,
2.01827074168764E-11));
#15410=CARTESIAN_POINT('Ctrl Pts',(-8.59489616869821,-1.38675111262029,
4.96226561667452));
#15411=CARTESIAN_POINT('Ctrl Pts',(-5.72993077912058,-1.21175111262029,
9.92453123332941));
#15412=CARTESIAN_POINT('Ctrl Pts',(1.74252411110907E-11,-1.03675111262028,
9.92453123331945));
#15413=CARTESIAN_POINT('Ctrl Pts',(5.72993077915486,-0.861751112620297,
9.92453123330961));
#15414=CARTESIAN_POINT('Ctrl Pts',(8.59489616871535,-0.686751112620287,
4.96226561664483));
#15415=CARTESIAN_POINT('Ctrl Pts',(11.4598615582757,-0.511751112620282,
-2.0059163167853E-11));
#15416=CARTESIAN_POINT('Ctrl Pts',(8.59489616869798,-0.336751112620298,
-4.96226561667492));
#15417=CARTESIAN_POINT('Ctrl Pts',(5.72993077912068,-0.161751112620292,
-9.92453123332935));
#15418=CARTESIAN_POINT('Ctrl Pts',(-1.7318248652945E-11,0.0132488873797187,
-9.92453123331945));
#15419=CARTESIAN_POINT('Ctrl Pts',(-5.72993077915532,0.188248887379698,
-9.92453123330935));
#15420=CARTESIAN_POINT('Ctrl Pts',(-8.59489616871529,0.363248887379708,
-4.96226561664492));
#15421=CARTESIAN_POINT('Ctrl Pts',(-11.4598615582757,0.538248887379713,
1.99356189188297E-11));
#15422=CARTESIAN_POINT('Ctrl Pts',(-8.59489616869803,0.713248887379697,
4.96226561667482));
#15423=CARTESIAN_POINT('Ctrl Pts',(-5.72993077912079,0.888248887379703,
9.92453123332929));
#15424=CARTESIAN_POINT('Ctrl Pts',(1.72112561947994E-11,1.06324888737971,
9.92453123331945));
#15425=CARTESIAN_POINT('Ctrl Pts',(5.72993077915521,1.23824888737969,9.92453123330941));
#15426=CARTESIAN_POINT('Ctrl Pts',(8.59489616871553,1.4132488873797,4.96226561664452));
#15427=CARTESIAN_POINT('Ctrl Pts',(11.4598615582757,1.58824888737971,-1.98120746698064E-11));
#15428=CARTESIAN_POINT('Ctrl Pts',(8.59489616869808,1.76324888737969,-4.96226561667473));
#15429=CARTESIAN_POINT('Ctrl Pts',(5.72993077912033,1.9382488873797,-9.92453123332955));
#15430=CARTESIAN_POINT('Ctrl Pts',(-1.71042637366537E-11,2.11324888737971,
-9.92453123331945));
#15431=CARTESIAN_POINT('Ctrl Pts',(-5.72993077915511,2.28824888737969,-9.92453123330947));
#15432=CARTESIAN_POINT('Ctrl Pts',(-8.59489616871547,2.4632488873797,-4.96226561664462));
#15433=CARTESIAN_POINT('Ctrl Pts',(-11.4598615582757,2.6382488873797,1.9688530420783E-11));
#15434=CARTESIAN_POINT('Ctrl Pts',(-8.59489616869814,2.81324888737972,4.96226561667464));
#15435=CARTESIAN_POINT('Ctrl Pts',(-5.72993077912044,2.98824888737969,9.92453123332949));
#15436=CARTESIAN_POINT('Ctrl Pts',(1.75614155644007E-11,3.16324888737971,
9.92453123331945));
#15437=CARTESIAN_POINT('Ctrl Pts',(5.729930779155,3.33824888737971,9.92453123330953));
#15438=CARTESIAN_POINT('Ctrl Pts',(8.59489616871542,3.51324888737969,4.96226561664471));
#15439=CARTESIAN_POINT('Ctrl Pts',(11.4598615582757,3.6882488873797,-2.02164038824036E-11));
#15440=CARTESIAN_POINT('Ctrl Pts',(8.59489616869819,3.86324888737971,-4.96226561667455));
#15441=CARTESIAN_POINT('Ctrl Pts',(5.72993077912055,4.03824888737969,-9.92453123332943));
#15442=CARTESIAN_POINT('Ctrl Pts',(-1.74544231062551E-11,4.2132488873797,
-9.92453123331945));
#15443=CARTESIAN_POINT('Ctrl Pts',(-5.72993077915489,4.3882488873797,-9.9245312333096));
#15444=CARTESIAN_POINT('Ctrl Pts',(-8.59489616871537,4.56324888737969,-4.9622656166448));
#15445=CARTESIAN_POINT('Ctrl Pts',(-11.4598615582757,4.73824888737969,2.00928596333803E-11));
#15446=CARTESIAN_POINT('Ctrl Pts',(-8.59489616869824,4.91324888737971,4.96226561667445));
#15447=CARTESIAN_POINT('Ctrl Pts',(-5.72993077912065,5.08824888737968,9.92453123332936));
#15448=CARTESIAN_POINT('Ctrl Pts',(1.73474306481094E-11,5.2632488873797,
9.92453123331945));
#15449=CARTESIAN_POINT('Ctrl Pts',(5.72993077915535,5.4382488873797,9.92453123330933));
#15450=CARTESIAN_POINT('Ctrl Pts',(8.59489616871531,5.61324888737968,4.96226561664489));
#15451=CARTESIAN_POINT('Ctrl Pts',(11.4598615582757,5.78824888737969,-1.9969315384357E-11));
#15452=CARTESIAN_POINT('Ctrl Pts',(8.59489616869802,5.9632488873797,-4.96226561667485));
#15453=CARTESIAN_POINT('Ctrl Pts',(5.72993077912076,6.13824888737968,-9.9245312333293));
#15454=CARTESIAN_POINT('Ctrl Pts',(-1.72404381899637E-11,6.31324888737969,
-9.92453123331945));
#15455=CARTESIAN_POINT('Ctrl Pts',(-5.72993077915524,6.4882488873797,-9.92453123330939));
#15456=CARTESIAN_POINT('Ctrl Pts',(-8.59489616871526,6.66324888737968,-4.96226561664499));
#15457=CARTESIAN_POINT('Ctrl Pts',(-11.4598615582757,6.83824888737969,1.98457711353336E-11));
#15458=CARTESIAN_POINT('Ctrl Pts',(-8.59489616869807,7.0132488873797,4.96226561667476));
#15459=CARTESIAN_POINT('Ctrl Pts',(-5.7299307791203,7.18824888737968,9.92453123332957));
#15460=CARTESIAN_POINT('Ctrl Pts',(1.7133445731818E-11,7.36324888737969,
9.92453123331945));
#15461=CARTESIAN_POINT('Ctrl Pts',(5.72993077915513,7.53824888737969,9.92453123330946));
#15462=CARTESIAN_POINT('Ctrl Pts',(8.59489616871549,7.7132488873797,4.96226561664459));
#15463=CARTESIAN_POINT('Ctrl Pts',(11.4598615582757,7.88824888737968,-1.97222268863103E-11));
#15464=CARTESIAN_POINT('Ctrl Pts',(8.59489616869812,8.06324888737969,-4.96226561667466));
#15465=CARTESIAN_POINT('Ctrl Pts',(5.72993077912041,8.2382488873797,-9.92453123332951));
#15466=CARTESIAN_POINT('Ctrl Pts',(-1.70264532736723E-11,8.41324888737968,
-9.92453123331945));
#15467=CARTESIAN_POINT('Ctrl Pts',(-5.72993077915503,8.58824888737968,-9.92453123330952));
#15468=CARTESIAN_POINT('Ctrl Pts',(-8.59489616871543,8.7632488873797,-4.96226561664468));
#15469=CARTESIAN_POINT('Ctrl Pts',(-11.4598615582757,8.93824888737968,2.02501003479309E-11));
#15470=CARTESIAN_POINT('Ctrl Pts',(-8.59489616869817,9.11324888737969,4.96226561667457));
#15471=CARTESIAN_POINT('Ctrl Pts',(-5.72993077912052,9.28824888737969,9.92453123332944));
#15472=CARTESIAN_POINT('Ctrl Pts',(1.74836051014194E-11,9.46324888737968,
9.92453123331945));
#15473=CARTESIAN_POINT('Ctrl Pts',(5.72993077915492,9.63824888737968,9.92453123330958));
#15474=CARTESIAN_POINT('Ctrl Pts',(8.59489616871538,9.81324888737969,4.96226561664478));
#15475=CARTESIAN_POINT('Ctrl Pts',(11.4598615582757,9.98824888737967,-2.01265560989075E-11));
#15476=CARTESIAN_POINT('Ctrl Pts',(8.59489616869823,10.1632488873797,-4.96226561667448));
#15477=CARTESIAN_POINT('Ctrl Pts',(5.72993077912063,10.3382488873797,-9.92453123332938));
#15478=CARTESIAN_POINT('Ctrl Pts',(-1.73766126432737E-11,10.5132488873797,
-9.92453123331945));
#15479=CARTESIAN_POINT('Ctrl Pts',(-5.72993077915538,10.6882488873797,-9.92453123330931));
#15480=CARTESIAN_POINT('Ctrl Pts',(-8.59489616871532,10.8632488873797,-4.96226561664487));
#15481=CARTESIAN_POINT('Ctrl Pts',(-11.4598615582757,11.0382488873797,2.00030118498842E-11));
#15482=CARTESIAN_POINT('Ctrl Pts',(-8.594896168698,11.2132488873797,4.96226561667487));
#15483=CARTESIAN_POINT('Ctrl Pts',(-5.72993077912073,11.3882488873797,9.92453123332932));
#15484=CARTESIAN_POINT('Ctrl Pts',(1.7269620185128E-11,11.5632488873797,
9.92453123331945));
#15485=CARTESIAN_POINT('Ctrl Pts',(5.72993077915527,11.7382488873797,9.92453123330938));
#15486=CARTESIAN_POINT('Ctrl Pts',(8.59489616871527,11.9132488873797,4.96226561664496));
#15487=CARTESIAN_POINT('Ctrl Pts',(11.4598615582757,12.0882488873797,-1.98794676008609E-11));
#15488=CARTESIAN_POINT('Ctrl Pts',(8.59489616869805,12.2632488873797,-4.96226561667478));
#15489=CARTESIAN_POINT('Ctrl Pts',(5.72993077912084,12.4382488873797,-9.92453123332926));
#15490=CARTESIAN_POINT('Ctrl Pts',(-1.71626277269823E-11,12.6132488873797,
-9.92453123331945));
#15491=CARTESIAN_POINT('Ctrl Pts',(-5.72993077915516,12.7882488873797,-9.92453123330944));
#15492=CARTESIAN_POINT('Ctrl Pts',(-8.5948961687155,12.9632488873797,-4.96226561664457));
#15493=CARTESIAN_POINT('Ctrl Pts',(-11.4598615582757,13.1382488873797,1.97559233518375E-11));
#15494=CARTESIAN_POINT('Ctrl Pts',(-8.59489616869811,13.3132488873797,4.96226561667469));
#15495=CARTESIAN_POINT('Ctrl Pts',(-5.72993077912038,13.4882488873797,9.92453123332952));
#15496=CARTESIAN_POINT('Ctrl Pts',(1.70556352688367E-11,13.6632488873797,
9.92453123331945));
#15497=CARTESIAN_POINT('Ctrl Pts',(5.72993077915506,13.8382488873797,9.9245312333095));
#15498=CARTESIAN_POINT('Ctrl Pts',(8.59489616871545,14.0132488873797,4.96226561664466));
#15499=CARTESIAN_POINT('Ctrl Pts',(11.4598615582757,14.1882488873797,-1.96323791028142E-11));
#15500=CARTESIAN_POINT('Ctrl Pts',(8.59489616869816,14.3632488873797,-4.96226561667459));
#15501=CARTESIAN_POINT('Ctrl Pts',(5.72993077912049,14.5382488873797,-9.92453123332946));
#15502=CARTESIAN_POINT('Ctrl Pts',(-1.75127870965837E-11,14.7132488873797,
-9.92453123331945));
#15503=CARTESIAN_POINT('Ctrl Pts',(-5.72993077915495,14.8882488873797,-9.92453123330957));
#15504=CARTESIAN_POINT('Ctrl Pts',(-8.59489616871539,15.0632488873797,-4.96226561664475));
#15505=CARTESIAN_POINT('Ctrl Pts',(-11.4598615582757,15.2382488873797,2.01602525644348E-11));
#15506=CARTESIAN_POINT('Ctrl Pts',(-8.59489616869821,15.4132488873797,4.9622656166745));
#15507=CARTESIAN_POINT('Ctrl Pts',(-5.7299307791206,15.5882488873797,9.9245312333294));
#15508=CARTESIAN_POINT('Ctrl Pts',(1.7405794638438E-11,15.7632488873797,
9.92453123331945));
#15509=CARTESIAN_POINT('Ctrl Pts',(5.72993077915484,15.9382488873797,9.92453123330963));
#15510=CARTESIAN_POINT('Ctrl Pts',(8.59489616871534,16.1132488873797,4.96226561664484));
#15511=CARTESIAN_POINT('Ctrl Pts',(11.4598615582757,16.2882488873797,-2.00367083154114E-11));
#15512=CARTESIAN_POINT('Ctrl Pts',(8.59489616869799,16.4632488873797,-4.9622656166749));
#15513=CARTESIAN_POINT('Ctrl Pts',(5.7299307791207,16.6382488873797,-9.92453123332934));
#15514=CARTESIAN_POINT('Ctrl Pts',(-1.72988021802924E-11,16.8132488873797,
-9.92453123331945));
#15515=CARTESIAN_POINT('Ctrl Pts',(-5.7299307791553,16.9882488873797,-9.92453123330936));
#15516=CARTESIAN_POINT('Ctrl Pts',(-8.59489616871529,17.1632488873797,-4.96226561664494));
#15517=CARTESIAN_POINT('Ctrl Pts',(-11.4598615582757,17.3382488873797,1.99131640663881E-11));
#15518=CARTESIAN_POINT('Ctrl Pts',(-8.59489616869804,17.5132488873797,4.96226561667481));
#15519=CARTESIAN_POINT('Ctrl Pts',(-5.72993077912081,17.6882488873797,9.92453123332928));
#15520=CARTESIAN_POINT('Ctrl Pts',(1.71918097221467E-11,17.8632488873797,
9.92453123331945));
#15521=CARTESIAN_POINT('Ctrl Pts',(5.72993077915519,18.0382488873797,9.92453123330942));
#15522=CARTESIAN_POINT('Ctrl Pts',(8.59489616871523,18.2132488873797,4.96226561664503));
#15523=CARTESIAN_POINT('Ctrl Pts',(11.4598615582757,18.3882488873797,-1.97896198173647E-11));
#15524=CARTESIAN_POINT('Ctrl Pts',(8.59489616869809,18.5632488873797,-4.96226561667471));
#15525=CARTESIAN_POINT('Ctrl Pts',(5.72993077912035,18.7382488873796,-9.92453123332954));
#15526=CARTESIAN_POINT('Ctrl Pts',(-1.7084817264001E-11,18.9132488873797,
-9.92453123331945));
#15527=CARTESIAN_POINT('Ctrl Pts',(-5.72993077915509,19.0882488873797,-9.92453123330948));
#15528=CARTESIAN_POINT('Ctrl Pts',(-8.59489616871546,19.2632488873797,-4.96226561664463));
#15529=CARTESIAN_POINT('Ctrl Pts',(-11.4598615582757,19.4382488873797,1.96660755683414E-11));
#15530=CARTESIAN_POINT('Ctrl Pts',(-8.59489616869815,19.6132488873797,4.96226561667462));
#15531=CARTESIAN_POINT('Ctrl Pts',(-5.72993077912046,19.7882488873796,9.92453123332948));
#15532=CARTESIAN_POINT('Ctrl Pts',(1.69778248058553E-11,19.9632488873797,
9.92453123331945));
#15533=CARTESIAN_POINT('Ctrl Pts',(5.72993077915498,20.1382488873797,9.92453123330955));
#15534=CARTESIAN_POINT('Ctrl Pts',(8.59489616871541,20.3132488873796,4.96226561664473));
#15535=CARTESIAN_POINT('Ctrl Pts',(11.4598615582757,20.4882488873797,-2.0193949029962E-11));
#15536=CARTESIAN_POINT('Ctrl Pts',(8.5948961686982,20.6632488873797,-4.96226561667453));
#15537=CARTESIAN_POINT('Ctrl Pts',(5.72993077912057,20.8382488873797,-9.92453123332941));
#15538=CARTESIAN_POINT('Ctrl Pts',(-1.74349766336024E-11,21.0132488873797,
-9.92453123331945));
#15539=CARTESIAN_POINT('Ctrl Pts',(-5.72993077915487,21.1882488873797,-9.92453123330961));
#15540=CARTESIAN_POINT('Ctrl Pts',(-8.59489616871535,21.3632488873797,-4.96226561664482));
#15541=CARTESIAN_POINT('Ctrl Pts',(-11.4598615582757,21.5382488873796,2.00704047809387E-11));
#15542=CARTESIAN_POINT('Ctrl Pts',(-8.59489616869825,21.7132488873797,4.96226561667444));
#15543=CARTESIAN_POINT('Ctrl Pts',(-5.72993077912067,21.8882488873797,9.92453123332935));
#15544=CARTESIAN_POINT('Ctrl Pts',(1.73279841754567E-11,22.0632488873797,
9.92453123331945));
#15545=CARTESIAN_POINT('Ctrl Pts',(2.38370069761474,22.1360503989788,9.92453123331524));
#15546=CARTESIAN_POINT('Ctrl Pts',(4.50738083181344,22.22,8.84193633985987));
#15547=CARTESIAN_POINT('Ctrl Pts',(-1.51301075899711E-11,-144.093984254242,
-8.40164026751963));
#15548=CARTESIAN_POINT('Ctrl Pts',(-4.85068927010199,-143.918984254242,
-8.4016402675109));
#15549=CARTESIAN_POINT('Ctrl Pts',(-7.27603390513785,-143.743984254242,
-4.20082013374671));
#15550=CARTESIAN_POINT('Ctrl Pts',(-9.70137854017372,-143.568984254242,
1.74701493417668E-11));
#15551=CARTESIAN_POINT('Ctrl Pts',(-7.27603390512272,-143.393984254242,
4.20082013377292));
#15552=CARTESIAN_POINT('Ctrl Pts',(-4.85068927007173,-143.218984254242,
8.40164026752836));
#15553=CARTESIAN_POINT('Ctrl Pts',(1.5129078685785E-11,-143.043984254242,
8.40164026751963));
#15554=CARTESIAN_POINT('Ctrl Pts',(4.85068927010198,-142.868984254242,8.4016402675109));
#15555=CARTESIAN_POINT('Ctrl Pts',(7.27603390513785,-142.693984254242,4.20082013374672));
#15556=CARTESIAN_POINT('Ctrl Pts',(9.70137854017372,-142.518984254242,-1.74689612655491E-11));
#15557=CARTESIAN_POINT('Ctrl Pts',(7.27603390512273,-142.343984254242,-4.20082013377291));
#15558=CARTESIAN_POINT('Ctrl Pts',(4.85068927007173,-142.168984254242,-8.40164026752836));
#15559=CARTESIAN_POINT('Ctrl Pts',(-1.51301075899711E-11,-141.993984254242,
-8.40164026751963));
#15560=CARTESIAN_POINT('Ctrl Pts',(-4.85068927010199,-141.818984254242,
-8.4016402675109));
#15561=CARTESIAN_POINT('Ctrl Pts',(-7.27603390513785,-141.643984254242,
-4.20082013374671));
#15562=CARTESIAN_POINT('Ctrl Pts',(-9.70137854017372,-141.468984254242,
1.74701493417668E-11));
#15563=CARTESIAN_POINT('Ctrl Pts',(-7.27603390512272,-141.293984254242,
4.20082013377292));
#15564=CARTESIAN_POINT('Ctrl Pts',(-4.85068927007173,-141.118984254242,
8.40164026752836));
#15565=CARTESIAN_POINT('Ctrl Pts',(1.5129078685785E-11,-140.943984254242,
8.40164026751963));
#15566=CARTESIAN_POINT('Ctrl Pts',(4.85068927010198,-140.768984254242,8.4016402675109));
#15567=CARTESIAN_POINT('Ctrl Pts',(7.27603390513785,-140.593984254242,4.20082013374672));
#15568=CARTESIAN_POINT('Ctrl Pts',(9.70137854017372,-140.418984254242,-1.74689612655491E-11));
#15569=CARTESIAN_POINT('Ctrl Pts',(7.27603390512273,-140.243984254242,-4.20082013377291));
#15570=CARTESIAN_POINT('Ctrl Pts',(4.85068927007173,-140.068984254242,-8.40164026752836));
#15571=CARTESIAN_POINT('Ctrl Pts',(-1.51301075899711E-11,-139.893984254242,
-8.40164026751963));
#15572=CARTESIAN_POINT('Ctrl Pts',(-4.85068927010199,-139.718984254242,
-8.4016402675109));
#15573=CARTESIAN_POINT('Ctrl Pts',(-7.27603390513785,-139.543984254242,
-4.20082013374671));
#15574=CARTESIAN_POINT('Ctrl Pts',(-9.70137854017372,-139.368984254242,
1.74701493417668E-11));
#15575=CARTESIAN_POINT('Ctrl Pts',(-7.27603390512272,-139.193984254242,
4.20082013377292));
#15576=CARTESIAN_POINT('Ctrl Pts',(-4.85068927007173,-139.018984254242,
8.40164026752836));
#15577=CARTESIAN_POINT('Ctrl Pts',(1.5129078685785E-11,-138.843984254242,
8.40164026751963));
#15578=CARTESIAN_POINT('Ctrl Pts',(4.85068927010198,-138.668984254242,8.4016402675109));
#15579=CARTESIAN_POINT('Ctrl Pts',(7.27603390513785,-138.493984254242,4.20082013374672));
#15580=CARTESIAN_POINT('Ctrl Pts',(9.70137854017372,-138.318984254242,-1.74689612655491E-11));
#15581=CARTESIAN_POINT('Ctrl Pts',(7.27603390512273,-138.143984254242,-4.20082013377291));
#15582=CARTESIAN_POINT('Ctrl Pts',(4.85068927007173,-137.968984254242,-8.40164026752836));
#15583=CARTESIAN_POINT('Ctrl Pts',(-1.51301075899711E-11,-137.793984254242,
-8.40164026751963));
#15584=CARTESIAN_POINT('Ctrl Pts',(-4.85068927010199,-137.618984254242,
-8.4016402675109));
#15585=CARTESIAN_POINT('Ctrl Pts',(-7.27603390513785,-137.443984254242,
-4.20082013374671));
#15586=CARTESIAN_POINT('Ctrl Pts',(-9.70137854017372,-137.268984254242,
1.74701493417668E-11));
#15587=CARTESIAN_POINT('Ctrl Pts',(-7.27603390512272,-137.093984254242,
4.20082013377292));
#15588=CARTESIAN_POINT('Ctrl Pts',(-4.85068927007173,-136.918984254242,
8.40164026752836));
#15589=CARTESIAN_POINT('Ctrl Pts',(1.5129078685785E-11,-136.743984254242,
8.40164026751963));
#15590=CARTESIAN_POINT('Ctrl Pts',(4.85068927010198,-136.568984254242,8.4016402675109));
#15591=CARTESIAN_POINT('Ctrl Pts',(7.27603390513785,-136.393984254242,4.20082013374672));
#15592=CARTESIAN_POINT('Ctrl Pts',(9.70137854017372,-136.218984254242,-1.74689612655491E-11));
#15593=CARTESIAN_POINT('Ctrl Pts',(7.27603390512273,-136.043984254242,-4.20082013377291));
#15594=CARTESIAN_POINT('Ctrl Pts',(4.85068927007173,-135.868984254242,-8.40164026752836));
#15595=CARTESIAN_POINT('Ctrl Pts',(-1.51301075899711E-11,-135.693984254242,
-8.40164026751963));
#15596=CARTESIAN_POINT('Ctrl Pts',(-4.85068927010199,-135.518984254242,
-8.4016402675109));
#15597=CARTESIAN_POINT('Ctrl Pts',(-7.27603390513785,-135.343984254242,
-4.20082013374671));
#15598=CARTESIAN_POINT('Ctrl Pts',(-9.70137854017372,-135.168984254242,
1.74701493417668E-11));
#15599=CARTESIAN_POINT('Ctrl Pts',(-7.27603390512272,-134.993984254242,
4.20082013377292));
#15600=CARTESIAN_POINT('Ctrl Pts',(-4.85068927007173,-134.818984254242,
8.40164026752836));
#15601=CARTESIAN_POINT('Ctrl Pts',(1.5129078685785E-11,-134.643984254242,
8.40164026751963));
#15602=CARTESIAN_POINT('Ctrl Pts',(4.85068927010198,-134.468984254242,8.4016402675109));
#15603=CARTESIAN_POINT('Ctrl Pts',(7.27603390513785,-134.293984254242,4.20082013374672));
#15604=CARTESIAN_POINT('Ctrl Pts',(9.70137854017372,-134.118984254242,-1.74689612655491E-11));
#15605=CARTESIAN_POINT('Ctrl Pts',(7.27603390512273,-133.943984254242,-4.20082013377291));
#15606=CARTESIAN_POINT('Ctrl Pts',(4.85068927007173,-133.768984254242,-8.40164026752836));
#15607=CARTESIAN_POINT('Ctrl Pts',(-1.51301075899711E-11,-133.593984254242,
-8.40164026751963));
#15608=CARTESIAN_POINT('Ctrl Pts',(-4.85068927010199,-133.418984254242,
-8.4016402675109));
#15609=CARTESIAN_POINT('Ctrl Pts',(-7.27603390513785,-133.243984254242,
-4.20082013374671));
#15610=CARTESIAN_POINT('Ctrl Pts',(-9.70137854017372,-133.068984254242,
1.74701493417668E-11));
#15611=CARTESIAN_POINT('Ctrl Pts',(-7.27603390512272,-132.893984254242,
4.20082013377292));
#15612=CARTESIAN_POINT('Ctrl Pts',(-4.85068927007173,-132.718984254242,
8.40164026752836));
#15613=CARTESIAN_POINT('Ctrl Pts',(1.5129078685785E-11,-132.543984254242,
8.40164026751963));
#15614=CARTESIAN_POINT('Ctrl Pts',(4.85068927010198,-132.368984254242,8.4016402675109));
#15615=CARTESIAN_POINT('Ctrl Pts',(7.27603390513785,-132.193984254242,4.20082013374672));
#15616=CARTESIAN_POINT('Ctrl Pts',(9.70137854017372,-132.018984254242,-1.74689612655491E-11));
#15617=CARTESIAN_POINT('Ctrl Pts',(7.27603390512273,-131.843984254242,-4.20082013377291));
#15618=CARTESIAN_POINT('Ctrl Pts',(4.85068927007173,-131.668984254242,-8.40164026752836));
#15619=CARTESIAN_POINT('Ctrl Pts',(-1.51301075899711E-11,-131.493984254242,
-8.40164026751963));
#15620=CARTESIAN_POINT('Ctrl Pts',(-4.85068927010199,-131.318984254242,
-8.4016402675109));
#15621=CARTESIAN_POINT('Ctrl Pts',(-7.27603390513785,-131.143984254242,
-4.20082013374671));
#15622=CARTESIAN_POINT('Ctrl Pts',(-9.70137854017372,-130.968984254242,
1.74701493417668E-11));
#15623=CARTESIAN_POINT('Ctrl Pts',(-7.27603390512272,-130.793984254242,
4.20082013377292));
#15624=CARTESIAN_POINT('Ctrl Pts',(-4.85068927007173,-130.618984254242,
8.40164026752836));
#15625=CARTESIAN_POINT('Ctrl Pts',(1.5129078685785E-11,-130.443984254242,
8.40164026751963));
#15626=CARTESIAN_POINT('Ctrl Pts',(4.85068927010198,-130.268984254242,8.4016402675109));
#15627=CARTESIAN_POINT('Ctrl Pts',(7.27603390513785,-130.093984254242,4.20082013374672));
#15628=CARTESIAN_POINT('Ctrl Pts',(9.70137854017372,-129.918984254242,-1.74689612655491E-11));
#15629=CARTESIAN_POINT('Ctrl Pts',(7.27603390512273,-129.743984254242,-4.20082013377291));
#15630=CARTESIAN_POINT('Ctrl Pts',(4.85068927007173,-129.568984254242,-8.40164026752836));
#15631=CARTESIAN_POINT('Ctrl Pts',(-1.51301075899711E-11,-129.393984254242,
-8.40164026751963));
#15632=CARTESIAN_POINT('Ctrl Pts',(-4.85068927010199,-129.218984254242,
-8.4016402675109));
#15633=CARTESIAN_POINT('Ctrl Pts',(-7.27603390513785,-129.043984254242,
-4.20082013374671));
#15634=CARTESIAN_POINT('Ctrl Pts',(-9.70137854017372,-128.868984254242,
1.74701493417668E-11));
#15635=CARTESIAN_POINT('Ctrl Pts',(-7.27603390512272,-128.693984254242,
4.20082013377292));
#15636=CARTESIAN_POINT('Ctrl Pts',(-4.85068927007173,-128.518984254242,
8.40164026752836));
#15637=CARTESIAN_POINT('Ctrl Pts',(1.5129078685785E-11,-128.343984254242,
8.40164026751963));
#15638=CARTESIAN_POINT('Ctrl Pts',(4.85068927010198,-128.168984254242,8.4016402675109));
#15639=CARTESIAN_POINT('Ctrl Pts',(7.27603390513785,-127.993984254242,4.20082013374672));
#15640=CARTESIAN_POINT('Ctrl Pts',(9.70137854017372,-127.818984254242,-1.74689612655491E-11));
#15641=CARTESIAN_POINT('Ctrl Pts',(7.27603390512273,-127.643984254242,-4.20082013377291));
#15642=CARTESIAN_POINT('Ctrl Pts',(4.85068927007173,-127.468984254242,-8.40164026752836));
#15643=CARTESIAN_POINT('Ctrl Pts',(-1.51301075899711E-11,-127.293984254242,
-8.40164026751963));
#15644=CARTESIAN_POINT('Ctrl Pts',(-4.85068927010199,-127.118984254242,
-8.4016402675109));
#15645=CARTESIAN_POINT('Ctrl Pts',(-7.27603390513785,-126.943984254242,
-4.20082013374671));
#15646=CARTESIAN_POINT('Ctrl Pts',(-9.70137854017372,-126.768984254242,
1.74701493417668E-11));
#15647=CARTESIAN_POINT('Ctrl Pts',(-7.27603390512272,-126.593984254242,
4.20082013377292));
#15648=CARTESIAN_POINT('Ctrl Pts',(-4.85068927007173,-126.418984254242,
8.40164026752836));
#15649=CARTESIAN_POINT('Ctrl Pts',(1.5129078685785E-11,-126.243984254242,
8.40164026751963));
#15650=CARTESIAN_POINT('Ctrl Pts',(4.85068927010198,-126.068984254242,8.4016402675109));
#15651=CARTESIAN_POINT('Ctrl Pts',(7.27603390513785,-125.893984254242,4.20082013374672));
#15652=CARTESIAN_POINT('Ctrl Pts',(9.70137854017372,-125.718984254242,-1.74689612655491E-11));
#15653=CARTESIAN_POINT('Ctrl Pts',(7.27603390512273,-125.543984254242,-4.20082013377291));
#15654=CARTESIAN_POINT('Ctrl Pts',(4.85068927007173,-125.368984254242,-8.40164026752836));
#15655=CARTESIAN_POINT('Ctrl Pts',(-1.51301075899711E-11,-125.193984254242,
-8.40164026751963));
#15656=CARTESIAN_POINT('Ctrl Pts',(-4.85068927010199,-125.018984254242,
-8.4016402675109));
#15657=CARTESIAN_POINT('Ctrl Pts',(-7.27603390513785,-124.843984254242,
-4.20082013374671));
#15658=CARTESIAN_POINT('Ctrl Pts',(-9.70137854017372,-124.668984254242,
1.74701493417668E-11));
#15659=CARTESIAN_POINT('Ctrl Pts',(-7.27603390512272,-124.493984254242,
4.20082013377292));
#15660=CARTESIAN_POINT('Ctrl Pts',(-4.85068927007173,-124.318984254242,
8.40164026752836));
#15661=CARTESIAN_POINT('Ctrl Pts',(1.5129078685785E-11,-124.143984254242,
8.40164026751963));
#15662=CARTESIAN_POINT('Ctrl Pts',(4.85068927010198,-123.968984254242,8.4016402675109));
#15663=CARTESIAN_POINT('Ctrl Pts',(7.27603390513785,-123.793984254242,4.20082013374672));
#15664=CARTESIAN_POINT('Ctrl Pts',(9.70137854017372,-123.618984254242,-1.74689612655491E-11));
#15665=CARTESIAN_POINT('Ctrl Pts',(7.27603390512273,-123.443984254242,-4.20082013377291));
#15666=CARTESIAN_POINT('Ctrl Pts',(4.85068927007173,-123.268984254242,-8.40164026752836));
#15667=CARTESIAN_POINT('Ctrl Pts',(-1.51301075899711E-11,-123.093984254242,
-8.40164026751963));
#15668=CARTESIAN_POINT('Ctrl Pts',(-4.85068927010199,-122.918984254242,
-8.4016402675109));
#15669=CARTESIAN_POINT('Ctrl Pts',(-7.27603390513785,-122.743984254242,
-4.20082013374671));
#15670=CARTESIAN_POINT('Ctrl Pts',(-9.70137854017372,-122.568984254242,
1.74701493417668E-11));
#15671=CARTESIAN_POINT('Ctrl Pts',(-7.27603390512272,-122.393984254242,
4.20082013377292));
#15672=CARTESIAN_POINT('Ctrl Pts',(-4.85068927007173,-122.218984254242,
8.40164026752836));
#15673=CARTESIAN_POINT('Ctrl Pts',(1.5129078685785E-11,-122.043984254242,
8.40164026751963));
#15674=CARTESIAN_POINT('Ctrl Pts',(4.85068927010198,-121.868984254242,8.4016402675109));
#15675=CARTESIAN_POINT('Ctrl Pts',(7.27603390513785,-121.693984254242,4.20082013374672));
#15676=CARTESIAN_POINT('Ctrl Pts',(9.70137854017372,-121.518984254242,-1.74689612655491E-11));
#15677=CARTESIAN_POINT('Ctrl Pts',(7.27603390512273,-121.343984254242,-4.20082013377291));
#15678=CARTESIAN_POINT('Ctrl Pts',(4.85068927007173,-121.168984254242,-8.40164026752836));
#15679=CARTESIAN_POINT('Ctrl Pts',(-1.51301075899711E-11,-120.993984254242,
-8.40164026751963));
#15680=CARTESIAN_POINT('Ctrl Pts',(-4.85068927010199,-120.818984254242,
-8.4016402675109));
#15681=CARTESIAN_POINT('Ctrl Pts',(-7.27603390513785,-120.643984254242,
-4.20082013374671));
#15682=CARTESIAN_POINT('Ctrl Pts',(-9.70137854017372,-120.468984254242,
1.74701493417668E-11));
#15683=CARTESIAN_POINT('Ctrl Pts',(-7.27603390512272,-120.293984254242,
4.20082013377292));
#15684=CARTESIAN_POINT('Ctrl Pts',(-4.85068927007173,-120.118984254242,
8.40164026752836));
#15685=CARTESIAN_POINT('Ctrl Pts',(1.5129078685785E-11,-119.943984254242,
8.40164026751963));
#15686=CARTESIAN_POINT('Ctrl Pts',(4.85068927010198,-119.768984254242,8.4016402675109));
#15687=CARTESIAN_POINT('Ctrl Pts',(7.27603390513785,-119.593984254242,4.20082013374672));
#15688=CARTESIAN_POINT('Ctrl Pts',(9.70137854017372,-119.418984254242,-1.74689612655491E-11));
#15689=CARTESIAN_POINT('Ctrl Pts',(7.27603390512273,-119.243984254242,-4.20082013377291));
#15690=CARTESIAN_POINT('Ctrl Pts',(4.85068927007173,-119.068984254242,-8.40164026752836));
#15691=CARTESIAN_POINT('Ctrl Pts',(-1.51301075899711E-11,-118.893984254242,
-8.40164026751963));
#15692=CARTESIAN_POINT('Ctrl Pts',(-4.85068927010199,-118.718984254242,
-8.4016402675109));
#15693=CARTESIAN_POINT('Ctrl Pts',(-7.27603390513785,-118.543984254242,
-4.20082013374671));
#15694=CARTESIAN_POINT('Ctrl Pts',(-9.70137854017372,-118.368984254242,
1.74701493417668E-11));
#15695=CARTESIAN_POINT('Ctrl Pts',(-7.27603390512272,-118.193984254242,
4.20082013377292));
#15696=CARTESIAN_POINT('Ctrl Pts',(-4.85068927007173,-118.018984254242,
8.40164026752836));
#15697=CARTESIAN_POINT('Ctrl Pts',(1.5129078685785E-11,-117.843984254242,
8.40164026751963));
#15698=CARTESIAN_POINT('Ctrl Pts',(4.85068927010198,-117.668984254242,8.4016402675109));
#15699=CARTESIAN_POINT('Ctrl Pts',(7.27603390513785,-117.493984254242,4.20082013374672));
#15700=CARTESIAN_POINT('Ctrl Pts',(9.70137854017372,-117.318984254242,-1.74689612655491E-11));
#15701=CARTESIAN_POINT('Ctrl Pts',(7.27603390512273,-117.143984254242,-4.20082013377291));
#15702=CARTESIAN_POINT('Ctrl Pts',(4.85068927007173,-116.968984254242,-8.40164026752836));
#15703=CARTESIAN_POINT('Ctrl Pts',(-1.51301075899711E-11,-116.793984254242,
-8.40164026751963));
#15704=CARTESIAN_POINT('Ctrl Pts',(-4.85068927010199,-116.618984254242,
-8.4016402675109));
#15705=CARTESIAN_POINT('Ctrl Pts',(-7.27603390513785,-116.443984254242,
-4.20082013374671));
#15706=CARTESIAN_POINT('Ctrl Pts',(-9.70137854017372,-116.268984254242,
1.74701493417668E-11));
#15707=CARTESIAN_POINT('Ctrl Pts',(-7.27603390512272,-116.093984254242,
4.20082013377292));
#15708=CARTESIAN_POINT('Ctrl Pts',(-4.85068927007173,-115.918984254242,
8.40164026752836));
#15709=CARTESIAN_POINT('Ctrl Pts',(1.5129078685785E-11,-115.743984254242,
8.40164026751963));
#15710=CARTESIAN_POINT('Ctrl Pts',(4.85068927010198,-115.568984254242,8.4016402675109));
#15711=CARTESIAN_POINT('Ctrl Pts',(7.27603390513785,-115.393984254242,4.20082013374672));
#15712=CARTESIAN_POINT('Ctrl Pts',(9.70137854017372,-115.218984254242,-1.74689612655491E-11));
#15713=CARTESIAN_POINT('Ctrl Pts',(7.27603390512273,-115.043984254242,-4.20082013377291));
#15714=CARTESIAN_POINT('Ctrl Pts',(4.85068927007173,-114.868984254242,-8.40164026752836));
#15715=CARTESIAN_POINT('Ctrl Pts',(-1.51301075899711E-11,-114.693984254242,
-8.40164026751963));
#15716=CARTESIAN_POINT('Ctrl Pts',(-4.85068927010199,-114.518984254242,
-8.4016402675109));
#15717=CARTESIAN_POINT('Ctrl Pts',(-7.27603390513785,-114.343984254242,
-4.20082013374671));
#15718=CARTESIAN_POINT('Ctrl Pts',(-9.70137854017372,-114.168984254242,
1.74701493417668E-11));
#15719=CARTESIAN_POINT('Ctrl Pts',(-7.27603390512272,-113.993984254242,
4.20082013377292));
#15720=CARTESIAN_POINT('Ctrl Pts',(-4.85068927007173,-113.818984254242,
8.40164026752836));
#15721=CARTESIAN_POINT('Ctrl Pts',(1.5129078685785E-11,-113.643984254242,
8.40164026751963));
#15722=CARTESIAN_POINT('Ctrl Pts',(4.85068927010198,-113.468984254242,8.4016402675109));
#15723=CARTESIAN_POINT('Ctrl Pts',(7.27603390513785,-113.293984254242,4.20082013374672));
#15724=CARTESIAN_POINT('Ctrl Pts',(9.70137854017372,-113.118984254242,-1.74689612655491E-11));
#15725=CARTESIAN_POINT('Ctrl Pts',(7.27603390512273,-112.943984254242,-4.20082013377291));
#15726=CARTESIAN_POINT('Ctrl Pts',(4.85068927007173,-112.768984254242,-8.40164026752836));
#15727=CARTESIAN_POINT('Ctrl Pts',(-1.51301075899711E-11,-112.593984254242,
-8.40164026751963));
#15728=CARTESIAN_POINT('Ctrl Pts',(-4.85068927010199,-112.418984254242,
-8.4016402675109));
#15729=CARTESIAN_POINT('Ctrl Pts',(-7.27603390513785,-112.243984254242,
-4.20082013374671));
#15730=CARTESIAN_POINT('Ctrl Pts',(-9.70137854017372,-112.068984254242,
1.74701493417668E-11));
#15731=CARTESIAN_POINT('Ctrl Pts',(-7.27603390512272,-111.893984254242,
4.20082013377292));
#15732=CARTESIAN_POINT('Ctrl Pts',(-4.85068927007173,-111.718984254242,
8.40164026752836));
#15733=CARTESIAN_POINT('Ctrl Pts',(1.5129078685785E-11,-111.543984254242,
8.40164026751963));
#15734=CARTESIAN_POINT('Ctrl Pts',(4.85068927010198,-111.368984254242,8.4016402675109));
#15735=CARTESIAN_POINT('Ctrl Pts',(7.27603390513785,-111.193984254242,4.20082013374672));
#15736=CARTESIAN_POINT('Ctrl Pts',(9.70137854017372,-111.018984254242,-1.74689612655491E-11));
#15737=CARTESIAN_POINT('Ctrl Pts',(7.27603390512273,-110.843984254242,-4.20082013377291));
#15738=CARTESIAN_POINT('Ctrl Pts',(4.85068927007173,-110.668984254242,-8.40164026752836));
#15739=CARTESIAN_POINT('Ctrl Pts',(-1.51301075899711E-11,-110.493984254242,
-8.40164026751963));
#15740=CARTESIAN_POINT('Ctrl Pts',(-4.85068927010199,-110.318984254242,
-8.4016402675109));
#15741=CARTESIAN_POINT('Ctrl Pts',(-7.27603390513785,-110.143984254242,
-4.20082013374671));
#15742=CARTESIAN_POINT('Ctrl Pts',(-9.70137854017372,-109.968984254242,
1.74701493417668E-11));
#15743=CARTESIAN_POINT('Ctrl Pts',(-7.27603390512272,-109.793984254242,
4.20082013377292));
#15744=CARTESIAN_POINT('Ctrl Pts',(-4.85068927007173,-109.618984254242,
8.40164026752836));
#15745=CARTESIAN_POINT('Ctrl Pts',(1.5129078685785E-11,-109.443984254242,
8.40164026751963));
#15746=CARTESIAN_POINT('Ctrl Pts',(4.85068927010198,-109.268984254242,8.4016402675109));
#15747=CARTESIAN_POINT('Ctrl Pts',(7.27603390513785,-109.093984254242,4.20082013374672));
#15748=CARTESIAN_POINT('Ctrl Pts',(9.70137854017372,-108.918984254242,-1.74689612655491E-11));
#15749=CARTESIAN_POINT('Ctrl Pts',(7.27603390512273,-108.743984254242,-4.20082013377291));
#15750=CARTESIAN_POINT('Ctrl Pts',(4.85068927007173,-108.568984254242,-8.40164026752836));
#15751=CARTESIAN_POINT('Ctrl Pts',(-1.51301075899711E-11,-108.393984254242,
-8.40164026751963));
#15752=CARTESIAN_POINT('Ctrl Pts',(-4.85068927010199,-108.218984254242,
-8.4016402675109));
#15753=CARTESIAN_POINT('Ctrl Pts',(-7.27603390513785,-108.043984254242,
-4.20082013374671));
#15754=CARTESIAN_POINT('Ctrl Pts',(-9.70137854017372,-107.868984254242,
1.74701493417668E-11));
#15755=CARTESIAN_POINT('Ctrl Pts',(-7.27603390512272,-107.693984254242,
4.20082013377292));
#15756=CARTESIAN_POINT('Ctrl Pts',(-4.85068927007173,-107.518984254242,
8.40164026752836));
#15757=CARTESIAN_POINT('Ctrl Pts',(1.5129078685785E-11,-107.343984254242,
8.40164026751963));
#15758=CARTESIAN_POINT('Ctrl Pts',(4.85068927010198,-107.168984254242,8.4016402675109));
#15759=CARTESIAN_POINT('Ctrl Pts',(7.27603390513785,-106.993984254242,4.20082013374672));
#15760=CARTESIAN_POINT('Ctrl Pts',(9.70137854017372,-106.818984254242,-1.74689612655491E-11));
#15761=CARTESIAN_POINT('Ctrl Pts',(7.27603390512273,-106.643984254242,-4.20082013377291));
#15762=CARTESIAN_POINT('Ctrl Pts',(4.85068927007173,-106.468984254242,-8.40164026752836));
#15763=CARTESIAN_POINT('Ctrl Pts',(-1.51301075899711E-11,-106.293984254242,
-8.40164026751963));
#15764=CARTESIAN_POINT('Ctrl Pts',(-4.85068927010199,-106.118984254242,
-8.4016402675109));
#15765=CARTESIAN_POINT('Ctrl Pts',(-7.27603390513785,-105.943984254242,
-4.20082013374671));
#15766=CARTESIAN_POINT('Ctrl Pts',(-9.70137854017372,-105.768984254242,
1.74701493417668E-11));
#15767=CARTESIAN_POINT('Ctrl Pts',(-7.27603390512272,-105.593984254242,
4.20082013377292));
#15768=CARTESIAN_POINT('Ctrl Pts',(-4.85068927007173,-105.418984254242,
8.40164026752836));
#15769=CARTESIAN_POINT('Ctrl Pts',(1.5129078685785E-11,-105.243984254242,
8.40164026751963));
#15770=CARTESIAN_POINT('Ctrl Pts',(4.85068927010198,-105.068984254242,8.4016402675109));
#15771=CARTESIAN_POINT('Ctrl Pts',(7.27603390513785,-104.893984254242,4.20082013374672));
#15772=CARTESIAN_POINT('Ctrl Pts',(9.70137854017372,-104.718984254242,-1.74689612655491E-11));
#15773=CARTESIAN_POINT('Ctrl Pts',(7.27603390512273,-104.543984254242,-4.20082013377291));
#15774=CARTESIAN_POINT('Ctrl Pts',(4.85068927007173,-104.368984254242,-8.40164026752836));
#15775=CARTESIAN_POINT('Ctrl Pts',(-1.51301075899711E-11,-104.193984254242,
-8.40164026751963));
#15776=CARTESIAN_POINT('Ctrl Pts',(-4.85068927010199,-104.018984254242,
-8.4016402675109));
#15777=CARTESIAN_POINT('Ctrl Pts',(-7.27603390513785,-103.843984254242,
-4.20082013374671));
#15778=CARTESIAN_POINT('Ctrl Pts',(-9.70137854017372,-103.668984254242,
1.74701493417668E-11));
#15779=CARTESIAN_POINT('Ctrl Pts',(-7.27603390512272,-103.493984254242,
4.20082013377292));
#15780=CARTESIAN_POINT('Ctrl Pts',(-4.85068927007173,-103.318984254242,
8.40164026752836));
#15781=CARTESIAN_POINT('Ctrl Pts',(1.5129078685785E-11,-103.143984254242,
8.40164026751963));
#15782=CARTESIAN_POINT('Ctrl Pts',(4.85068927010198,-102.968984254242,8.4016402675109));
#15783=CARTESIAN_POINT('Ctrl Pts',(7.27603390513785,-102.793984254242,4.20082013374672));
#15784=CARTESIAN_POINT('Ctrl Pts',(9.70137854017372,-102.618984254242,-1.74689612655491E-11));
#15785=CARTESIAN_POINT('Ctrl Pts',(7.27603390512273,-102.443984254242,-4.20082013377291));
#15786=CARTESIAN_POINT('Ctrl Pts',(4.85068927007173,-102.268984254242,-8.40164026752836));
#15787=CARTESIAN_POINT('Ctrl Pts',(-1.51301075899711E-11,-102.093984254242,
-8.40164026751963));
#15788=CARTESIAN_POINT('Ctrl Pts',(-4.85068927010199,-101.918984254242,
-8.4016402675109));
#15789=CARTESIAN_POINT('Ctrl Pts',(-7.27603390513785,-101.743984254242,
-4.20082013374671));
#15790=CARTESIAN_POINT('Ctrl Pts',(-9.70137854017372,-101.568984254242,
1.74701493417668E-11));
#15791=CARTESIAN_POINT('Ctrl Pts',(-7.27603390512272,-101.393984254242,
4.20082013377292));
#15792=CARTESIAN_POINT('Ctrl Pts',(-4.85068927007173,-101.218984254242,
8.40164026752836));
#15793=CARTESIAN_POINT('Ctrl Pts',(1.5129078685785E-11,-101.043984254242,
8.40164026751963));
#15794=CARTESIAN_POINT('Ctrl Pts',(4.85068927010198,-100.868984254242,8.4016402675109));
#15795=CARTESIAN_POINT('Ctrl Pts',(7.27603390513785,-100.693984254242,4.20082013374672));
#15796=CARTESIAN_POINT('Ctrl Pts',(9.70137854017372,-100.518984254242,-1.74689612655491E-11));
#15797=CARTESIAN_POINT('Ctrl Pts',(7.27603390512273,-100.343984254242,-4.20082013377291));
#15798=CARTESIAN_POINT('Ctrl Pts',(4.85068927007173,-100.168984254242,-8.40164026752836));
#15799=CARTESIAN_POINT('Ctrl Pts',(-1.51301075899711E-11,-99.9939842542418,
-8.40164026751963));
#15800=CARTESIAN_POINT('Ctrl Pts',(-4.85068927010199,-99.8189842542418,
-8.4016402675109));
#15801=CARTESIAN_POINT('Ctrl Pts',(-7.27603390513785,-99.6439842542417,
-4.20082013374671));
#15802=CARTESIAN_POINT('Ctrl Pts',(-9.70137854017372,-99.4689842542418,
1.74701493417668E-11));
#15803=CARTESIAN_POINT('Ctrl Pts',(-7.27603390512272,-99.2939842542417,
4.20082013377292));
#15804=CARTESIAN_POINT('Ctrl Pts',(-4.85068927007173,-99.1189842542418,
8.40164026752836));
#15805=CARTESIAN_POINT('Ctrl Pts',(1.5129078685785E-11,-98.9439842542418,
8.40164026751963));
#15806=CARTESIAN_POINT('Ctrl Pts',(4.85068927010198,-98.7689842542417,8.4016402675109));
#15807=CARTESIAN_POINT('Ctrl Pts',(7.27603390513785,-98.5939842542417,4.20082013374672));
#15808=CARTESIAN_POINT('Ctrl Pts',(9.70137854017372,-98.4189842542418,-1.74689612655491E-11));
#15809=CARTESIAN_POINT('Ctrl Pts',(7.27603390512273,-98.2439842542418,-4.20082013377291));
#15810=CARTESIAN_POINT('Ctrl Pts',(4.85068927007173,-98.0689842542417,-8.40164026752836));
#15811=CARTESIAN_POINT('Ctrl Pts',(-1.51301075899711E-11,-97.8939842542418,
-8.40164026751963));
#15812=CARTESIAN_POINT('Ctrl Pts',(-4.85068927010199,-97.7189842542418,
-8.4016402675109));
#15813=CARTESIAN_POINT('Ctrl Pts',(-7.27603390513785,-97.5439842542417,
-4.20082013374671));
#15814=CARTESIAN_POINT('Ctrl Pts',(-9.70137854017372,-97.3689842542418,
1.74701493417668E-11));
#15815=CARTESIAN_POINT('Ctrl Pts',(-7.27603390512272,-97.1939842542418,
4.20082013377292));
#15816=CARTESIAN_POINT('Ctrl Pts',(-4.85068927007173,-97.0189842542418,
8.40164026752836));
#15817=CARTESIAN_POINT('Ctrl Pts',(1.5129078685785E-11,-96.8439842542418,
8.40164026751963));
#15818=CARTESIAN_POINT('Ctrl Pts',(4.85068927010198,-96.6689842542418,8.4016402675109));
#15819=CARTESIAN_POINT('Ctrl Pts',(7.27603390513785,-96.4939842542417,4.20082013374672));
#15820=CARTESIAN_POINT('Ctrl Pts',(9.70137854017372,-96.3189842542418,-1.74689612655491E-11));
#15821=CARTESIAN_POINT('Ctrl Pts',(7.27603390512273,-96.1439842542418,-4.20082013377291));
#15822=CARTESIAN_POINT('Ctrl Pts',(4.85068927007173,-95.9689842542417,-8.40164026752836));
#15823=CARTESIAN_POINT('Ctrl Pts',(-1.51301075899711E-11,-95.7939842542418,
-8.40164026751963));
#15824=CARTESIAN_POINT('Ctrl Pts',(-4.85068927010199,-95.6189842542418,
-8.4016402675109));
#15825=CARTESIAN_POINT('Ctrl Pts',(-7.27603390513785,-95.4439842542418,
-4.20082013374671));
#15826=CARTESIAN_POINT('Ctrl Pts',(-9.70137854017372,-95.2689842542418,
1.74701493417668E-11));
#15827=CARTESIAN_POINT('Ctrl Pts',(-7.27603390512272,-95.0939842542418,
4.20082013377292));
#15828=CARTESIAN_POINT('Ctrl Pts',(-4.85068927007173,-94.9189842542418,
8.40164026752836));
#15829=CARTESIAN_POINT('Ctrl Pts',(1.5129078685785E-11,-94.7439842542418,
8.40164026751963));
#15830=CARTESIAN_POINT('Ctrl Pts',(4.85068927010198,-94.5689842542417,8.4016402675109));
#15831=CARTESIAN_POINT('Ctrl Pts',(7.27603390513785,-94.3939842542418,4.20082013374672));
#15832=CARTESIAN_POINT('Ctrl Pts',(9.70137854017372,-94.2189842542417,-1.74689612655491E-11));
#15833=CARTESIAN_POINT('Ctrl Pts',(7.27603390512273,-94.0439842542417,-4.20082013377291));
#15834=CARTESIAN_POINT('Ctrl Pts',(4.85068927007173,-93.8689842542418,-8.40164026752836));
#15835=CARTESIAN_POINT('Ctrl Pts',(-1.51301075899711E-11,-93.6939842542417,
-8.40164026751963));
#15836=CARTESIAN_POINT('Ctrl Pts',(-4.85068927010199,-93.5189842542417,
-8.4016402675109));
#15837=CARTESIAN_POINT('Ctrl Pts',(-7.27603390513785,-93.3439842542418,
-4.20082013374671));
#15838=CARTESIAN_POINT('Ctrl Pts',(-9.70137854017372,-93.1689842542418,
1.74701493417668E-11));
#15839=CARTESIAN_POINT('Ctrl Pts',(-7.27603390512272,-92.9939842542417,
4.20082013377292));
#15840=CARTESIAN_POINT('Ctrl Pts',(-4.85068927007173,-92.8189842542418,
8.40164026752836));
#15841=CARTESIAN_POINT('Ctrl Pts',(1.5129078685785E-11,-92.6439842542418,
8.40164026751963));
#15842=CARTESIAN_POINT('Ctrl Pts',(4.85068927010198,-92.4689842542418,8.4016402675109));
#15843=CARTESIAN_POINT('Ctrl Pts',(7.27603390513785,-92.2939842542418,4.20082013374672));
#15844=CARTESIAN_POINT('Ctrl Pts',(9.70137854017372,-92.1189842542418,-1.74689612655491E-11));
#15845=CARTESIAN_POINT('Ctrl Pts',(7.27603390512273,-91.9439842542417,-4.20082013377291));
#15846=CARTESIAN_POINT('Ctrl Pts',(4.85068927007173,-91.7689842542418,-8.40164026752836));
#15847=CARTESIAN_POINT('Ctrl Pts',(-1.51301075899711E-11,-91.5939842542418,
-8.40164026751963));
#15848=CARTESIAN_POINT('Ctrl Pts',(-4.85068927010199,-91.4189842542417,
-8.4016402675109));
#15849=CARTESIAN_POINT('Ctrl Pts',(-7.27603390513785,-91.2439842542418,
-4.20082013374671));
#15850=CARTESIAN_POINT('Ctrl Pts',(-9.70137854017372,-91.0689842542418,
1.74701493417668E-11));
#15851=CARTESIAN_POINT('Ctrl Pts',(-7.27603390512272,-90.8939842542418,
4.20082013377292));
#15852=CARTESIAN_POINT('Ctrl Pts',(-4.85068927007173,-90.7189842542418,
8.40164026752836));
#15853=CARTESIAN_POINT('Ctrl Pts',(1.5129078685785E-11,-90.5439842542418,
8.40164026751963));
#15854=CARTESIAN_POINT('Ctrl Pts',(4.85068927010198,-90.3689842542418,8.4016402675109));
#15855=CARTESIAN_POINT('Ctrl Pts',(7.27603390513785,-90.1939842542418,4.20082013374672));
#15856=CARTESIAN_POINT('Ctrl Pts',(9.70137854017372,-90.0189842542418,-1.74689612655491E-11));
#15857=CARTESIAN_POINT('Ctrl Pts',(7.27603390512273,-89.8439842542418,-4.20082013377291));
#15858=CARTESIAN_POINT('Ctrl Pts',(4.85068927007173,-89.6689842542418,-8.40164026752836));
#15859=CARTESIAN_POINT('Ctrl Pts',(-1.51301075899711E-11,-89.4939842542418,
-8.40164026751963));
#15860=CARTESIAN_POINT('Ctrl Pts',(-4.85068927010199,-89.3189842542418,
-8.4016402675109));
#15861=CARTESIAN_POINT('Ctrl Pts',(-7.27603390513785,-89.1439842542418,
-4.20082013374671));
#15862=CARTESIAN_POINT('Ctrl Pts',(-9.70137854017372,-88.9689842542418,
1.74701493417668E-11));
#15863=CARTESIAN_POINT('Ctrl Pts',(-7.27603390512272,-88.7939842542418,
4.20082013377292));
#15864=CARTESIAN_POINT('Ctrl Pts',(-4.85068927007173,-88.6189842542418,
8.40164026752836));
#15865=CARTESIAN_POINT('Ctrl Pts',(1.5129078685785E-11,-88.4439842542418,
8.40164026751963));
#15866=CARTESIAN_POINT('Ctrl Pts',(4.85068927010198,-88.2689842542418,8.4016402675109));
#15867=CARTESIAN_POINT('Ctrl Pts',(7.27603390513785,-88.0939842542418,4.20082013374672));
#15868=CARTESIAN_POINT('Ctrl Pts',(9.70137854017372,-87.9189842542418,-1.74689612655491E-11));
#15869=CARTESIAN_POINT('Ctrl Pts',(7.27603390512273,-87.7439842542418,-4.20082013377291));
#15870=CARTESIAN_POINT('Ctrl Pts',(4.85068927007173,-87.5689842542418,-8.40164026752836));
#15871=CARTESIAN_POINT('Ctrl Pts',(-1.51301075899711E-11,-87.3939842542418,
-8.40164026751963));
#15872=CARTESIAN_POINT('Ctrl Pts',(-4.85068927010199,-87.2189842542418,
-8.4016402675109));
#15873=CARTESIAN_POINT('Ctrl Pts',(-7.27603390513785,-87.0439842542418,
-4.20082013374671));
#15874=CARTESIAN_POINT('Ctrl Pts',(-9.70137854017372,-86.8689842542418,
1.74701493417668E-11));
#15875=CARTESIAN_POINT('Ctrl Pts',(-7.27603390512272,-86.6939842542418,
4.20082013377292));
#15876=CARTESIAN_POINT('Ctrl Pts',(-4.85068927007173,-86.5189842542418,
8.40164026752836));
#15877=CARTESIAN_POINT('Ctrl Pts',(1.5129078685785E-11,-86.3439842542418,
8.40164026751963));
#15878=CARTESIAN_POINT('Ctrl Pts',(4.85068927010198,-86.1689842542418,8.4016402675109));
#15879=CARTESIAN_POINT('Ctrl Pts',(7.27603390513785,-85.9939842542418,4.20082013374672));
#15880=CARTESIAN_POINT('Ctrl Pts',(9.70137854017372,-85.8189842542418,-1.74689612655491E-11));
#15881=CARTESIAN_POINT('Ctrl Pts',(7.27603390512273,-85.6439842542418,-4.20082013377291));
#15882=CARTESIAN_POINT('Ctrl Pts',(4.85068927007173,-85.4689842542418,-8.40164026752836));
#15883=CARTESIAN_POINT('Ctrl Pts',(-1.51301075899711E-11,-85.2939842542417,
-8.40164026751963));
#15884=CARTESIAN_POINT('Ctrl Pts',(-4.85068927010199,-85.1189842542418,
-8.4016402675109));
#15885=CARTESIAN_POINT('Ctrl Pts',(-7.27603390513785,-84.9439842542418,
-4.20082013374671));
#15886=CARTESIAN_POINT('Ctrl Pts',(-9.70137854017372,-84.7689842542418,
1.74701493417668E-11));
#15887=CARTESIAN_POINT('Ctrl Pts',(-7.27603390512272,-84.5939842542418,
4.20082013377292));
#15888=CARTESIAN_POINT('Ctrl Pts',(-4.85068927007173,-84.4189842542418,
8.40164026752836));
#15889=CARTESIAN_POINT('Ctrl Pts',(1.5129078685785E-11,-84.2439842542418,
8.40164026751963));
#15890=CARTESIAN_POINT('Ctrl Pts',(4.85068927010198,-84.0689842542418,8.4016402675109));
#15891=CARTESIAN_POINT('Ctrl Pts',(7.27603390513785,-83.8939842542418,4.20082013374672));
#15892=CARTESIAN_POINT('Ctrl Pts',(9.70137854017372,-83.7189842542418,-1.74689612655491E-11));
#15893=CARTESIAN_POINT('Ctrl Pts',(7.27603390512273,-83.5439842542418,-4.20082013377291));
#15894=CARTESIAN_POINT('Ctrl Pts',(4.85068927007173,-83.3689842542418,-8.40164026752836));
#15895=CARTESIAN_POINT('Ctrl Pts',(-1.51301075899711E-11,-83.1939842542418,
-8.40164026751963));
#15896=CARTESIAN_POINT('Ctrl Pts',(-4.85068927010199,-83.0189842542418,
-8.4016402675109));
#15897=CARTESIAN_POINT('Ctrl Pts',(-7.27603390513785,-82.8439842542418,
-4.20082013374671));
#15898=CARTESIAN_POINT('Ctrl Pts',(-9.70137854017372,-82.6689842542418,
1.74701493417668E-11));
#15899=CARTESIAN_POINT('Ctrl Pts',(-7.27603390512272,-82.4939842542418,
4.20082013377292));
#15900=CARTESIAN_POINT('Ctrl Pts',(-4.85068927007173,-82.3189842542418,
8.40164026752836));
#15901=CARTESIAN_POINT('Ctrl Pts',(1.5129078685785E-11,-82.1439842542418,
8.40164026751963));
#15902=CARTESIAN_POINT('Ctrl Pts',(4.85068927010198,-81.9689842542418,8.4016402675109));
#15903=CARTESIAN_POINT('Ctrl Pts',(7.27603390513785,-81.7939842542418,4.20082013374672));
#15904=CARTESIAN_POINT('Ctrl Pts',(9.70137854017372,-81.6189842542418,-1.74689612655491E-11));
#15905=CARTESIAN_POINT('Ctrl Pts',(7.27603390512273,-81.4439842542418,-4.20082013377291));
#15906=CARTESIAN_POINT('Ctrl Pts',(4.85068927007173,-81.2689842542418,-8.40164026752836));
#15907=CARTESIAN_POINT('Ctrl Pts',(-1.51301075899711E-11,-81.0939842542418,
-8.40164026751963));
#15908=CARTESIAN_POINT('Ctrl Pts',(-4.85068927010199,-80.9189842542418,
-8.4016402675109));
#15909=CARTESIAN_POINT('Ctrl Pts',(-7.27603390513785,-80.7439842542418,
-4.20082013374671));
#15910=CARTESIAN_POINT('Ctrl Pts',(-9.70137854017372,-80.5689842542418,
1.74701493417668E-11));
#15911=CARTESIAN_POINT('Ctrl Pts',(-7.27603390512272,-80.3939842542418,
4.20082013377292));
#15912=CARTESIAN_POINT('Ctrl Pts',(-4.85068927007173,-80.2189842542418,
8.40164026752836));
#15913=CARTESIAN_POINT('Ctrl Pts',(1.5129078685785E-11,-80.0439842542418,
8.40164026751963));
#15914=CARTESIAN_POINT('Ctrl Pts',(4.85068927010198,-79.8689842542418,8.4016402675109));
#15915=CARTESIAN_POINT('Ctrl Pts',(7.27603390513785,-79.6939842542418,4.20082013374672));
#15916=CARTESIAN_POINT('Ctrl Pts',(9.70137854017372,-79.5189842542418,-1.74689612655491E-11));
#15917=CARTESIAN_POINT('Ctrl Pts',(7.27603390512273,-79.3439842542418,-4.20082013377291));
#15918=CARTESIAN_POINT('Ctrl Pts',(4.85068927007173,-79.1689842542418,-8.40164026752836));
#15919=CARTESIAN_POINT('Ctrl Pts',(-1.51301075899711E-11,-78.9939842542418,
-8.40164026751963));
#15920=CARTESIAN_POINT('Ctrl Pts',(-4.85068927010199,-78.8189842542418,
-8.4016402675109));
#15921=CARTESIAN_POINT('Ctrl Pts',(-7.27603390513785,-78.6439842542418,
-4.20082013374671));
#15922=CARTESIAN_POINT('Ctrl Pts',(-9.70137854017372,-78.4689842542418,
1.74701493417668E-11));
#15923=CARTESIAN_POINT('Ctrl Pts',(-7.27603390512272,-78.2939842542418,
4.20082013377292));
#15924=CARTESIAN_POINT('Ctrl Pts',(-4.85068927007173,-78.1189842542418,
8.40164026752836));
#15925=CARTESIAN_POINT('Ctrl Pts',(1.5129078685785E-11,-77.9439842542418,
8.40164026751963));
#15926=CARTESIAN_POINT('Ctrl Pts',(4.85068927010198,-77.7689842542418,8.4016402675109));
#15927=CARTESIAN_POINT('Ctrl Pts',(7.27603390513785,-77.5939842542418,4.20082013374672));
#15928=CARTESIAN_POINT('Ctrl Pts',(9.70137854017372,-77.4189842542418,-1.74689612655491E-11));
#15929=CARTESIAN_POINT('Ctrl Pts',(7.27603390512273,-77.2439842542418,-4.20082013377291));
#15930=CARTESIAN_POINT('Ctrl Pts',(4.85068927007173,-77.0689842542418,-8.40164026752836));
#15931=CARTESIAN_POINT('Ctrl Pts',(-1.51301075899711E-11,-76.8939842542418,
-8.40164026751963));
#15932=CARTESIAN_POINT('Ctrl Pts',(-4.85068927010199,-76.7189842542418,
-8.4016402675109));
#15933=CARTESIAN_POINT('Ctrl Pts',(-7.27603390513785,-76.5439842542418,
-4.20082013374671));
#15934=CARTESIAN_POINT('Ctrl Pts',(-9.70137854017372,-76.3689842542418,
1.74701493417668E-11));
#15935=CARTESIAN_POINT('Ctrl Pts',(-7.27603390512272,-76.1939842542418,
4.20082013377292));
#15936=CARTESIAN_POINT('Ctrl Pts',(-4.85068927007173,-76.0189842542418,
8.40164026752836));
#15937=CARTESIAN_POINT('Ctrl Pts',(1.5129078685785E-11,-75.8439842542418,
8.40164026751963));
#15938=CARTESIAN_POINT('Ctrl Pts',(4.85068927010198,-75.6689842542418,8.4016402675109));
#15939=CARTESIAN_POINT('Ctrl Pts',(7.27603390513785,-75.4939842542418,4.20082013374672));
#15940=CARTESIAN_POINT('Ctrl Pts',(9.70137854017372,-75.3189842542418,-1.74689612655491E-11));
#15941=CARTESIAN_POINT('Ctrl Pts',(7.27603390512273,-75.1439842542418,-4.20082013377291));
#15942=CARTESIAN_POINT('Ctrl Pts',(4.85068927007173,-74.9689842542418,-8.40164026752836));
#15943=CARTESIAN_POINT('Ctrl Pts',(-1.51301075899711E-11,-74.7939842542418,
-8.40164026751963));
#15944=CARTESIAN_POINT('Ctrl Pts',(-4.85068927010199,-74.6189842542418,
-8.4016402675109));
#15945=CARTESIAN_POINT('Ctrl Pts',(-7.27603390513785,-74.4439842542418,
-4.20082013374671));
#15946=CARTESIAN_POINT('Ctrl Pts',(-9.70137854017372,-74.2689842542418,
1.74701493417668E-11));
#15947=CARTESIAN_POINT('Ctrl Pts',(-7.27603390512272,-74.0939842542418,
4.20082013377292));
#15948=CARTESIAN_POINT('Ctrl Pts',(-4.85068927007173,-73.9189842542418,
8.40164026752836));
#15949=CARTESIAN_POINT('Ctrl Pts',(1.5129078685785E-11,-73.7439842542418,
8.40164026751963));
#15950=CARTESIAN_POINT('Ctrl Pts',(4.85068927010198,-73.5689842542418,8.4016402675109));
#15951=CARTESIAN_POINT('Ctrl Pts',(7.27603390513785,-73.3939842542418,4.20082013374672));
#15952=CARTESIAN_POINT('Ctrl Pts',(9.70137854017372,-73.2189842542418,-1.74689612655491E-11));
#15953=CARTESIAN_POINT('Ctrl Pts',(7.27603390512273,-73.0439842542418,-4.20082013377291));
#15954=CARTESIAN_POINT('Ctrl Pts',(4.85068927007173,-72.8689842542418,-8.40164026752836));
#15955=CARTESIAN_POINT('Ctrl Pts',(-1.51301075899711E-11,-72.6939842542418,
-8.40164026751963));
#15956=CARTESIAN_POINT('Ctrl Pts',(-4.85068927010199,-72.5189842542418,
-8.4016402675109));
#15957=CARTESIAN_POINT('Ctrl Pts',(-7.27603390513785,-72.3439842542418,
-4.20082013374671));
#15958=CARTESIAN_POINT('Ctrl Pts',(-9.70137854017372,-72.1689842542418,
1.74701493417668E-11));
#15959=CARTESIAN_POINT('Ctrl Pts',(-7.27603390512272,-71.9939842542418,
4.20082013377292));
#15960=CARTESIAN_POINT('Ctrl Pts',(-4.85068927007173,-71.8189842542418,
8.40164026752836));
#15961=CARTESIAN_POINT('Ctrl Pts',(1.5129078685785E-11,-71.6439842542418,
8.40164026751963));
#15962=CARTESIAN_POINT('Ctrl Pts',(4.85068927010198,-71.4689842542418,8.4016402675109));
#15963=CARTESIAN_POINT('Ctrl Pts',(7.27603390513785,-71.2939842542418,4.20082013374672));
#15964=CARTESIAN_POINT('Ctrl Pts',(9.70137854017372,-71.1189842542418,-1.74689612655491E-11));
#15965=CARTESIAN_POINT('Ctrl Pts',(7.27603390512273,-70.9439842542418,-4.20082013377291));
#15966=CARTESIAN_POINT('Ctrl Pts',(4.85068927007173,-70.7689842542418,-8.40164026752836));
#15967=CARTESIAN_POINT('Ctrl Pts',(-1.51301075899711E-11,-70.5939842542418,
-8.40164026751963));
#15968=CARTESIAN_POINT('Ctrl Pts',(-4.85068927010199,-70.4189842542418,
-8.4016402675109));
#15969=CARTESIAN_POINT('Ctrl Pts',(-7.27603390513785,-70.2439842542418,
-4.20082013374671));
#15970=CARTESIAN_POINT('Ctrl Pts',(-9.70137854017372,-70.0689842542418,
1.74701493417668E-11));
#15971=CARTESIAN_POINT('Ctrl Pts',(-7.27603390512272,-69.8939842542418,
4.20082013377292));
#15972=CARTESIAN_POINT('Ctrl Pts',(-4.85068927007173,-69.7189842542418,
8.40164026752836));
#15973=CARTESIAN_POINT('Ctrl Pts',(1.5129078685785E-11,-69.5439842542418,
8.40164026751963));
#15974=CARTESIAN_POINT('Ctrl Pts',(4.85068927010198,-69.3689842542418,8.4016402675109));
#15975=CARTESIAN_POINT('Ctrl Pts',(7.27603390513785,-69.1939842542418,4.20082013374672));
#15976=CARTESIAN_POINT('Ctrl Pts',(9.70137854017372,-69.0189842542418,-1.74689612655491E-11));
#15977=CARTESIAN_POINT('Ctrl Pts',(7.27603390512273,-68.8439842542418,-4.20082013377291));
#15978=CARTESIAN_POINT('Ctrl Pts',(4.85068927007173,-68.6689842542418,-8.40164026752836));
#15979=CARTESIAN_POINT('Ctrl Pts',(-1.51301075899711E-11,-68.4939842542418,
-8.40164026751963));
#15980=CARTESIAN_POINT('Ctrl Pts',(-4.85068927010199,-68.3189842542418,
-8.4016402675109));
#15981=CARTESIAN_POINT('Ctrl Pts',(-7.27603390513785,-68.1439842542418,
-4.20082013374671));
#15982=CARTESIAN_POINT('Ctrl Pts',(-9.70137854017372,-67.9689842542418,
1.74701493417668E-11));
#15983=CARTESIAN_POINT('Ctrl Pts',(-7.27603390512272,-67.7939842542418,
4.20082013377292));
#15984=CARTESIAN_POINT('Ctrl Pts',(-4.85068927007173,-67.6189842542418,
8.40164026752836));
#15985=CARTESIAN_POINT('Ctrl Pts',(1.5129078685785E-11,-67.4439842542418,
8.40164026751963));
#15986=CARTESIAN_POINT('Ctrl Pts',(4.85068927010198,-67.2689842542418,8.4016402675109));
#15987=CARTESIAN_POINT('Ctrl Pts',(7.27603390513785,-67.0939842542418,4.20082013374672));
#15988=CARTESIAN_POINT('Ctrl Pts',(9.70137854017372,-66.9189842542418,-1.74689612655491E-11));
#15989=CARTESIAN_POINT('Ctrl Pts',(7.27603390512273,-66.7439842542418,-4.20082013377291));
#15990=CARTESIAN_POINT('Ctrl Pts',(4.85068927007173,-66.5689842542419,-8.40164026752836));
#15991=CARTESIAN_POINT('Ctrl Pts',(-1.51301075899711E-11,-66.3939842542418,
-8.40164026751963));
#15992=CARTESIAN_POINT('Ctrl Pts',(-4.85068927010199,-66.2189842542418,
-8.4016402675109));
#15993=CARTESIAN_POINT('Ctrl Pts',(-7.27603390513785,-66.0439842542418,
-4.20082013374671));
#15994=CARTESIAN_POINT('Ctrl Pts',(-9.70137854017372,-65.8689842542418,
1.74701493417668E-11));
#15995=CARTESIAN_POINT('Ctrl Pts',(-7.27603390512272,-65.6939842542418,
4.20082013377292));
#15996=CARTESIAN_POINT('Ctrl Pts',(-4.85068927007173,-65.5189842542418,
8.40164026752836));
#15997=CARTESIAN_POINT('Ctrl Pts',(1.5129078685785E-11,-65.3439842542418,
8.40164026751963));
#15998=CARTESIAN_POINT('Ctrl Pts',(4.85068927010198,-65.1689842542418,8.4016402675109));
#15999=CARTESIAN_POINT('Ctrl Pts',(7.27603390513785,-64.9939842542418,4.20082013374672));
#16000=CARTESIAN_POINT('Ctrl Pts',(9.70137854017372,-64.8189842542418,-1.74689612655491E-11));
#16001=CARTESIAN_POINT('Ctrl Pts',(7.27603390512273,-64.6439842542418,-4.20082013377291));
#16002=CARTESIAN_POINT('Ctrl Pts',(4.85068927007173,-64.4689842542418,-8.40164026752836));
#16003=CARTESIAN_POINT('Ctrl Pts',(-1.51301075899711E-11,-64.2939842542418,
-8.40164026751963));
#16004=CARTESIAN_POINT('Ctrl Pts',(-4.85068927010199,-64.1189842542418,
-8.4016402675109));
#16005=CARTESIAN_POINT('Ctrl Pts',(-7.27603390513785,-63.9439842542418,
-4.20082013374671));
#16006=CARTESIAN_POINT('Ctrl Pts',(-9.70137854017372,-63.7689842542418,
1.74701493417668E-11));
#16007=CARTESIAN_POINT('Ctrl Pts',(-7.27603390512272,-63.5939842542418,
4.20082013377292));
#16008=CARTESIAN_POINT('Ctrl Pts',(-4.85068927007173,-63.4189842542418,
8.40164026752836));
#16009=CARTESIAN_POINT('Ctrl Pts',(1.5129078685785E-11,-63.2439842542418,
8.40164026751963));
#16010=CARTESIAN_POINT('Ctrl Pts',(4.85068927010198,-63.0689842542418,8.4016402675109));
#16011=CARTESIAN_POINT('Ctrl Pts',(7.27603390513785,-62.8939842542418,4.20082013374672));
#16012=CARTESIAN_POINT('Ctrl Pts',(9.70137854017372,-62.7189842542418,-1.74689612655491E-11));
#16013=CARTESIAN_POINT('Ctrl Pts',(7.27603390512273,-62.5439842542418,-4.20082013377291));
#16014=CARTESIAN_POINT('Ctrl Pts',(4.85068927007173,-62.3689842542419,-8.40164026752836));
#16015=CARTESIAN_POINT('Ctrl Pts',(-1.51301075899711E-11,-62.1939842542418,
-8.40164026751963));
#16016=CARTESIAN_POINT('Ctrl Pts',(-4.85068927010199,-62.0189842542418,
-8.4016402675109));
#16017=CARTESIAN_POINT('Ctrl Pts',(-7.27603390513785,-61.8439842542418,
-4.20082013374671));
#16018=CARTESIAN_POINT('Ctrl Pts',(-9.70137854017372,-61.6689842542418,
1.74701493417668E-11));
#16019=CARTESIAN_POINT('Ctrl Pts',(-7.27603390512272,-61.4939842542418,
4.20082013377292));
#16020=CARTESIAN_POINT('Ctrl Pts',(-4.85068927007173,-61.3189842542419,
8.40164026752836));
#16021=CARTESIAN_POINT('Ctrl Pts',(1.5129078685785E-11,-61.1439842542418,
8.40164026751963));
#16022=CARTESIAN_POINT('Ctrl Pts',(4.85068927010198,-60.9689842542418,8.4016402675109));
#16023=CARTESIAN_POINT('Ctrl Pts',(7.27603390513785,-60.7939842542418,4.20082013374672));
#16024=CARTESIAN_POINT('Ctrl Pts',(9.70137854017372,-60.6189842542418,-1.74689612655491E-11));
#16025=CARTESIAN_POINT('Ctrl Pts',(7.27603390512273,-60.4439842542418,-4.20082013377291));
#16026=CARTESIAN_POINT('Ctrl Pts',(4.85068927007173,-60.2689842542419,-8.40164026752836));
#16027=CARTESIAN_POINT('Ctrl Pts',(-1.51301075899711E-11,-60.0939842542418,
-8.40164026751963));
#16028=CARTESIAN_POINT('Ctrl Pts',(-4.85068927010199,-59.9189842542418,
-8.4016402675109));
#16029=CARTESIAN_POINT('Ctrl Pts',(-7.27603390513785,-59.7439842542419,
-4.20082013374671));
#16030=CARTESIAN_POINT('Ctrl Pts',(-9.70137854017372,-59.5689842542418,
1.74701493417668E-11));
#16031=CARTESIAN_POINT('Ctrl Pts',(-7.27603390512272,-59.3939842542418,
4.20082013377292));
#16032=CARTESIAN_POINT('Ctrl Pts',(-4.85068927007173,-59.2189842542419,
8.40164026752836));
#16033=CARTESIAN_POINT('Ctrl Pts',(1.5129078685785E-11,-59.0439842542418,
8.40164026751963));
#16034=CARTESIAN_POINT('Ctrl Pts',(4.85068927010198,-58.8689842542419,8.4016402675109));
#16035=CARTESIAN_POINT('Ctrl Pts',(7.27603390513785,-58.6939842542419,4.20082013374672));
#16036=CARTESIAN_POINT('Ctrl Pts',(9.70137854017372,-58.5189842542418,-1.74689612655491E-11));
#16037=CARTESIAN_POINT('Ctrl Pts',(7.27603390512273,-58.3439842542418,-4.20082013377291));
#16038=CARTESIAN_POINT('Ctrl Pts',(4.85068927007173,-58.1689842542419,-8.40164026752836));
#16039=CARTESIAN_POINT('Ctrl Pts',(-1.51301075899711E-11,-57.9939842542418,
-8.40164026751963));
#16040=CARTESIAN_POINT('Ctrl Pts',(-4.85068927010199,-57.8189842542418,
-8.4016402675109));
#16041=CARTESIAN_POINT('Ctrl Pts',(-7.27603390513785,-57.6439842542418,
-4.20082013374671));
#16042=CARTESIAN_POINT('Ctrl Pts',(-9.70137854017372,-57.4689842542418,
1.74701493417668E-11));
#16043=CARTESIAN_POINT('Ctrl Pts',(-7.27603390512272,-57.2939842542418,
4.20082013377292));
#16044=CARTESIAN_POINT('Ctrl Pts',(-4.85068927007173,-57.1189842542418,
8.40164026752836));
#16045=CARTESIAN_POINT('Ctrl Pts',(1.5129078685785E-11,-56.9439842542418,
8.40164026751963));
#16046=CARTESIAN_POINT('Ctrl Pts',(4.85068927010198,-56.7689842542419,8.4016402675109));
#16047=CARTESIAN_POINT('Ctrl Pts',(7.27603390513785,-56.5939842542418,4.20082013374672));
#16048=CARTESIAN_POINT('Ctrl Pts',(9.70137854017372,-56.4189842542418,-1.74689612655491E-11));
#16049=CARTESIAN_POINT('Ctrl Pts',(7.27603390512273,-56.2439842542419,-4.20082013377291));
#16050=CARTESIAN_POINT('Ctrl Pts',(4.85068927007173,-56.0689842542418,-8.40164026752836));
#16051=CARTESIAN_POINT('Ctrl Pts',(-1.51301075899711E-11,-55.8939842542418,
-8.40164026751963));
#16052=CARTESIAN_POINT('Ctrl Pts',(-4.85068927010199,-55.7189842542419,
-8.4016402675109));
#16053=CARTESIAN_POINT('Ctrl Pts',(-7.27603390513785,-55.5439842542418,
-4.20082013374671));
#16054=CARTESIAN_POINT('Ctrl Pts',(-9.70137854017372,-55.3689842542418,
1.74701493417668E-11));
#16055=CARTESIAN_POINT('Ctrl Pts',(-7.27603390512272,-55.1939842542419,
4.20082013377292));
#16056=CARTESIAN_POINT('Ctrl Pts',(-4.85068927007173,-55.0189842542419,
8.40164026752836));
#16057=CARTESIAN_POINT('Ctrl Pts',(1.5129078685785E-11,-54.8439842542419,
8.40164026751963));
#16058=CARTESIAN_POINT('Ctrl Pts',(4.85068927010198,-54.6689842542418,8.4016402675109));
#16059=CARTESIAN_POINT('Ctrl Pts',(7.27603390513785,-54.4939842542419,4.20082013374672));
#16060=CARTESIAN_POINT('Ctrl Pts',(9.70137854017372,-54.3189842542419,-1.74689612655491E-11));
#16061=CARTESIAN_POINT('Ctrl Pts',(7.27603390512273,-54.1439842542419,-4.20082013377291));
#16062=CARTESIAN_POINT('Ctrl Pts',(4.85068927007173,-53.9689842542419,-8.40164026752836));
#16063=CARTESIAN_POINT('Ctrl Pts',(-1.51301075899711E-11,-53.7939842542419,
-8.40164026751963));
#16064=CARTESIAN_POINT('Ctrl Pts',(-4.85068927010199,-53.6189842542419,
-8.4016402675109));
#16065=CARTESIAN_POINT('Ctrl Pts',(-7.27603390513785,-53.4439842542418,
-4.20082013374671));
#16066=CARTESIAN_POINT('Ctrl Pts',(-9.70137854017372,-53.2689842542418,
1.74701493417668E-11));
#16067=CARTESIAN_POINT('Ctrl Pts',(-7.27603390512272,-53.0939842542418,
4.20082013377292));
#16068=CARTESIAN_POINT('Ctrl Pts',(-4.85068927007173,-52.9189842542419,
8.40164026752836));
#16069=CARTESIAN_POINT('Ctrl Pts',(1.5129078685785E-11,-52.7439842542418,
8.40164026751963));
#16070=CARTESIAN_POINT('Ctrl Pts',(4.85068927010198,-52.5689842542419,8.4016402675109));
#16071=CARTESIAN_POINT('Ctrl Pts',(7.27603390513785,-52.3939842542419,4.20082013374672));
#16072=CARTESIAN_POINT('Ctrl Pts',(9.70137854017372,-52.2189842542419,-1.74689612655491E-11));
#16073=CARTESIAN_POINT('Ctrl Pts',(7.27603390512273,-52.0439842542418,-4.20082013377291));
#16074=CARTESIAN_POINT('Ctrl Pts',(4.85068927007173,-51.8689842542419,-8.40164026752836));
#16075=CARTESIAN_POINT('Ctrl Pts',(-1.51301075899711E-11,-51.6939842542418,
-8.40164026751963));
#16076=CARTESIAN_POINT('Ctrl Pts',(-4.85068927010199,-51.5189842542419,
-8.4016402675109));
#16077=CARTESIAN_POINT('Ctrl Pts',(-7.27603390513785,-51.3439842542419,
-4.20082013374671));
#16078=CARTESIAN_POINT('Ctrl Pts',(-9.70137854017372,-51.1689842542419,
1.74701493417668E-11));
#16079=CARTESIAN_POINT('Ctrl Pts',(-7.27603390512272,-50.9939842542419,
4.20082013377292));
#16080=CARTESIAN_POINT('Ctrl Pts',(-4.85068927007173,-50.8189842542419,
8.40164026752836));
#16081=CARTESIAN_POINT('Ctrl Pts',(1.5129078685785E-11,-50.6439842542419,
8.40164026751963));
#16082=CARTESIAN_POINT('Ctrl Pts',(4.85068927010198,-50.4689842542419,8.4016402675109));
#16083=CARTESIAN_POINT('Ctrl Pts',(7.27603390513785,-50.2939842542418,4.20082013374672));
#16084=CARTESIAN_POINT('Ctrl Pts',(9.70137854017372,-50.1189842542419,-1.74689612655491E-11));
#16085=CARTESIAN_POINT('Ctrl Pts',(7.27603390512273,-49.9439842542419,-4.20082013377291));
#16086=CARTESIAN_POINT('Ctrl Pts',(4.85068927007173,-49.7689842542419,-8.40164026752836));
#16087=CARTESIAN_POINT('Ctrl Pts',(-1.51301075899711E-11,-49.5939842542419,
-8.40164026751963));
#16088=CARTESIAN_POINT('Ctrl Pts',(-4.85068927010199,-49.4189842542419,
-8.4016402675109));
#16089=CARTESIAN_POINT('Ctrl Pts',(-7.27603390513785,-49.2439842542419,
-4.20082013374671));
#16090=CARTESIAN_POINT('Ctrl Pts',(-9.70137854017372,-49.0689842542419,
1.74701493417668E-11));
#16091=CARTESIAN_POINT('Ctrl Pts',(-7.27603390512272,-48.8939842542419,
4.20082013377292));
#16092=CARTESIAN_POINT('Ctrl Pts',(-4.85068927007173,-48.7189842542419,
8.40164026752836));
#16093=CARTESIAN_POINT('Ctrl Pts',(1.5129078685785E-11,-48.5439842542419,
8.40164026751963));
#16094=CARTESIAN_POINT('Ctrl Pts',(4.85068927010198,-48.3689842542419,8.4016402675109));
#16095=CARTESIAN_POINT('Ctrl Pts',(7.27603390513785,-48.1939842542419,4.20082013374672));
#16096=CARTESIAN_POINT('Ctrl Pts',(9.70137854017372,-48.0189842542419,-1.74689612655491E-11));
#16097=CARTESIAN_POINT('Ctrl Pts',(7.27603390512273,-47.8439842542419,-4.20082013377291));
#16098=CARTESIAN_POINT('Ctrl Pts',(4.85068927007173,-47.6689842542419,-8.40164026752836));
#16099=CARTESIAN_POINT('Ctrl Pts',(-1.51301075899711E-11,-47.4939842542419,
-8.40164026751963));
#16100=CARTESIAN_POINT('Ctrl Pts',(-4.85068927010199,-47.3189842542419,
-8.4016402675109));
#16101=CARTESIAN_POINT('Ctrl Pts',(-7.27603390513785,-47.1439842542419,
-4.20082013374671));
#16102=CARTESIAN_POINT('Ctrl Pts',(-9.70137854017372,-46.9689842542419,
1.74701493417668E-11));
#16103=CARTESIAN_POINT('Ctrl Pts',(-7.27603390512272,-46.7939842542419,
4.20082013377292));
#16104=CARTESIAN_POINT('Ctrl Pts',(-4.85068927007173,-46.6189842542419,
8.40164026752836));
#16105=CARTESIAN_POINT('Ctrl Pts',(1.5129078685785E-11,-46.4439842542419,
8.40164026751963));
#16106=CARTESIAN_POINT('Ctrl Pts',(4.85068927010198,-46.2689842542419,8.4016402675109));
#16107=CARTESIAN_POINT('Ctrl Pts',(7.27603390513785,-46.0939842542419,4.20082013374672));
#16108=CARTESIAN_POINT('Ctrl Pts',(9.70137854017372,-45.9189842542419,-1.74689612655491E-11));
#16109=CARTESIAN_POINT('Ctrl Pts',(7.27603390512273,-45.7439842542419,-4.20082013377291));
#16110=CARTESIAN_POINT('Ctrl Pts',(4.85068927007173,-45.5689842542419,-8.40164026752836));
#16111=CARTESIAN_POINT('Ctrl Pts',(-1.51301075899711E-11,-45.3939842542419,
-8.40164026751963));
#16112=CARTESIAN_POINT('Ctrl Pts',(-4.85068927010199,-45.2189842542419,
-8.4016402675109));
#16113=CARTESIAN_POINT('Ctrl Pts',(-7.27603390513785,-45.0439842542419,
-4.20082013374671));
#16114=CARTESIAN_POINT('Ctrl Pts',(-9.70137854017372,-44.8689842542419,
1.74701493417668E-11));
#16115=CARTESIAN_POINT('Ctrl Pts',(-7.27603390512272,-44.6939842542419,
4.20082013377292));
#16116=CARTESIAN_POINT('Ctrl Pts',(-4.85068927007173,-44.5189842542419,
8.40164026752836));
#16117=CARTESIAN_POINT('Ctrl Pts',(1.5129078685785E-11,-44.3439842542419,
8.40164026751963));
#16118=CARTESIAN_POINT('Ctrl Pts',(4.85068927010198,-44.1689842542419,8.4016402675109));
#16119=CARTESIAN_POINT('Ctrl Pts',(7.27603390513785,-43.9939842542419,4.20082013374672));
#16120=CARTESIAN_POINT('Ctrl Pts',(9.70137854017372,-43.8189842542419,-1.74689612655491E-11));
#16121=CARTESIAN_POINT('Ctrl Pts',(7.27603390512273,-43.6439842542419,-4.20082013377291));
#16122=CARTESIAN_POINT('Ctrl Pts',(4.85068927007173,-43.4689842542419,-8.40164026752836));
#16123=CARTESIAN_POINT('Ctrl Pts',(-1.51301075899711E-11,-43.2939842542419,
-8.40164026751963));
#16124=CARTESIAN_POINT('Ctrl Pts',(-4.85068927010199,-43.1189842542419,
-8.4016402675109));
#16125=CARTESIAN_POINT('Ctrl Pts',(-7.27603390513785,-42.9439842542419,
-4.20082013374671));
#16126=CARTESIAN_POINT('Ctrl Pts',(-9.70137854017372,-42.7689842542419,
1.74701493417668E-11));
#16127=CARTESIAN_POINT('Ctrl Pts',(-7.27603390512272,-42.5939842542419,
4.20082013377292));
#16128=CARTESIAN_POINT('Ctrl Pts',(-4.85068927007173,-42.4189842542419,
8.40164026752836));
#16129=CARTESIAN_POINT('Ctrl Pts',(1.5129078685785E-11,-42.2439842542419,
8.40164026751963));
#16130=CARTESIAN_POINT('Ctrl Pts',(4.85068927010198,-42.0689842542419,8.4016402675109));
#16131=CARTESIAN_POINT('Ctrl Pts',(7.27603390513785,-41.8939842542419,4.20082013374672));
#16132=CARTESIAN_POINT('Ctrl Pts',(9.70137854017372,-41.7189842542419,-1.74689612655491E-11));
#16133=CARTESIAN_POINT('Ctrl Pts',(7.27603390512273,-41.5439842542419,-4.20082013377291));
#16134=CARTESIAN_POINT('Ctrl Pts',(4.85068927007173,-41.3689842542419,-8.40164026752836));
#16135=CARTESIAN_POINT('Ctrl Pts',(-1.51301075899711E-11,-41.1939842542419,
-8.40164026751963));
#16136=CARTESIAN_POINT('Ctrl Pts',(-4.85068927010199,-41.0189842542419,
-8.4016402675109));
#16137=CARTESIAN_POINT('Ctrl Pts',(-7.27603390513785,-40.8439842542419,
-4.20082013374671));
#16138=CARTESIAN_POINT('Ctrl Pts',(-9.70137854017372,-40.6689842542419,
1.74701493417668E-11));
#16139=CARTESIAN_POINT('Ctrl Pts',(-7.27603390512272,-40.4939842542419,
4.20082013377292));
#16140=CARTESIAN_POINT('Ctrl Pts',(-4.85068927007173,-40.3189842542419,
8.40164026752836));
#16141=CARTESIAN_POINT('Ctrl Pts',(1.5129078685785E-11,-40.1439842542419,
8.40164026751963));
#16142=CARTESIAN_POINT('Ctrl Pts',(4.85068927010198,-39.9689842542419,8.4016402675109));
#16143=CARTESIAN_POINT('Ctrl Pts',(7.27603390513785,-39.7939842542419,4.20082013374672));
#16144=CARTESIAN_POINT('Ctrl Pts',(9.70137854017372,-39.6189842542419,-1.74689612655491E-11));
#16145=CARTESIAN_POINT('Ctrl Pts',(7.27603390512273,-39.4439842542419,-4.20082013377291));
#16146=CARTESIAN_POINT('Ctrl Pts',(4.85068927007173,-39.2689842542419,-8.40164026752836));
#16147=CARTESIAN_POINT('Ctrl Pts',(-1.51301075899711E-11,-39.0939842542419,
-8.40164026751963));
#16148=CARTESIAN_POINT('Ctrl Pts',(-4.85068927010199,-38.9189842542419,
-8.4016402675109));
#16149=CARTESIAN_POINT('Ctrl Pts',(-7.27603390513785,-38.7439842542419,
-4.20082013374671));
#16150=CARTESIAN_POINT('Ctrl Pts',(-9.70137854017372,-38.5689842542419,
1.74701493417668E-11));
#16151=CARTESIAN_POINT('Ctrl Pts',(-7.27603390512272,-38.3939842542419,
4.20082013377292));
#16152=CARTESIAN_POINT('Ctrl Pts',(-4.85068927007173,-38.2189842542419,
8.40164026752836));
#16153=CARTESIAN_POINT('Ctrl Pts',(1.5129078685785E-11,-38.0439842542419,
8.40164026751963));
#16154=CARTESIAN_POINT('Ctrl Pts',(4.85068927010198,-37.8689842542419,8.4016402675109));
#16155=CARTESIAN_POINT('Ctrl Pts',(7.27603390513785,-37.6939842542419,4.20082013374672));
#16156=CARTESIAN_POINT('Ctrl Pts',(9.70137854017372,-37.5189842542419,-1.74689612655491E-11));
#16157=CARTESIAN_POINT('Ctrl Pts',(7.27603390512273,-37.3439842542419,-4.20082013377291));
#16158=CARTESIAN_POINT('Ctrl Pts',(4.85068927007173,-37.1689842542419,-8.40164026752836));
#16159=CARTESIAN_POINT('Ctrl Pts',(-1.51301075899711E-11,-36.9939842542419,
-8.40164026751963));
#16160=CARTESIAN_POINT('Ctrl Pts',(-4.85068927010199,-36.8189842542419,
-8.4016402675109));
#16161=CARTESIAN_POINT('Ctrl Pts',(-7.27603390513785,-36.6439842542419,
-4.20082013374671));
#16162=CARTESIAN_POINT('Ctrl Pts',(-9.70137854017372,-36.4689842542419,
1.74701493417668E-11));
#16163=CARTESIAN_POINT('Ctrl Pts',(-7.27603390512272,-36.2939842542419,
4.20082013377292));
#16164=CARTESIAN_POINT('Ctrl Pts',(-4.85068927007173,-36.1189842542419,
8.40164026752836));
#16165=CARTESIAN_POINT('Ctrl Pts',(1.5129078685785E-11,-35.9439842542419,
8.40164026751963));
#16166=CARTESIAN_POINT('Ctrl Pts',(4.85068927010198,-35.7689842542419,8.4016402675109));
#16167=CARTESIAN_POINT('Ctrl Pts',(7.27603390513785,-35.5939842542419,4.20082013374672));
#16168=CARTESIAN_POINT('Ctrl Pts',(9.70137854017372,-35.4189842542419,-1.74689612655491E-11));
#16169=CARTESIAN_POINT('Ctrl Pts',(7.27603390512273,-35.2439842542419,-4.20082013377291));
#16170=CARTESIAN_POINT('Ctrl Pts',(4.85068927007173,-35.0689842542419,-8.40164026752836));
#16171=CARTESIAN_POINT('Ctrl Pts',(-1.51301075899711E-11,-34.8939842542419,
-8.40164026751963));
#16172=CARTESIAN_POINT('Ctrl Pts',(-4.85068927010199,-34.7189842542419,
-8.4016402675109));
#16173=CARTESIAN_POINT('Ctrl Pts',(-7.27603390513785,-34.5439842542419,
-4.20082013374671));
#16174=CARTESIAN_POINT('Ctrl Pts',(-9.70137854017372,-34.3689842542419,
1.74701493417668E-11));
#16175=CARTESIAN_POINT('Ctrl Pts',(-7.27603390512272,-34.1939842542419,
4.20082013377292));
#16176=CARTESIAN_POINT('Ctrl Pts',(-4.85068927007173,-34.0189842542419,
8.40164026752836));
#16177=CARTESIAN_POINT('Ctrl Pts',(1.5129078685785E-11,-33.8439842542419,
8.40164026751963));
#16178=CARTESIAN_POINT('Ctrl Pts',(4.85068927010198,-33.6689842542419,8.4016402675109));
#16179=CARTESIAN_POINT('Ctrl Pts',(7.27603390513785,-33.4939842542419,4.20082013374672));
#16180=CARTESIAN_POINT('Ctrl Pts',(9.70137854017372,-33.3189842542419,-1.74689612655491E-11));
#16181=CARTESIAN_POINT('Ctrl Pts',(7.27603390512273,-33.1439842542419,-4.20082013377291));
#16182=CARTESIAN_POINT('Ctrl Pts',(4.85068927007173,-32.9689842542419,-8.40164026752836));
#16183=CARTESIAN_POINT('Ctrl Pts',(-1.51301075899711E-11,-32.7939842542419,
-8.40164026751963));
#16184=CARTESIAN_POINT('Ctrl Pts',(-4.85068927010199,-32.6189842542419,
-8.4016402675109));
#16185=CARTESIAN_POINT('Ctrl Pts',(-7.27603390513785,-32.4439842542419,
-4.20082013374671));
#16186=CARTESIAN_POINT('Ctrl Pts',(-9.70137854017372,-32.2689842542419,
1.74701493417668E-11));
#16187=CARTESIAN_POINT('Ctrl Pts',(-7.27603390512272,-32.0939842542419,
4.20082013377292));
#16188=CARTESIAN_POINT('Ctrl Pts',(-4.85068927007173,-31.9189842542419,
8.40164026752836));
#16189=CARTESIAN_POINT('Ctrl Pts',(1.5129078685785E-11,-31.7439842542419,
8.40164026751963));
#16190=CARTESIAN_POINT('Ctrl Pts',(4.85068927010198,-31.5689842542419,8.4016402675109));
#16191=CARTESIAN_POINT('Ctrl Pts',(7.27603390513785,-31.3939842542419,4.20082013374672));
#16192=CARTESIAN_POINT('Ctrl Pts',(9.70137854017372,-31.2189842542419,-1.74689612655491E-11));
#16193=CARTESIAN_POINT('Ctrl Pts',(7.27603390512273,-31.0439842542419,-4.20082013377291));
#16194=CARTESIAN_POINT('Ctrl Pts',(4.85068927007173,-30.8689842542419,-8.40164026752836));
#16195=CARTESIAN_POINT('Ctrl Pts',(-1.51301075899711E-11,-30.6939842542419,
-8.40164026751963));
#16196=CARTESIAN_POINT('Ctrl Pts',(-4.85068927010199,-30.5189842542419,
-8.4016402675109));
#16197=CARTESIAN_POINT('Ctrl Pts',(-7.27603390513785,-30.3439842542419,
-4.20082013374671));
#16198=CARTESIAN_POINT('Ctrl Pts',(-9.70137854017372,-30.1689842542419,
1.74701493417668E-11));
#16199=CARTESIAN_POINT('Ctrl Pts',(-7.27603390512272,-29.9939842542419,
4.20082013377292));
#16200=CARTESIAN_POINT('Ctrl Pts',(-4.85068927007173,-29.8189842542419,
8.40164026752836));
#16201=CARTESIAN_POINT('Ctrl Pts',(1.5129078685785E-11,-29.6439842542419,
8.40164026751963));
#16202=CARTESIAN_POINT('Ctrl Pts',(4.85068927010198,-29.4689842542419,8.4016402675109));
#16203=CARTESIAN_POINT('Ctrl Pts',(7.27603390513785,-29.2939842542419,4.20082013374672));
#16204=CARTESIAN_POINT('Ctrl Pts',(9.70137854017372,-29.1189842542419,-1.74689612655491E-11));
#16205=CARTESIAN_POINT('Ctrl Pts',(7.27603390512273,-28.9439842542419,-4.20082013377291));
#16206=CARTESIAN_POINT('Ctrl Pts',(4.85068927007173,-28.7689842542419,-8.40164026752836));
#16207=CARTESIAN_POINT('Ctrl Pts',(-1.51301075899711E-11,-28.5939842542419,
-8.40164026751963));
#16208=CARTESIAN_POINT('Ctrl Pts',(-4.85068927010199,-28.4189842542419,
-8.4016402675109));
#16209=CARTESIAN_POINT('Ctrl Pts',(-7.27603390513785,-28.2439842542419,
-4.20082013374671));
#16210=CARTESIAN_POINT('Ctrl Pts',(-9.70137854017372,-28.0689842542419,
1.74701493417668E-11));
#16211=CARTESIAN_POINT('Ctrl Pts',(-7.27603390512272,-27.8939842542419,
4.20082013377292));
#16212=CARTESIAN_POINT('Ctrl Pts',(-4.85068927007173,-27.7189842542419,
8.40164026752836));
#16213=CARTESIAN_POINT('Ctrl Pts',(1.5129078685785E-11,-27.5439842542419,
8.40164026751963));
#16214=CARTESIAN_POINT('Ctrl Pts',(4.85068927010198,-27.3689842542419,8.4016402675109));
#16215=CARTESIAN_POINT('Ctrl Pts',(7.27603390513785,-27.1939842542419,4.20082013374672));
#16216=CARTESIAN_POINT('Ctrl Pts',(9.70137854017372,-27.0189842542419,-1.74689612655491E-11));
#16217=CARTESIAN_POINT('Ctrl Pts',(7.27603390512273,-26.8439842542419,-4.20082013377291));
#16218=CARTESIAN_POINT('Ctrl Pts',(4.85068927007173,-26.6689842542419,-8.40164026752836));
#16219=CARTESIAN_POINT('Ctrl Pts',(-1.51301075899711E-11,-26.4939842542419,
-8.40164026751963));
#16220=CARTESIAN_POINT('Ctrl Pts',(-4.85068927010199,-26.3189842542419,
-8.4016402675109));
#16221=CARTESIAN_POINT('Ctrl Pts',(-7.27603390513785,-26.1439842542419,
-4.20082013374671));
#16222=CARTESIAN_POINT('Ctrl Pts',(-9.70137854017372,-25.9689842542419,
1.74701493417668E-11));
#16223=CARTESIAN_POINT('Ctrl Pts',(-7.27603390512272,-25.7939842542419,
4.20082013377292));
#16224=CARTESIAN_POINT('Ctrl Pts',(-4.85068927007173,-25.6189842542419,
8.40164026752836));
#16225=CARTESIAN_POINT('Ctrl Pts',(1.5129078685785E-11,-25.4439842542419,
8.40164026751963));
#16226=CARTESIAN_POINT('Ctrl Pts',(4.85068927010198,-25.2689842542419,8.4016402675109));
#16227=CARTESIAN_POINT('Ctrl Pts',(7.27603390513785,-25.0939842542419,4.20082013374672));
#16228=CARTESIAN_POINT('Ctrl Pts',(9.70137854017372,-24.9189842542419,-1.74689612655491E-11));
#16229=CARTESIAN_POINT('Ctrl Pts',(7.27603390512273,-24.7439842542419,-4.20082013377291));
#16230=CARTESIAN_POINT('Ctrl Pts',(4.85068927007173,-24.5689842542419,-8.40164026752836));
#16231=CARTESIAN_POINT('Ctrl Pts',(-1.51301075899711E-11,-24.3939842542419,
-8.40164026751963));
#16232=CARTESIAN_POINT('Ctrl Pts',(-4.85068927010199,-24.2189842542419,
-8.4016402675109));
#16233=CARTESIAN_POINT('Ctrl Pts',(-7.27603390513785,-24.0439842542419,
-4.20082013374671));
#16234=CARTESIAN_POINT('Ctrl Pts',(-9.70137854017372,-23.8689842542419,
1.74701493417668E-11));
#16235=CARTESIAN_POINT('Ctrl Pts',(-7.27603390512272,-23.6939842542419,
4.20082013377292));
#16236=CARTESIAN_POINT('Ctrl Pts',(-4.85068927007173,-23.5189842542419,
8.40164026752836));
#16237=CARTESIAN_POINT('Ctrl Pts',(1.5129078685785E-11,-23.3439842542419,
8.40164026751963));
#16238=CARTESIAN_POINT('Ctrl Pts',(4.85068927010198,-23.1689842542419,8.4016402675109));
#16239=CARTESIAN_POINT('Ctrl Pts',(7.27603390513785,-22.9939842542419,4.20082013374672));
#16240=CARTESIAN_POINT('Ctrl Pts',(9.70137854017372,-22.8189842542419,-1.74689612655491E-11));
#16241=CARTESIAN_POINT('Ctrl Pts',(7.27603390512273,-22.6439842542419,-4.20082013377291));
#16242=CARTESIAN_POINT('Ctrl Pts',(4.85068927007173,-22.4689842542419,-8.40164026752836));
#16243=CARTESIAN_POINT('Ctrl Pts',(-1.51301075899711E-11,-22.2939842542419,
-8.40164026751963));
#16244=CARTESIAN_POINT('Ctrl Pts',(-4.85068927010199,-22.1189842542419,
-8.4016402675109));
#16245=CARTESIAN_POINT('Ctrl Pts',(-7.27603390513785,-21.9439842542419,
-4.20082013374671));
#16246=CARTESIAN_POINT('Ctrl Pts',(-9.70137854017372,-21.7689842542419,
1.74701493417668E-11));
#16247=CARTESIAN_POINT('Ctrl Pts',(-7.27603390512272,-21.5939842542419,
4.20082013377292));
#16248=CARTESIAN_POINT('Ctrl Pts',(-4.85068927007173,-21.4189842542419,
8.40164026752836));
#16249=CARTESIAN_POINT('Ctrl Pts',(1.5129078685785E-11,-21.2439842542419,
8.40164026751963));
#16250=CARTESIAN_POINT('Ctrl Pts',(4.85068927010198,-21.0689842542419,8.4016402675109));
#16251=CARTESIAN_POINT('Ctrl Pts',(7.27603390513785,-20.8939842542419,4.20082013374672));
#16252=CARTESIAN_POINT('Ctrl Pts',(9.70137854017372,-20.7189842542419,-1.74689612655491E-11));
#16253=CARTESIAN_POINT('Ctrl Pts',(7.27603390512273,-20.5439842542419,-4.20082013377291));
#16254=CARTESIAN_POINT('Ctrl Pts',(4.85068927007173,-20.3689842542419,-8.40164026752836));
#16255=CARTESIAN_POINT('Ctrl Pts',(-1.51301075899711E-11,-20.1939842542419,
-8.40164026751963));
#16256=CARTESIAN_POINT('Ctrl Pts',(-4.85068927010199,-20.0189842542419,
-8.4016402675109));
#16257=CARTESIAN_POINT('Ctrl Pts',(-7.27603390513785,-19.8439842542419,
-4.20082013374671));
#16258=CARTESIAN_POINT('Ctrl Pts',(-9.70137854017372,-19.6689842542419,
1.74701493417668E-11));
#16259=CARTESIAN_POINT('Ctrl Pts',(-7.27603390512272,-19.4939842542419,
4.20082013377292));
#16260=CARTESIAN_POINT('Ctrl Pts',(-4.85068927007173,-19.3189842542419,
8.40164026752836));
#16261=CARTESIAN_POINT('Ctrl Pts',(1.5129078685785E-11,-19.1439842542419,
8.40164026751963));
#16262=CARTESIAN_POINT('Ctrl Pts',(4.85068927010198,-18.9689842542419,8.4016402675109));
#16263=CARTESIAN_POINT('Ctrl Pts',(7.27603390513785,-18.7939842542419,4.20082013374672));
#16264=CARTESIAN_POINT('Ctrl Pts',(9.70137854017372,-18.6189842542419,-1.74689612655491E-11));
#16265=CARTESIAN_POINT('Ctrl Pts',(7.27603390512273,-18.4439842542419,-4.20082013377291));
#16266=CARTESIAN_POINT('Ctrl Pts',(4.85068927007173,-18.2689842542419,-8.40164026752836));
#16267=CARTESIAN_POINT('Ctrl Pts',(-1.51301075899711E-11,-18.0939842542419,
-8.40164026751963));
#16268=CARTESIAN_POINT('Ctrl Pts',(-4.85068927010199,-17.9189842542419,
-8.4016402675109));
#16269=CARTESIAN_POINT('Ctrl Pts',(-7.27603390513785,-17.7439842542419,
-4.20082013374671));
#16270=CARTESIAN_POINT('Ctrl Pts',(-9.70137854017372,-17.5689842542419,
1.74701493417668E-11));
#16271=CARTESIAN_POINT('Ctrl Pts',(-7.27603390512272,-17.3939842542419,
4.20082013377292));
#16272=CARTESIAN_POINT('Ctrl Pts',(-4.85068927007173,-17.2189842542419,
8.40164026752836));
#16273=CARTESIAN_POINT('Ctrl Pts',(1.5129078685785E-11,-17.0439842542419,
8.40164026751963));
#16274=CARTESIAN_POINT('Ctrl Pts',(4.85068927010198,-16.8689842542419,8.4016402675109));
#16275=CARTESIAN_POINT('Ctrl Pts',(7.27603390513785,-16.6939842542419,4.20082013374672));
#16276=CARTESIAN_POINT('Ctrl Pts',(9.70137854017372,-16.518984254242,-1.74689612655491E-11));
#16277=CARTESIAN_POINT('Ctrl Pts',(7.27603390512273,-16.3439842542419,-4.20082013377291));
#16278=CARTESIAN_POINT('Ctrl Pts',(4.85068927007173,-16.1689842542419,-8.40164026752836));
#16279=CARTESIAN_POINT('Ctrl Pts',(-1.51301075899711E-11,-15.9939842542419,
-8.40164026751963));
#16280=CARTESIAN_POINT('Ctrl Pts',(-4.85068927010199,-15.8189842542419,
-8.4016402675109));
#16281=CARTESIAN_POINT('Ctrl Pts',(-7.27603390513785,-15.6439842542419,
-4.20082013374671));
#16282=CARTESIAN_POINT('Ctrl Pts',(-9.70137854017372,-15.4689842542419,
1.74701493417668E-11));
#16283=CARTESIAN_POINT('Ctrl Pts',(-7.27603390512272,-15.2939842542419,
4.20082013377292));
#16284=CARTESIAN_POINT('Ctrl Pts',(-4.85068927007173,-15.1189842542419,
8.40164026752836));
#16285=CARTESIAN_POINT('Ctrl Pts',(1.5129078685785E-11,-14.9439842542419,
8.40164026751963));
#16286=CARTESIAN_POINT('Ctrl Pts',(4.85068927010198,-14.7689842542419,8.4016402675109));
#16287=CARTESIAN_POINT('Ctrl Pts',(7.27603390513785,-14.5939842542419,4.20082013374672));
#16288=CARTESIAN_POINT('Ctrl Pts',(9.70137854017372,-14.4189842542419,-1.74689612655491E-11));
#16289=CARTESIAN_POINT('Ctrl Pts',(7.27603390512273,-14.2439842542419,-4.20082013377291));
#16290=CARTESIAN_POINT('Ctrl Pts',(4.85068927007173,-14.0689842542419,-8.40164026752836));
#16291=CARTESIAN_POINT('Ctrl Pts',(-1.51301075899711E-11,-13.8939842542419,
-8.40164026751963));
#16292=CARTESIAN_POINT('Ctrl Pts',(-4.85068927010199,-13.7189842542419,
-8.4016402675109));
#16293=CARTESIAN_POINT('Ctrl Pts',(-7.27603390513785,-13.5439842542419,
-4.20082013374671));
#16294=CARTESIAN_POINT('Ctrl Pts',(-9.70137854017372,-13.3689842542419,
1.74701493417668E-11));
#16295=CARTESIAN_POINT('Ctrl Pts',(-7.27603390512272,-13.193984254242,4.20082013377292));
#16296=CARTESIAN_POINT('Ctrl Pts',(-4.85068927007173,-13.018984254242,8.40164026752836));
#16297=CARTESIAN_POINT('Ctrl Pts',(1.5129078685785E-11,-12.8439842542419,
8.40164026751963));
#16298=CARTESIAN_POINT('Ctrl Pts',(4.85068927010198,-12.668984254242,8.4016402675109));
#16299=CARTESIAN_POINT('Ctrl Pts',(7.27603390513785,-12.4939842542419,4.20082013374672));
#16300=CARTESIAN_POINT('Ctrl Pts',(9.70137854017372,-12.3189842542419,-1.74689612655491E-11));
#16301=CARTESIAN_POINT('Ctrl Pts',(7.27603390512273,-12.143984254242,-4.20082013377291));
#16302=CARTESIAN_POINT('Ctrl Pts',(4.85068927007173,-11.968984254242,-8.40164026752836));
#16303=CARTESIAN_POINT('Ctrl Pts',(-1.51301075899711E-11,-11.7939842542419,
-8.40164026751963));
#16304=CARTESIAN_POINT('Ctrl Pts',(-4.85068927010199,-11.6189842542419,
-8.4016402675109));
#16305=CARTESIAN_POINT('Ctrl Pts',(-7.27603390513785,-11.443984254242,-4.20082013374671));
#16306=CARTESIAN_POINT('Ctrl Pts',(-9.70137854017372,-11.2689842542419,
1.74701493417668E-11));
#16307=CARTESIAN_POINT('Ctrl Pts',(-7.27603390512272,-11.0939842542419,
4.20082013377292));
#16308=CARTESIAN_POINT('Ctrl Pts',(-4.85068927007173,-10.918984254242,8.40164026752836));
#16309=CARTESIAN_POINT('Ctrl Pts',(1.5129078685785E-11,-10.7439842542419,
8.40164026751963));
#16310=CARTESIAN_POINT('Ctrl Pts',(4.85068927010198,-10.5689842542419,8.4016402675109));
#16311=CARTESIAN_POINT('Ctrl Pts',(7.27603390513785,-10.393984254242,4.20082013374672));
#16312=CARTESIAN_POINT('Ctrl Pts',(9.70137854017372,-10.2189842542419,-1.74689612655491E-11));
#16313=CARTESIAN_POINT('Ctrl Pts',(7.27603390512273,-10.0439842542419,-4.20082013377291));
#16314=CARTESIAN_POINT('Ctrl Pts',(4.85068927007173,-9.86898425424196,-8.40164026752836));
#16315=CARTESIAN_POINT('Ctrl Pts',(-1.51301075899711E-11,-9.69398425424195,
-8.40164026751963));
#16316=CARTESIAN_POINT('Ctrl Pts',(-4.85068927010199,-9.51898425424195,
-8.4016402675109));
#16317=CARTESIAN_POINT('Ctrl Pts',(-7.27603390513785,-9.34398425424196,
-4.20082013374671));
#16318=CARTESIAN_POINT('Ctrl Pts',(-9.70137854017372,-9.16898425424195,
1.74701493417668E-11));
#16319=CARTESIAN_POINT('Ctrl Pts',(-7.27603390512272,-8.99398425424194,
4.20082013377292));
#16320=CARTESIAN_POINT('Ctrl Pts',(-4.85068927007173,-8.81898425424197,
8.40164026752836));
#16321=CARTESIAN_POINT('Ctrl Pts',(1.5129078685785E-11,-8.64398425424195,
8.40164026751963));
#16322=CARTESIAN_POINT('Ctrl Pts',(4.85068927010198,-8.46898425424195,8.4016402675109));
#16323=CARTESIAN_POINT('Ctrl Pts',(7.27603390513785,-8.29398425424196,4.20082013374672));
#16324=CARTESIAN_POINT('Ctrl Pts',(9.70137854017372,-8.11898425424196,-1.74689612655491E-11));
#16325=CARTESIAN_POINT('Ctrl Pts',(7.27603390512273,-7.94398425424195,-4.20082013377291));
#16326=CARTESIAN_POINT('Ctrl Pts',(4.85068927007173,-7.76898425424197,-8.40164026752836));
#16327=CARTESIAN_POINT('Ctrl Pts',(-1.51301075899711E-11,-7.59398425424196,
-8.40164026751963));
#16328=CARTESIAN_POINT('Ctrl Pts',(-4.85068927010199,-7.41898425424196,
-8.4016402675109));
#16329=CARTESIAN_POINT('Ctrl Pts',(-7.27603390513785,-7.24398425424194,
-4.20082013374671));
#16330=CARTESIAN_POINT('Ctrl Pts',(-9.70137854017372,-7.06898425424196,
1.74701493417668E-11));
#16331=CARTESIAN_POINT('Ctrl Pts',(-7.27603390512272,-6.89398425424195,
4.20082013377292));
#16332=CARTESIAN_POINT('Ctrl Pts',(-4.85068927007173,-6.71898425424195,
8.40164026752836));
#16333=CARTESIAN_POINT('Ctrl Pts',(1.5129078685785E-11,-6.54398425424196,
8.40164026751963));
#16334=CARTESIAN_POINT('Ctrl Pts',(4.85068927010198,-6.36898425424197,8.4016402675109));
#16335=CARTESIAN_POINT('Ctrl Pts',(7.27603390513785,-6.19398425424195,4.20082013374672));
#16336=CARTESIAN_POINT('Ctrl Pts',(9.70137854017372,-6.01898425424197,-1.74689612655491E-11));
#16337=CARTESIAN_POINT('Ctrl Pts',(7.27603390512273,-5.84398425424196,-4.20082013377291));
#16338=CARTESIAN_POINT('Ctrl Pts',(4.85068927007173,-5.66898425424195,-8.40164026752836));
#16339=CARTESIAN_POINT('Ctrl Pts',(-1.51301075899711E-11,-5.49398425424197,
-8.40164026751963));
#16340=CARTESIAN_POINT('Ctrl Pts',(-4.85068927010199,-5.31898425424197,
-8.4016402675109));
#16341=CARTESIAN_POINT('Ctrl Pts',(-7.27603390513785,-5.14398425424195,
-4.20082013374671));
#16342=CARTESIAN_POINT('Ctrl Pts',(-9.70137854017372,-4.96898425424197,
1.74701493417668E-11));
#16343=CARTESIAN_POINT('Ctrl Pts',(-7.27603390512272,-4.79398425424196,
4.20082013377292));
#16344=CARTESIAN_POINT('Ctrl Pts',(-4.85068927007173,-4.61898425424196,
8.40164026752836));
#16345=CARTESIAN_POINT('Ctrl Pts',(1.5129078685785E-11,-4.44398425424197,
8.40164026751963));
#16346=CARTESIAN_POINT('Ctrl Pts',(4.85068927010198,-4.26898425424197,8.4016402675109));
#16347=CARTESIAN_POINT('Ctrl Pts',(7.27603390513785,-4.09398425424196,4.20082013374672));
#16348=CARTESIAN_POINT('Ctrl Pts',(9.70137854017372,-3.91898425424198,-1.74689612655491E-11));
#16349=CARTESIAN_POINT('Ctrl Pts',(7.27603390512273,-3.74398425424197,-4.20082013377291));
#16350=CARTESIAN_POINT('Ctrl Pts',(4.85068927007173,-3.56898425424196,-8.40164026752836));
#16351=CARTESIAN_POINT('Ctrl Pts',(-1.51301075899711E-11,-3.39398425424198,
-8.40164026751963));
#16352=CARTESIAN_POINT('Ctrl Pts',(-4.85068927010199,-3.21898425424198,
-8.4016402675109));
#16353=CARTESIAN_POINT('Ctrl Pts',(-7.27603390513785,-3.04398425424196,
-4.20082013374671));
#16354=CARTESIAN_POINT('Ctrl Pts',(-9.70137854017372,-2.86898425424196,
1.74701493417668E-11));
#16355=CARTESIAN_POINT('Ctrl Pts',(-7.27603390512272,-2.69398425424197,
4.20082013377292));
#16356=CARTESIAN_POINT('Ctrl Pts',(-4.85068927007173,-2.51898425424196,
8.40164026752836));
#16357=CARTESIAN_POINT('Ctrl Pts',(1.5129078685785E-11,-2.34398425424195,
8.40164026751963));
#16358=CARTESIAN_POINT('Ctrl Pts',(4.85068927010198,-2.16898425424197,8.4016402675109));
#16359=CARTESIAN_POINT('Ctrl Pts',(7.27603390513785,-1.99398425424197,4.20082013374672));
#16360=CARTESIAN_POINT('Ctrl Pts',(9.70137854017372,-1.81898425424196,-1.74689612655491E-11));
#16361=CARTESIAN_POINT('Ctrl Pts',(7.27603390512273,-1.64398425424198,-4.20082013377291));
#16362=CARTESIAN_POINT('Ctrl Pts',(4.85068927007173,-1.46898425424197,-8.40164026752836));
#16363=CARTESIAN_POINT('Ctrl Pts',(-1.51301075899711E-11,-1.29398425424196,
-8.40164026751963));
#16364=CARTESIAN_POINT('Ctrl Pts',(-4.85068927010199,-1.11898425424198,
-8.4016402675109));
#16365=CARTESIAN_POINT('Ctrl Pts',(-7.27603390513785,-0.94398425424197,
-4.20082013374671));
#16366=CARTESIAN_POINT('Ctrl Pts',(-9.70137854017372,-0.768984254241965,
1.74701493417668E-11));
#16367=CARTESIAN_POINT('Ctrl Pts',(-7.27603390512272,-0.59398425424198,
4.20082013377292));
#16368=CARTESIAN_POINT('Ctrl Pts',(-4.85068927007173,-0.418984254241974,
8.40164026752836));
#16369=CARTESIAN_POINT('Ctrl Pts',(1.5129078685785E-11,-0.243984254241963,
8.40164026751963));
#16370=CARTESIAN_POINT('Ctrl Pts',(4.85068927010198,-0.068984254241984,
8.4016402675109));
#16371=CARTESIAN_POINT('Ctrl Pts',(7.27603390513785,0.106015745758026,4.20082013374672));
#16372=CARTESIAN_POINT('Ctrl Pts',(9.70137854017372,0.28101574575803,-1.74689612655491E-11));
#16373=CARTESIAN_POINT('Ctrl Pts',(7.27603390512273,0.456015745758015,-4.20082013377291));
#16374=CARTESIAN_POINT('Ctrl Pts',(4.85068927007173,0.631015745758021,-8.40164026752836));
#16375=CARTESIAN_POINT('Ctrl Pts',(-1.51301075899711E-11,0.806015745758032,
-8.40164026751963));
#16376=CARTESIAN_POINT('Ctrl Pts',(-4.85068927010199,0.981015745758011,
-8.4016402675109));
#16377=CARTESIAN_POINT('Ctrl Pts',(-7.27603390513785,1.15601574575802,-4.20082013374671));
#16378=CARTESIAN_POINT('Ctrl Pts',(-9.70137854017372,1.33101574575803,1.74701493417668E-11));
#16379=CARTESIAN_POINT('Ctrl Pts',(-7.27603390512272,1.50601574575804,4.20082013377292));
#16380=CARTESIAN_POINT('Ctrl Pts',(-4.85068927007173,1.68101574575802,8.40164026752836));
#16381=CARTESIAN_POINT('Ctrl Pts',(1.5129078685785E-11,1.85601574575803,
8.40164026751963));
#16382=CARTESIAN_POINT('Ctrl Pts',(4.85068927010198,2.03101574575803,8.4016402675109));
#16383=CARTESIAN_POINT('Ctrl Pts',(7.27603390513785,2.20601574575802,4.20082013374672));
#16384=CARTESIAN_POINT('Ctrl Pts',(9.70137854017372,2.38101574575802,-1.74689612655491E-11));
#16385=CARTESIAN_POINT('Ctrl Pts',(7.27603390512273,2.55601574575803,-4.20082013377291));
#16386=CARTESIAN_POINT('Ctrl Pts',(4.85068927007173,2.73101574575801,-8.40164026752836));
#16387=CARTESIAN_POINT('Ctrl Pts',(-1.51301075899711E-11,2.90601574575802,
-8.40164026751963));
#16388=CARTESIAN_POINT('Ctrl Pts',(-4.85068927010199,3.08101574575803,-8.4016402675109));
#16389=CARTESIAN_POINT('Ctrl Pts',(-7.27603390513785,3.25601574575801,-4.20082013374671));
#16390=CARTESIAN_POINT('Ctrl Pts',(-9.70137854017372,3.43101574575802,1.74701493417668E-11));
#16391=CARTESIAN_POINT('Ctrl Pts',(-7.27603390512272,3.60601574575803,4.20082013377292));
#16392=CARTESIAN_POINT('Ctrl Pts',(-4.85068927007173,3.78101574575801,8.40164026752836));
#16393=CARTESIAN_POINT('Ctrl Pts',(1.5129078685785E-11,3.95601574575802,
8.40164026751963));
#16394=CARTESIAN_POINT('Ctrl Pts',(4.85068927010198,4.13101574575802,8.4016402675109));
#16395=CARTESIAN_POINT('Ctrl Pts',(7.27603390513785,4.30601574575801,4.20082013374672));
#16396=CARTESIAN_POINT('Ctrl Pts',(9.70137854017372,4.48101574575801,-1.74689612655491E-11));
#16397=CARTESIAN_POINT('Ctrl Pts',(7.27603390512273,4.65601574575802,-4.20082013377291));
#16398=CARTESIAN_POINT('Ctrl Pts',(4.85068927007173,4.831015745758,-8.40164026752836));
#16399=CARTESIAN_POINT('Ctrl Pts',(-1.51301075899711E-11,5.00601574575801,
-8.40164026751963));
#16400=CARTESIAN_POINT('Ctrl Pts',(-4.85068927010199,5.18101574575802,-8.4016402675109));
#16401=CARTESIAN_POINT('Ctrl Pts',(-7.27603390513785,5.356015745758,-4.20082013374671));
#16402=CARTESIAN_POINT('Ctrl Pts',(-9.70137854017372,5.53101574575801,1.74701493417668E-11));
#16403=CARTESIAN_POINT('Ctrl Pts',(-7.27603390512272,5.70601574575802,4.20082013377292));
#16404=CARTESIAN_POINT('Ctrl Pts',(-4.85068927007173,5.881015745758,8.40164026752836));
#16405=CARTESIAN_POINT('Ctrl Pts',(1.5129078685785E-11,6.05601574575801,
8.40164026751963));
#16406=CARTESIAN_POINT('Ctrl Pts',(4.85068927010198,6.23101574575801,8.4016402675109));
#16407=CARTESIAN_POINT('Ctrl Pts',(7.27603390513785,6.40601574575803,4.20082013374672));
#16408=CARTESIAN_POINT('Ctrl Pts',(9.70137854017372,6.581015745758,-1.74689612655491E-11));
#16409=CARTESIAN_POINT('Ctrl Pts',(7.27603390512273,6.75601574575802,-4.20082013377291));
#16410=CARTESIAN_POINT('Ctrl Pts',(4.85068927007173,6.93101574575802,-8.40164026752836));
#16411=CARTESIAN_POINT('Ctrl Pts',(-1.51301075899711E-11,7.106015745758,
-8.40164026751963));
#16412=CARTESIAN_POINT('Ctrl Pts',(-4.85068927010199,7.28101574575801,-8.4016402675109));
#16413=CARTESIAN_POINT('Ctrl Pts',(-7.27603390513785,7.45601574575802,-4.20082013374671));
#16414=CARTESIAN_POINT('Ctrl Pts',(-9.70137854017372,7.631015745758,1.74701493417668E-11));
#16415=CARTESIAN_POINT('Ctrl Pts',(-7.27603390512272,7.80601574575801,4.20082013377292));
#16416=CARTESIAN_POINT('Ctrl Pts',(-4.85068927007173,7.98101574575801,8.40164026752836));
#16417=CARTESIAN_POINT('Ctrl Pts',(1.5129078685785E-11,8.156015745758,8.40164026751963));
#16418=CARTESIAN_POINT('Ctrl Pts',(4.85068927010198,8.331015745758,8.4016402675109));
#16419=CARTESIAN_POINT('Ctrl Pts',(7.27603390513785,8.50601574575802,4.20082013374672));
#16420=CARTESIAN_POINT('Ctrl Pts',(9.70137854017372,8.68101574575799,-1.74689612655491E-11));
#16421=CARTESIAN_POINT('Ctrl Pts',(7.27603390512273,8.85601574575801,-4.20082013377291));
#16422=CARTESIAN_POINT('Ctrl Pts',(4.85068927007173,9.03101574575801,-8.40164026752836));
#16423=CARTESIAN_POINT('Ctrl Pts',(-1.51301075899711E-11,9.20601574575799,
-8.40164026751963));
#16424=CARTESIAN_POINT('Ctrl Pts',(-4.85068927010199,9.381015745758,-8.4016402675109));
#16425=CARTESIAN_POINT('Ctrl Pts',(-7.27603390513785,9.55601574575801,-4.20082013374671));
#16426=CARTESIAN_POINT('Ctrl Pts',(-9.70137854017372,9.73101574575799,1.74701493417668E-11));
#16427=CARTESIAN_POINT('Ctrl Pts',(-7.27603390512272,9.906015745758,4.20082013377292));
#16428=CARTESIAN_POINT('Ctrl Pts',(-4.85068927007173,10.081015745758,8.40164026752836));
#16429=CARTESIAN_POINT('Ctrl Pts',(1.5129078685785E-11,10.256015745758,
8.40164026751963));
#16430=CARTESIAN_POINT('Ctrl Pts',(4.85068927010198,10.431015745758,8.4016402675109));
#16431=CARTESIAN_POINT('Ctrl Pts',(7.27603390513785,10.606015745758,4.20082013374672));
#16432=CARTESIAN_POINT('Ctrl Pts',(9.70137854017372,10.781015745758,-1.74689612655491E-11));
#16433=CARTESIAN_POINT('Ctrl Pts',(7.27603390512273,10.956015745758,-4.20082013377291));
#16434=CARTESIAN_POINT('Ctrl Pts',(4.85068927007173,11.131015745758,-8.40164026752836));
#16435=CARTESIAN_POINT('Ctrl Pts',(-1.51301075899711E-11,11.306015745758,
-8.40164026751963));
#16436=CARTESIAN_POINT('Ctrl Pts',(-4.85068927010199,11.481015745758,-8.4016402675109));
#16437=CARTESIAN_POINT('Ctrl Pts',(-7.27603390513785,11.656015745758,-4.20082013374671));
#16438=CARTESIAN_POINT('Ctrl Pts',(-9.70137854017372,11.831015745758,1.74701493417668E-11));
#16439=CARTESIAN_POINT('Ctrl Pts',(-7.27603390512272,12.006015745758,4.20082013377292));
#16440=CARTESIAN_POINT('Ctrl Pts',(-4.85068927007173,12.181015745758,8.40164026752836));
#16441=CARTESIAN_POINT('Ctrl Pts',(1.5129078685785E-11,12.356015745758,
8.40164026751963));
#16442=CARTESIAN_POINT('Ctrl Pts',(4.85068927010198,12.531015745758,8.4016402675109));
#16443=CARTESIAN_POINT('Ctrl Pts',(7.27603390513785,12.706015745758,4.20082013374672));
#16444=CARTESIAN_POINT('Ctrl Pts',(9.70137854017372,12.881015745758,-1.74689612655491E-11));
#16445=CARTESIAN_POINT('Ctrl Pts',(7.27603390512273,13.056015745758,-4.20082013377291));
#16446=CARTESIAN_POINT('Ctrl Pts',(4.85068927007173,13.231015745758,-8.40164026752836));
#16447=CARTESIAN_POINT('Ctrl Pts',(-1.51301075899711E-11,13.406015745758,
-8.40164026751963));
#16448=CARTESIAN_POINT('Ctrl Pts',(-4.85068927010199,13.581015745758,-8.4016402675109));
#16449=CARTESIAN_POINT('Ctrl Pts',(-7.27603390513785,13.756015745758,-4.20082013374671));
#16450=CARTESIAN_POINT('Ctrl Pts',(-9.70137854017372,13.931015745758,1.74701493417668E-11));
#16451=CARTESIAN_POINT('Ctrl Pts',(-7.27603390512272,14.106015745758,4.20082013377292));
#16452=CARTESIAN_POINT('Ctrl Pts',(-4.85068927007173,14.281015745758,8.40164026752836));
#16453=CARTESIAN_POINT('Ctrl Pts',(1.5129078685785E-11,14.456015745758,
8.40164026751963));
#16454=CARTESIAN_POINT('Ctrl Pts',(4.85068927010198,14.631015745758,8.4016402675109));
#16455=CARTESIAN_POINT('Ctrl Pts',(7.27603390513785,14.806015745758,4.20082013374672));
#16456=CARTESIAN_POINT('Ctrl Pts',(9.70137854017372,14.981015745758,-1.74689612655491E-11));
#16457=CARTESIAN_POINT('Ctrl Pts',(7.27603390512273,15.156015745758,-4.20082013377291));
#16458=CARTESIAN_POINT('Ctrl Pts',(4.85068927007173,15.331015745758,-8.40164026752836));
#16459=CARTESIAN_POINT('Ctrl Pts',(-1.51301075899711E-11,15.506015745758,
-8.40164026751963));
#16460=CARTESIAN_POINT('Ctrl Pts',(-4.85068927010199,15.681015745758,-8.4016402675109));
#16461=CARTESIAN_POINT('Ctrl Pts',(-7.27603390513785,15.856015745758,-4.20082013374671));
#16462=CARTESIAN_POINT('Ctrl Pts',(-9.70137854017372,16.031015745758,1.74701493417668E-11));
#16463=CARTESIAN_POINT('Ctrl Pts',(-7.27603390512272,16.206015745758,4.20082013377292));
#16464=CARTESIAN_POINT('Ctrl Pts',(-4.85068927007173,16.381015745758,8.40164026752836));
#16465=CARTESIAN_POINT('Ctrl Pts',(1.5129078685785E-11,16.556015745758,
8.40164026751963));
#16466=CARTESIAN_POINT('Ctrl Pts',(4.85068927010198,16.731015745758,8.4016402675109));
#16467=CARTESIAN_POINT('Ctrl Pts',(7.27603390513785,16.906015745758,4.20082013374672));
#16468=CARTESIAN_POINT('Ctrl Pts',(9.70137854017372,17.081015745758,-1.74689612655491E-11));
#16469=CARTESIAN_POINT('Ctrl Pts',(7.27603390512273,17.256015745758,-4.20082013377291));
#16470=CARTESIAN_POINT('Ctrl Pts',(4.85068927007173,17.431015745758,-8.40164026752836));
#16471=CARTESIAN_POINT('Ctrl Pts',(-1.51301075899711E-11,17.606015745758,
-8.40164026751963));
#16472=CARTESIAN_POINT('Ctrl Pts',(-4.85068927010199,17.781015745758,-8.4016402675109));
#16473=CARTESIAN_POINT('Ctrl Pts',(-7.27603390513785,17.956015745758,-4.20082013374671));
#16474=CARTESIAN_POINT('Ctrl Pts',(-9.70137854017372,18.131015745758,1.74701493417668E-11));
#16475=CARTESIAN_POINT('Ctrl Pts',(-7.27603390512272,18.306015745758,4.20082013377292));
#16476=CARTESIAN_POINT('Ctrl Pts',(-4.85068927007173,18.481015745758,8.40164026752836));
#16477=CARTESIAN_POINT('Ctrl Pts',(1.5129078685785E-11,18.656015745758,
8.40164026751963));
#16478=CARTESIAN_POINT('Ctrl Pts',(4.85068927010198,18.831015745758,8.4016402675109));
#16479=CARTESIAN_POINT('Ctrl Pts',(7.27603390513785,19.006015745758,4.20082013374672));
#16480=CARTESIAN_POINT('Ctrl Pts',(9.70137854017372,19.181015745758,-1.74689612655491E-11));
#16481=CARTESIAN_POINT('Ctrl Pts',(7.27603390512273,19.356015745758,-4.20082013377291));
#16482=CARTESIAN_POINT('Ctrl Pts',(4.85068927007173,19.531015745758,-8.40164026752836));
#16483=CARTESIAN_POINT('Ctrl Pts',(-1.51301075899711E-11,19.706015745758,
-8.40164026751963));
#16484=CARTESIAN_POINT('Ctrl Pts',(-4.85068927010199,19.881015745758,-8.4016402675109));
#16485=CARTESIAN_POINT('Ctrl Pts',(-7.27603390513785,20.056015745758,-4.20082013374671));
#16486=CARTESIAN_POINT('Ctrl Pts',(-9.70137854017372,20.231015745758,1.74701493417668E-11));
#16487=CARTESIAN_POINT('Ctrl Pts',(-7.27603390512272,20.406015745758,4.20082013377292));
#16488=CARTESIAN_POINT('Ctrl Pts',(-4.85068927007173,20.581015745758,8.40164026752836));
#16489=CARTESIAN_POINT('Ctrl Pts',(1.5129078685785E-11,20.756015745758,
8.40164026751963));
#16490=CARTESIAN_POINT('Ctrl Pts',(4.85068927010198,20.931015745758,8.4016402675109));
#16491=CARTESIAN_POINT('Ctrl Pts',(7.27603390513785,21.106015745758,4.20082013374672));
#16492=CARTESIAN_POINT('Ctrl Pts',(9.70137854017372,21.281015745758,-1.74689612655491E-11));
#16493=CARTESIAN_POINT('Ctrl Pts',(7.27603390512273,21.456015745758,-4.20082013377291));
#16494=CARTESIAN_POINT('Ctrl Pts',(4.85068927007173,21.631015745758,-8.40164026752836));
#16495=CARTESIAN_POINT('Ctrl Pts',(-1.51301075899711E-11,21.806015745758,
-8.40164026751963));
#16496=CARTESIAN_POINT('Ctrl Pts',(-4.85068927010199,21.981015745758,-8.4016402675109));
#16497=CARTESIAN_POINT('Ctrl Pts',(-7.27603390513785,22.156015745758,-4.20082013374671));
#16498=CARTESIAN_POINT('Ctrl Pts',(-9.70137854017372,22.331015745758,1.74701493417668E-11));
#16499=CARTESIAN_POINT('Ctrl Pts',(-7.27603390512272,22.506015745758,4.20082013377292));
#16500=CARTESIAN_POINT('Ctrl Pts',(-4.85068927007173,22.681015745758,8.40164026752836));
#16501=CARTESIAN_POINT('Ctrl Pts',(1.5129078685785E-11,22.856015745758,
8.40164026751963));
#16502=CARTESIAN_POINT('Ctrl Pts',(4.85068927010198,23.031015745758,8.4016402675109));
#16503=CARTESIAN_POINT('Ctrl Pts',(7.27603390513785,23.206015745758,4.20082013374672));
#16504=CARTESIAN_POINT('Ctrl Pts',(9.70137854017372,23.381015745758,-1.74689612655491E-11));
#16505=CARTESIAN_POINT('Ctrl Pts',(7.27603390512273,23.556015745758,-4.20082013377291));
#16506=CARTESIAN_POINT('Ctrl Pts',(4.85068927007173,23.731015745758,-8.40164026752836));
#16507=CARTESIAN_POINT('Ctrl Pts',(-1.51301075899711E-11,23.906015745758,
-8.40164026751963));
#16508=CARTESIAN_POINT('Ctrl Pts',(-4.85068927010199,24.081015745758,-8.4016402675109));
#16509=CARTESIAN_POINT('Ctrl Pts',(-7.27603390513785,24.256015745758,-4.20082013374671));
#16510=CARTESIAN_POINT('Ctrl Pts',(-9.70137854017372,24.431015745758,1.74701493417668E-11));
#16511=CARTESIAN_POINT('Ctrl Pts',(-7.27603390512272,24.606015745758,4.20082013377292));
#16512=CARTESIAN_POINT('Ctrl Pts',(-4.85068927007173,24.781015745758,8.40164026752836));
#16513=CARTESIAN_POINT('Ctrl Pts',(1.5129078685785E-11,24.956015745758,
8.40164026751963));
#16514=CARTESIAN_POINT('Ctrl Pts',(4.85068927010198,25.131015745758,8.4016402675109));
#16515=CARTESIAN_POINT('Ctrl Pts',(7.27603390513785,25.306015745758,4.20082013374672));
#16516=CARTESIAN_POINT('Ctrl Pts',(9.70137854017372,25.481015745758,-1.74689612655491E-11));
#16517=CARTESIAN_POINT('Ctrl Pts',(7.27603390512273,25.656015745758,-4.20082013377291));
#16518=CARTESIAN_POINT('Ctrl Pts',(4.85068927007173,25.831015745758,-8.40164026752836));
#16519=CARTESIAN_POINT('Ctrl Pts',(-1.51301075899711E-11,26.006015745758,
-8.40164026751963));
#16520=CARTESIAN_POINT('Ctrl Pts',(-1.4702867290402E-11,-143.970483118095,
-8.16439679232146));
#16521=CARTESIAN_POINT('Ctrl Pts',(-4.71371668583241,-143.795483118095,
-8.16439679231297));
#16522=CARTESIAN_POINT('Ctrl Pts',(-7.07057502873392,-143.620483118095,
-4.082198396148));
#16523=CARTESIAN_POINT('Ctrl Pts',(-9.42743337163542,-143.445483118095,
1.69768315121407E-11));
#16524=CARTESIAN_POINT('Ctrl Pts',(-7.07057502871922,-143.270483118095,
4.08219839617346));
#16525=CARTESIAN_POINT('Ctrl Pts',(-4.71371668580301,-143.095483118095,
8.16439679232994));
#16526=CARTESIAN_POINT('Ctrl Pts',(1.47018674401621E-11,-142.920483118095,
8.16439679232146));
#16527=CARTESIAN_POINT('Ctrl Pts',(4.71371668583241,-142.745483118095,8.16439679231297));
#16528=CARTESIAN_POINT('Ctrl Pts',(7.07057502873392,-142.570483118095,4.082198396148));
#16529=CARTESIAN_POINT('Ctrl Pts',(9.42743337163542,-142.395483118095,-1.69756769845304E-11));
#16530=CARTESIAN_POINT('Ctrl Pts',(7.07057502871922,-142.220483118095,-4.08219839617346));
#16531=CARTESIAN_POINT('Ctrl Pts',(4.71371668580301,-142.045483118095,-8.16439679232994));
#16532=CARTESIAN_POINT('Ctrl Pts',(-1.4702867290402E-11,-141.870483118095,
-8.16439679232146));
#16533=CARTESIAN_POINT('Ctrl Pts',(-4.71371668583241,-141.695483118095,
-8.16439679231297));
#16534=CARTESIAN_POINT('Ctrl Pts',(-7.07057502873392,-141.520483118095,
-4.082198396148));
#16535=CARTESIAN_POINT('Ctrl Pts',(-9.42743337163542,-141.345483118095,
1.69768315121407E-11));
#16536=CARTESIAN_POINT('Ctrl Pts',(-7.07057502871922,-141.170483118095,
4.08219839617346));
#16537=CARTESIAN_POINT('Ctrl Pts',(-4.71371668580301,-140.995483118095,
8.16439679232994));
#16538=CARTESIAN_POINT('Ctrl Pts',(1.47018674401621E-11,-140.820483118095,
8.16439679232146));
#16539=CARTESIAN_POINT('Ctrl Pts',(4.71371668583241,-140.645483118095,8.16439679231297));
#16540=CARTESIAN_POINT('Ctrl Pts',(7.07057502873392,-140.470483118095,4.082198396148));
#16541=CARTESIAN_POINT('Ctrl Pts',(9.42743337163542,-140.295483118095,-1.69756769845304E-11));
#16542=CARTESIAN_POINT('Ctrl Pts',(7.07057502871922,-140.120483118095,-4.08219839617346));
#16543=CARTESIAN_POINT('Ctrl Pts',(4.71371668580301,-139.945483118095,-8.16439679232994));
#16544=CARTESIAN_POINT('Ctrl Pts',(-1.4702867290402E-11,-139.770483118095,
-8.16439679232146));
#16545=CARTESIAN_POINT('Ctrl Pts',(-4.71371668583241,-139.595483118095,
-8.16439679231297));
#16546=CARTESIAN_POINT('Ctrl Pts',(-7.07057502873392,-139.420483118095,
-4.082198396148));
#16547=CARTESIAN_POINT('Ctrl Pts',(-9.42743337163542,-139.245483118095,
1.69768315121407E-11));
#16548=CARTESIAN_POINT('Ctrl Pts',(-7.07057502871922,-139.070483118095,
4.08219839617346));
#16549=CARTESIAN_POINT('Ctrl Pts',(-4.71371668580301,-138.895483118095,
8.16439679232994));
#16550=CARTESIAN_POINT('Ctrl Pts',(1.47018674401621E-11,-138.720483118095,
8.16439679232146));
#16551=CARTESIAN_POINT('Ctrl Pts',(4.71371668583241,-138.545483118095,8.16439679231297));
#16552=CARTESIAN_POINT('Ctrl Pts',(7.07057502873392,-138.370483118095,4.082198396148));
#16553=CARTESIAN_POINT('Ctrl Pts',(9.42743337163542,-138.195483118095,-1.69756769845304E-11));
#16554=CARTESIAN_POINT('Ctrl Pts',(7.07057502871922,-138.020483118095,-4.08219839617346));
#16555=CARTESIAN_POINT('Ctrl Pts',(4.71371668580301,-137.845483118095,-8.16439679232994));
#16556=CARTESIAN_POINT('Ctrl Pts',(-1.4702867290402E-11,-137.670483118095,
-8.16439679232146));
#16557=CARTESIAN_POINT('Ctrl Pts',(-4.71371668583241,-137.495483118095,
-8.16439679231297));
#16558=CARTESIAN_POINT('Ctrl Pts',(-7.07057502873392,-137.320483118095,
-4.082198396148));
#16559=CARTESIAN_POINT('Ctrl Pts',(-9.42743337163542,-137.145483118095,
1.69768315121407E-11));
#16560=CARTESIAN_POINT('Ctrl Pts',(-7.07057502871922,-136.970483118095,
4.08219839617346));
#16561=CARTESIAN_POINT('Ctrl Pts',(-4.71371668580301,-136.795483118095,
8.16439679232994));
#16562=CARTESIAN_POINT('Ctrl Pts',(1.47018674401621E-11,-136.620483118095,
8.16439679232146));
#16563=CARTESIAN_POINT('Ctrl Pts',(4.71371668583241,-136.445483118095,8.16439679231297));
#16564=CARTESIAN_POINT('Ctrl Pts',(7.07057502873392,-136.270483118095,4.082198396148));
#16565=CARTESIAN_POINT('Ctrl Pts',(9.42743337163542,-136.095483118095,-1.69756769845304E-11));
#16566=CARTESIAN_POINT('Ctrl Pts',(7.07057502871922,-135.920483118095,-4.08219839617346));
#16567=CARTESIAN_POINT('Ctrl Pts',(4.71371668580301,-135.745483118095,-8.16439679232994));
#16568=CARTESIAN_POINT('Ctrl Pts',(-1.4702867290402E-11,-135.570483118095,
-8.16439679232146));
#16569=CARTESIAN_POINT('Ctrl Pts',(-4.71371668583241,-135.395483118095,
-8.16439679231297));
#16570=CARTESIAN_POINT('Ctrl Pts',(-7.07057502873392,-135.220483118095,
-4.082198396148));
#16571=CARTESIAN_POINT('Ctrl Pts',(-9.42743337163542,-135.045483118095,
1.69768315121407E-11));
#16572=CARTESIAN_POINT('Ctrl Pts',(-7.07057502871922,-134.870483118095,
4.08219839617346));
#16573=CARTESIAN_POINT('Ctrl Pts',(-4.71371668580301,-134.695483118095,
8.16439679232994));
#16574=CARTESIAN_POINT('Ctrl Pts',(1.47018674401621E-11,-134.520483118095,
8.16439679232146));
#16575=CARTESIAN_POINT('Ctrl Pts',(4.71371668583241,-134.345483118095,8.16439679231297));
#16576=CARTESIAN_POINT('Ctrl Pts',(7.07057502873392,-134.170483118095,4.082198396148));
#16577=CARTESIAN_POINT('Ctrl Pts',(9.42743337163542,-133.995483118095,-1.69756769845304E-11));
#16578=CARTESIAN_POINT('Ctrl Pts',(7.07057502871922,-133.820483118095,-4.08219839617346));
#16579=CARTESIAN_POINT('Ctrl Pts',(4.71371668580301,-133.645483118095,-8.16439679232994));
#16580=CARTESIAN_POINT('Ctrl Pts',(-1.4702867290402E-11,-133.470483118095,
-8.16439679232146));
#16581=CARTESIAN_POINT('Ctrl Pts',(-4.71371668583241,-133.295483118095,
-8.16439679231297));
#16582=CARTESIAN_POINT('Ctrl Pts',(-7.07057502873392,-133.120483118095,
-4.082198396148));
#16583=CARTESIAN_POINT('Ctrl Pts',(-9.42743337163542,-132.945483118095,
1.69768315121407E-11));
#16584=CARTESIAN_POINT('Ctrl Pts',(-7.07057502871922,-132.770483118095,
4.08219839617346));
#16585=CARTESIAN_POINT('Ctrl Pts',(-4.71371668580301,-132.595483118095,
8.16439679232994));
#16586=CARTESIAN_POINT('Ctrl Pts',(1.47018674401621E-11,-132.420483118095,
8.16439679232146));
#16587=CARTESIAN_POINT('Ctrl Pts',(4.71371668583241,-132.245483118095,8.16439679231297));
#16588=CARTESIAN_POINT('Ctrl Pts',(7.07057502873392,-132.070483118095,4.082198396148));
#16589=CARTESIAN_POINT('Ctrl Pts',(9.42743337163542,-131.895483118095,-1.69756769845304E-11));
#16590=CARTESIAN_POINT('Ctrl Pts',(7.07057502871922,-131.720483118095,-4.08219839617346));
#16591=CARTESIAN_POINT('Ctrl Pts',(4.71371668580301,-131.545483118095,-8.16439679232994));
#16592=CARTESIAN_POINT('Ctrl Pts',(-1.4702867290402E-11,-131.370483118095,
-8.16439679232146));
#16593=CARTESIAN_POINT('Ctrl Pts',(-4.71371668583241,-131.195483118095,
-8.16439679231297));
#16594=CARTESIAN_POINT('Ctrl Pts',(-7.07057502873392,-131.020483118095,
-4.082198396148));
#16595=CARTESIAN_POINT('Ctrl Pts',(-9.42743337163542,-130.845483118095,
1.69768315121407E-11));
#16596=CARTESIAN_POINT('Ctrl Pts',(-7.07057502871922,-130.670483118095,
4.08219839617346));
#16597=CARTESIAN_POINT('Ctrl Pts',(-4.71371668580301,-130.495483118095,
8.16439679232994));
#16598=CARTESIAN_POINT('Ctrl Pts',(1.47018674401621E-11,-130.320483118095,
8.16439679232146));
#16599=CARTESIAN_POINT('Ctrl Pts',(4.71371668583241,-130.145483118095,8.16439679231297));
#16600=CARTESIAN_POINT('Ctrl Pts',(7.07057502873392,-129.970483118095,4.082198396148));
#16601=CARTESIAN_POINT('Ctrl Pts',(9.42743337163542,-129.795483118095,-1.69756769845304E-11));
#16602=CARTESIAN_POINT('Ctrl Pts',(7.07057502871922,-129.620483118095,-4.08219839617346));
#16603=CARTESIAN_POINT('Ctrl Pts',(4.71371668580301,-129.445483118095,-8.16439679232994));
#16604=CARTESIAN_POINT('Ctrl Pts',(-1.4702867290402E-11,-129.270483118095,
-8.16439679232146));
#16605=CARTESIAN_POINT('Ctrl Pts',(-4.71371668583241,-129.095483118095,
-8.16439679231297));
#16606=CARTESIAN_POINT('Ctrl Pts',(-7.07057502873392,-128.920483118095,
-4.082198396148));
#16607=CARTESIAN_POINT('Ctrl Pts',(-9.42743337163542,-128.745483118095,
1.69768315121407E-11));
#16608=CARTESIAN_POINT('Ctrl Pts',(-7.07057502871922,-128.570483118095,
4.08219839617346));
#16609=CARTESIAN_POINT('Ctrl Pts',(-4.71371668580301,-128.395483118095,
8.16439679232994));
#16610=CARTESIAN_POINT('Ctrl Pts',(1.47018674401621E-11,-128.220483118095,
8.16439679232146));
#16611=CARTESIAN_POINT('Ctrl Pts',(4.71371668583241,-128.045483118095,8.16439679231297));
#16612=CARTESIAN_POINT('Ctrl Pts',(7.07057502873392,-127.870483118095,4.082198396148));
#16613=CARTESIAN_POINT('Ctrl Pts',(9.42743337163542,-127.695483118095,-1.69756769845304E-11));
#16614=CARTESIAN_POINT('Ctrl Pts',(7.07057502871922,-127.520483118095,-4.08219839617346));
#16615=CARTESIAN_POINT('Ctrl Pts',(4.71371668580301,-127.345483118095,-8.16439679232994));
#16616=CARTESIAN_POINT('Ctrl Pts',(-1.4702867290402E-11,-127.170483118095,
-8.16439679232146));
#16617=CARTESIAN_POINT('Ctrl Pts',(-4.71371668583241,-126.995483118095,
-8.16439679231297));
#16618=CARTESIAN_POINT('Ctrl Pts',(-7.07057502873392,-126.820483118095,
-4.082198396148));
#16619=CARTESIAN_POINT('Ctrl Pts',(-9.42743337163542,-126.645483118095,
1.69768315121407E-11));
#16620=CARTESIAN_POINT('Ctrl Pts',(-7.07057502871922,-126.470483118095,
4.08219839617346));
#16621=CARTESIAN_POINT('Ctrl Pts',(-4.71371668580301,-126.295483118095,
8.16439679232994));
#16622=CARTESIAN_POINT('Ctrl Pts',(1.47018674401621E-11,-126.120483118095,
8.16439679232146));
#16623=CARTESIAN_POINT('Ctrl Pts',(4.71371668583241,-125.945483118095,8.16439679231297));
#16624=CARTESIAN_POINT('Ctrl Pts',(7.07057502873392,-125.770483118095,4.082198396148));
#16625=CARTESIAN_POINT('Ctrl Pts',(9.42743337163542,-125.595483118095,-1.69756769845304E-11));
#16626=CARTESIAN_POINT('Ctrl Pts',(7.07057502871922,-125.420483118095,-4.08219839617346));
#16627=CARTESIAN_POINT('Ctrl Pts',(4.71371668580301,-125.245483118095,-8.16439679232994));
#16628=CARTESIAN_POINT('Ctrl Pts',(-1.4702867290402E-11,-125.070483118095,
-8.16439679232146));
#16629=CARTESIAN_POINT('Ctrl Pts',(-4.71371668583241,-124.895483118095,
-8.16439679231297));
#16630=CARTESIAN_POINT('Ctrl Pts',(-7.07057502873392,-124.720483118095,
-4.082198396148));
#16631=CARTESIAN_POINT('Ctrl Pts',(-9.42743337163542,-124.545483118095,
1.69768315121407E-11));
#16632=CARTESIAN_POINT('Ctrl Pts',(-7.07057502871922,-124.370483118095,
4.08219839617346));
#16633=CARTESIAN_POINT('Ctrl Pts',(-4.71371668580301,-124.195483118095,
8.16439679232994));
#16634=CARTESIAN_POINT('Ctrl Pts',(1.47018674401621E-11,-124.020483118095,
8.16439679232146));
#16635=CARTESIAN_POINT('Ctrl Pts',(4.71371668583241,-123.845483118095,8.16439679231297));
#16636=CARTESIAN_POINT('Ctrl Pts',(7.07057502873392,-123.670483118095,4.082198396148));
#16637=CARTESIAN_POINT('Ctrl Pts',(9.42743337163542,-123.495483118095,-1.69756769845304E-11));
#16638=CARTESIAN_POINT('Ctrl Pts',(7.07057502871922,-123.320483118095,-4.08219839617346));
#16639=CARTESIAN_POINT('Ctrl Pts',(4.71371668580301,-123.145483118095,-8.16439679232994));
#16640=CARTESIAN_POINT('Ctrl Pts',(-1.4702867290402E-11,-122.970483118095,
-8.16439679232146));
#16641=CARTESIAN_POINT('Ctrl Pts',(-4.71371668583241,-122.795483118095,
-8.16439679231297));
#16642=CARTESIAN_POINT('Ctrl Pts',(-7.07057502873392,-122.620483118095,
-4.082198396148));
#16643=CARTESIAN_POINT('Ctrl Pts',(-9.42743337163542,-122.445483118095,
1.69768315121407E-11));
#16644=CARTESIAN_POINT('Ctrl Pts',(-7.07057502871922,-122.270483118095,
4.08219839617346));
#16645=CARTESIAN_POINT('Ctrl Pts',(-4.71371668580301,-122.095483118095,
8.16439679232994));
#16646=CARTESIAN_POINT('Ctrl Pts',(1.47018674401621E-11,-121.920483118095,
8.16439679232146));
#16647=CARTESIAN_POINT('Ctrl Pts',(4.71371668583241,-121.745483118095,8.16439679231297));
#16648=CARTESIAN_POINT('Ctrl Pts',(7.07057502873392,-121.570483118095,4.082198396148));
#16649=CARTESIAN_POINT('Ctrl Pts',(9.42743337163542,-121.395483118095,-1.69756769845304E-11));
#16650=CARTESIAN_POINT('Ctrl Pts',(7.07057502871922,-121.220483118095,-4.08219839617346));
#16651=CARTESIAN_POINT('Ctrl Pts',(4.71371668580301,-121.045483118095,-8.16439679232994));
#16652=CARTESIAN_POINT('Ctrl Pts',(-1.4702867290402E-11,-120.870483118095,
-8.16439679232146));
#16653=CARTESIAN_POINT('Ctrl Pts',(-4.71371668583241,-120.695483118095,
-8.16439679231297));
#16654=CARTESIAN_POINT('Ctrl Pts',(-7.07057502873392,-120.520483118095,
-4.082198396148));
#16655=CARTESIAN_POINT('Ctrl Pts',(-9.42743337163542,-120.345483118095,
1.69768315121407E-11));
#16656=CARTESIAN_POINT('Ctrl Pts',(-7.07057502871922,-120.170483118095,
4.08219839617346));
#16657=CARTESIAN_POINT('Ctrl Pts',(-4.71371668580301,-119.995483118095,
8.16439679232994));
#16658=CARTESIAN_POINT('Ctrl Pts',(1.47018674401621E-11,-119.820483118095,
8.16439679232146));
#16659=CARTESIAN_POINT('Ctrl Pts',(4.71371668583241,-119.645483118095,8.16439679231297));
#16660=CARTESIAN_POINT('Ctrl Pts',(7.07057502873392,-119.470483118095,4.082198396148));
#16661=CARTESIAN_POINT('Ctrl Pts',(9.42743337163542,-119.295483118095,-1.69756769845304E-11));
#16662=CARTESIAN_POINT('Ctrl Pts',(7.07057502871922,-119.120483118095,-4.08219839617346));
#16663=CARTESIAN_POINT('Ctrl Pts',(4.71371668580301,-118.945483118095,-8.16439679232994));
#16664=CARTESIAN_POINT('Ctrl Pts',(-1.4702867290402E-11,-118.770483118095,
-8.16439679232146));
#16665=CARTESIAN_POINT('Ctrl Pts',(-4.71371668583241,-118.595483118095,
-8.16439679231297));
#16666=CARTESIAN_POINT('Ctrl Pts',(-7.07057502873392,-118.420483118095,
-4.082198396148));
#16667=CARTESIAN_POINT('Ctrl Pts',(-9.42743337163542,-118.245483118095,
1.69768315121407E-11));
#16668=CARTESIAN_POINT('Ctrl Pts',(-7.07057502871922,-118.070483118095,
4.08219839617346));
#16669=CARTESIAN_POINT('Ctrl Pts',(-4.71371668580301,-117.895483118095,
8.16439679232994));
#16670=CARTESIAN_POINT('Ctrl Pts',(1.47018674401621E-11,-117.720483118095,
8.16439679232146));
#16671=CARTESIAN_POINT('Ctrl Pts',(4.71371668583241,-117.545483118095,8.16439679231297));
#16672=CARTESIAN_POINT('Ctrl Pts',(7.07057502873392,-117.370483118095,4.082198396148));
#16673=CARTESIAN_POINT('Ctrl Pts',(9.42743337163542,-117.195483118095,-1.69756769845304E-11));
#16674=CARTESIAN_POINT('Ctrl Pts',(7.07057502871922,-117.020483118095,-4.08219839617346));
#16675=CARTESIAN_POINT('Ctrl Pts',(4.71371668580301,-116.845483118095,-8.16439679232994));
#16676=CARTESIAN_POINT('Ctrl Pts',(-1.4702867290402E-11,-116.670483118095,
-8.16439679232146));
#16677=CARTESIAN_POINT('Ctrl Pts',(-4.71371668583241,-116.495483118095,
-8.16439679231297));
#16678=CARTESIAN_POINT('Ctrl Pts',(-7.07057502873392,-116.320483118095,
-4.082198396148));
#16679=CARTESIAN_POINT('Ctrl Pts',(-9.42743337163542,-116.145483118095,
1.69768315121407E-11));
#16680=CARTESIAN_POINT('Ctrl Pts',(-7.07057502871922,-115.970483118095,
4.08219839617346));
#16681=CARTESIAN_POINT('Ctrl Pts',(-4.71371668580301,-115.795483118095,
8.16439679232994));
#16682=CARTESIAN_POINT('Ctrl Pts',(1.47018674401621E-11,-115.620483118095,
8.16439679232146));
#16683=CARTESIAN_POINT('Ctrl Pts',(4.71371668583241,-115.445483118095,8.16439679231297));
#16684=CARTESIAN_POINT('Ctrl Pts',(7.07057502873392,-115.270483118095,4.082198396148));
#16685=CARTESIAN_POINT('Ctrl Pts',(9.42743337163542,-115.095483118095,-1.69756769845304E-11));
#16686=CARTESIAN_POINT('Ctrl Pts',(7.07057502871922,-114.920483118095,-4.08219839617346));
#16687=CARTESIAN_POINT('Ctrl Pts',(4.71371668580301,-114.745483118095,-8.16439679232994));
#16688=CARTESIAN_POINT('Ctrl Pts',(-1.4702867290402E-11,-114.570483118095,
-8.16439679232146));
#16689=CARTESIAN_POINT('Ctrl Pts',(-4.71371668583241,-114.395483118095,
-8.16439679231297));
#16690=CARTESIAN_POINT('Ctrl Pts',(-7.07057502873392,-114.220483118095,
-4.082198396148));
#16691=CARTESIAN_POINT('Ctrl Pts',(-9.42743337163542,-114.045483118095,
1.69768315121407E-11));
#16692=CARTESIAN_POINT('Ctrl Pts',(-7.07057502871922,-113.870483118095,
4.08219839617346));
#16693=CARTESIAN_POINT('Ctrl Pts',(-4.71371668580301,-113.695483118095,
8.16439679232994));
#16694=CARTESIAN_POINT('Ctrl Pts',(1.47018674401621E-11,-113.520483118095,
8.16439679232146));
#16695=CARTESIAN_POINT('Ctrl Pts',(4.71371668583241,-113.345483118095,8.16439679231297));
#16696=CARTESIAN_POINT('Ctrl Pts',(7.07057502873392,-113.170483118095,4.082198396148));
#16697=CARTESIAN_POINT('Ctrl Pts',(9.42743337163542,-112.995483118095,-1.69756769845304E-11));
#16698=CARTESIAN_POINT('Ctrl Pts',(7.07057502871922,-112.820483118095,-4.08219839617346));
#16699=CARTESIAN_POINT('Ctrl Pts',(4.71371668580301,-112.645483118095,-8.16439679232994));
#16700=CARTESIAN_POINT('Ctrl Pts',(-1.4702867290402E-11,-112.470483118095,
-8.16439679232146));
#16701=CARTESIAN_POINT('Ctrl Pts',(-4.71371668583241,-112.295483118095,
-8.16439679231297));
#16702=CARTESIAN_POINT('Ctrl Pts',(-7.07057502873392,-112.120483118095,
-4.082198396148));
#16703=CARTESIAN_POINT('Ctrl Pts',(-9.42743337163542,-111.945483118095,
1.69768315121407E-11));
#16704=CARTESIAN_POINT('Ctrl Pts',(-7.07057502871922,-111.770483118095,
4.08219839617346));
#16705=CARTESIAN_POINT('Ctrl Pts',(-4.71371668580301,-111.595483118095,
8.16439679232994));
#16706=CARTESIAN_POINT('Ctrl Pts',(1.47018674401621E-11,-111.420483118095,
8.16439679232146));
#16707=CARTESIAN_POINT('Ctrl Pts',(4.71371668583241,-111.245483118095,8.16439679231297));
#16708=CARTESIAN_POINT('Ctrl Pts',(7.07057502873392,-111.070483118095,4.082198396148));
#16709=CARTESIAN_POINT('Ctrl Pts',(9.42743337163542,-110.895483118095,-1.69756769845304E-11));
#16710=CARTESIAN_POINT('Ctrl Pts',(7.07057502871922,-110.720483118095,-4.08219839617346));
#16711=CARTESIAN_POINT('Ctrl Pts',(4.71371668580301,-110.545483118095,-8.16439679232994));
#16712=CARTESIAN_POINT('Ctrl Pts',(-1.4702867290402E-11,-110.370483118095,
-8.16439679232146));
#16713=CARTESIAN_POINT('Ctrl Pts',(-4.71371668583241,-110.195483118095,
-8.16439679231297));
#16714=CARTESIAN_POINT('Ctrl Pts',(-7.07057502873392,-110.020483118095,
-4.082198396148));
#16715=CARTESIAN_POINT('Ctrl Pts',(-9.42743337163542,-109.845483118095,
1.69768315121407E-11));
#16716=CARTESIAN_POINT('Ctrl Pts',(-7.07057502871922,-109.670483118095,
4.08219839617346));
#16717=CARTESIAN_POINT('Ctrl Pts',(-4.71371668580301,-109.495483118095,
8.16439679232994));
#16718=CARTESIAN_POINT('Ctrl Pts',(1.47018674401621E-11,-109.320483118095,
8.16439679232146));
#16719=CARTESIAN_POINT('Ctrl Pts',(4.71371668583241,-109.145483118095,8.16439679231297));
#16720=CARTESIAN_POINT('Ctrl Pts',(7.07057502873392,-108.970483118095,4.082198396148));
#16721=CARTESIAN_POINT('Ctrl Pts',(9.42743337163542,-108.795483118095,-1.69756769845304E-11));
#16722=CARTESIAN_POINT('Ctrl Pts',(7.07057502871922,-108.620483118095,-4.08219839617346));
#16723=CARTESIAN_POINT('Ctrl Pts',(4.71371668580301,-108.445483118095,-8.16439679232994));
#16724=CARTESIAN_POINT('Ctrl Pts',(-1.4702867290402E-11,-108.270483118095,
-8.16439679232146));
#16725=CARTESIAN_POINT('Ctrl Pts',(-4.71371668583241,-108.095483118095,
-8.16439679231297));
#16726=CARTESIAN_POINT('Ctrl Pts',(-7.07057502873392,-107.920483118095,
-4.082198396148));
#16727=CARTESIAN_POINT('Ctrl Pts',(-9.42743337163542,-107.745483118095,
1.69768315121407E-11));
#16728=CARTESIAN_POINT('Ctrl Pts',(-7.07057502871922,-107.570483118095,
4.08219839617346));
#16729=CARTESIAN_POINT('Ctrl Pts',(-4.71371668580301,-107.395483118095,
8.16439679232994));
#16730=CARTESIAN_POINT('Ctrl Pts',(1.47018674401621E-11,-107.220483118095,
8.16439679232146));
#16731=CARTESIAN_POINT('Ctrl Pts',(4.71371668583241,-107.045483118095,8.16439679231297));
#16732=CARTESIAN_POINT('Ctrl Pts',(7.07057502873392,-106.870483118095,4.082198396148));
#16733=CARTESIAN_POINT('Ctrl Pts',(9.42743337163542,-106.695483118095,-1.69756769845304E-11));
#16734=CARTESIAN_POINT('Ctrl Pts',(7.07057502871922,-106.520483118095,-4.08219839617346));
#16735=CARTESIAN_POINT('Ctrl Pts',(4.71371668580301,-106.345483118095,-8.16439679232994));
#16736=CARTESIAN_POINT('Ctrl Pts',(-1.4702867290402E-11,-106.170483118095,
-8.16439679232146));
#16737=CARTESIAN_POINT('Ctrl Pts',(-4.71371668583241,-105.995483118095,
-8.16439679231297));
#16738=CARTESIAN_POINT('Ctrl Pts',(-7.07057502873392,-105.820483118095,
-4.082198396148));
#16739=CARTESIAN_POINT('Ctrl Pts',(-9.42743337163542,-105.645483118095,
1.69768315121407E-11));
#16740=CARTESIAN_POINT('Ctrl Pts',(-7.07057502871922,-105.470483118095,
4.08219839617346));
#16741=CARTESIAN_POINT('Ctrl Pts',(-4.71371668580301,-105.295483118095,
8.16439679232994));
#16742=CARTESIAN_POINT('Ctrl Pts',(1.47018674401621E-11,-105.120483118095,
8.16439679232146));
#16743=CARTESIAN_POINT('Ctrl Pts',(4.71371668583241,-104.945483118095,8.16439679231297));
#16744=CARTESIAN_POINT('Ctrl Pts',(7.07057502873392,-104.770483118095,4.082198396148));
#16745=CARTESIAN_POINT('Ctrl Pts',(9.42743337163542,-104.595483118095,-1.69756769845304E-11));
#16746=CARTESIAN_POINT('Ctrl Pts',(7.07057502871922,-104.420483118095,-4.08219839617346));
#16747=CARTESIAN_POINT('Ctrl Pts',(4.71371668580301,-104.245483118095,-8.16439679232994));
#16748=CARTESIAN_POINT('Ctrl Pts',(-1.4702867290402E-11,-104.070483118095,
-8.16439679232146));
#16749=CARTESIAN_POINT('Ctrl Pts',(-4.71371668583241,-103.895483118095,
-8.16439679231297));
#16750=CARTESIAN_POINT('Ctrl Pts',(-7.07057502873392,-103.720483118095,
-4.082198396148));
#16751=CARTESIAN_POINT('Ctrl Pts',(-9.42743337163542,-103.545483118095,
1.69768315121407E-11));
#16752=CARTESIAN_POINT('Ctrl Pts',(-7.07057502871922,-103.370483118095,
4.08219839617346));
#16753=CARTESIAN_POINT('Ctrl Pts',(-4.71371668580301,-103.195483118095,
8.16439679232994));
#16754=CARTESIAN_POINT('Ctrl Pts',(1.47018674401621E-11,-103.020483118095,
8.16439679232146));
#16755=CARTESIAN_POINT('Ctrl Pts',(4.71371668583241,-102.845483118095,8.16439679231297));
#16756=CARTESIAN_POINT('Ctrl Pts',(7.07057502873392,-102.670483118095,4.082198396148));
#16757=CARTESIAN_POINT('Ctrl Pts',(9.42743337163542,-102.495483118095,-1.69756769845304E-11));
#16758=CARTESIAN_POINT('Ctrl Pts',(7.07057502871922,-102.320483118095,-4.08219839617346));
#16759=CARTESIAN_POINT('Ctrl Pts',(4.71371668580301,-102.145483118095,-8.16439679232994));
#16760=CARTESIAN_POINT('Ctrl Pts',(-1.4702867290402E-11,-101.970483118095,
-8.16439679232146));
#16761=CARTESIAN_POINT('Ctrl Pts',(-4.71371668583241,-101.795483118095,
-8.16439679231297));
#16762=CARTESIAN_POINT('Ctrl Pts',(-7.07057502873392,-101.620483118095,
-4.082198396148));
#16763=CARTESIAN_POINT('Ctrl Pts',(-9.42743337163542,-101.445483118095,
1.69768315121407E-11));
#16764=CARTESIAN_POINT('Ctrl Pts',(-7.07057502871922,-101.270483118095,
4.08219839617346));
#16765=CARTESIAN_POINT('Ctrl Pts',(-4.71371668580301,-101.095483118095,
8.16439679232994));
#16766=CARTESIAN_POINT('Ctrl Pts',(1.47018674401621E-11,-100.920483118095,
8.16439679232146));
#16767=CARTESIAN_POINT('Ctrl Pts',(4.71371668583241,-100.745483118095,8.16439679231297));
#16768=CARTESIAN_POINT('Ctrl Pts',(7.07057502873392,-100.570483118095,4.082198396148));
#16769=CARTESIAN_POINT('Ctrl Pts',(9.42743337163542,-100.395483118095,-1.69756769845304E-11));
#16770=CARTESIAN_POINT('Ctrl Pts',(7.07057502871922,-100.220483118095,-4.08219839617346));
#16771=CARTESIAN_POINT('Ctrl Pts',(4.71371668580301,-100.045483118095,-8.16439679232994));
#16772=CARTESIAN_POINT('Ctrl Pts',(-1.4702867290402E-11,-99.8704831180952,
-8.16439679232146));
#16773=CARTESIAN_POINT('Ctrl Pts',(-4.71371668583241,-99.6954831180952,
-8.16439679231297));
#16774=CARTESIAN_POINT('Ctrl Pts',(-7.07057502873392,-99.5204831180952,
-4.082198396148));
#16775=CARTESIAN_POINT('Ctrl Pts',(-9.42743337163542,-99.3454831180952,
1.69768315121407E-11));
#16776=CARTESIAN_POINT('Ctrl Pts',(-7.07057502871922,-99.1704831180952,
4.08219839617346));
#16777=CARTESIAN_POINT('Ctrl Pts',(-4.71371668580301,-98.9954831180952,
8.16439679232994));
#16778=CARTESIAN_POINT('Ctrl Pts',(1.47018674401621E-11,-98.8204831180952,
8.16439679232146));
#16779=CARTESIAN_POINT('Ctrl Pts',(4.71371668583241,-98.6454831180952,8.16439679231297));
#16780=CARTESIAN_POINT('Ctrl Pts',(7.07057502873392,-98.4704831180952,4.082198396148));
#16781=CARTESIAN_POINT('Ctrl Pts',(9.42743337163542,-98.2954831180952,-1.69756769845304E-11));
#16782=CARTESIAN_POINT('Ctrl Pts',(7.07057502871922,-98.1204831180952,-4.08219839617346));
#16783=CARTESIAN_POINT('Ctrl Pts',(4.71371668580301,-97.9454831180952,-8.16439679232994));
#16784=CARTESIAN_POINT('Ctrl Pts',(-1.4702867290402E-11,-97.7704831180952,
-8.16439679232146));
#16785=CARTESIAN_POINT('Ctrl Pts',(-4.71371668583241,-97.5954831180952,
-8.16439679231297));
#16786=CARTESIAN_POINT('Ctrl Pts',(-7.07057502873392,-97.4204831180952,
-4.082198396148));
#16787=CARTESIAN_POINT('Ctrl Pts',(-9.42743337163542,-97.2454831180952,
1.69768315121407E-11));
#16788=CARTESIAN_POINT('Ctrl Pts',(-7.07057502871922,-97.0704831180952,
4.08219839617346));
#16789=CARTESIAN_POINT('Ctrl Pts',(-4.71371668580301,-96.8954831180952,
8.16439679232994));
#16790=CARTESIAN_POINT('Ctrl Pts',(1.47018674401621E-11,-96.7204831180952,
8.16439679232146));
#16791=CARTESIAN_POINT('Ctrl Pts',(4.71371668583241,-96.5454831180952,8.16439679231297));
#16792=CARTESIAN_POINT('Ctrl Pts',(7.07057502873392,-96.3704831180952,4.082198396148));
#16793=CARTESIAN_POINT('Ctrl Pts',(9.42743337163542,-96.1954831180952,-1.69756769845304E-11));
#16794=CARTESIAN_POINT('Ctrl Pts',(7.07057502871922,-96.0204831180952,-4.08219839617346));
#16795=CARTESIAN_POINT('Ctrl Pts',(4.71371668580301,-95.8454831180952,-8.16439679232994));
#16796=CARTESIAN_POINT('Ctrl Pts',(-1.4702867290402E-11,-95.6704831180952,
-8.16439679232146));
#16797=CARTESIAN_POINT('Ctrl Pts',(-4.71371668583241,-95.4954831180952,
-8.16439679231297));
#16798=CARTESIAN_POINT('Ctrl Pts',(-7.07057502873392,-95.3204831180952,
-4.082198396148));
#16799=CARTESIAN_POINT('Ctrl Pts',(-9.42743337163542,-95.1454831180952,
1.69768315121407E-11));
#16800=CARTESIAN_POINT('Ctrl Pts',(-7.07057502871922,-94.9704831180952,
4.08219839617346));
#16801=CARTESIAN_POINT('Ctrl Pts',(-4.71371668580301,-94.7954831180952,
8.16439679232994));
#16802=CARTESIAN_POINT('Ctrl Pts',(1.47018674401621E-11,-94.6204831180952,
8.16439679232146));
#16803=CARTESIAN_POINT('Ctrl Pts',(4.71371668583241,-94.4454831180952,8.16439679231297));
#16804=CARTESIAN_POINT('Ctrl Pts',(7.07057502873392,-94.2704831180952,4.082198396148));
#16805=CARTESIAN_POINT('Ctrl Pts',(9.42743337163542,-94.0954831180952,-1.69756769845304E-11));
#16806=CARTESIAN_POINT('Ctrl Pts',(7.07057502871922,-93.9204831180952,-4.08219839617346));
#16807=CARTESIAN_POINT('Ctrl Pts',(4.71371668580301,-93.7454831180952,-8.16439679232994));
#16808=CARTESIAN_POINT('Ctrl Pts',(-1.4702867290402E-11,-93.5704831180952,
-8.16439679232146));
#16809=CARTESIAN_POINT('Ctrl Pts',(-4.71371668583241,-93.3954831180952,
-8.16439679231297));
#16810=CARTESIAN_POINT('Ctrl Pts',(-7.07057502873392,-93.2204831180952,
-4.082198396148));
#16811=CARTESIAN_POINT('Ctrl Pts',(-9.42743337163542,-93.0454831180952,
1.69768315121407E-11));
#16812=CARTESIAN_POINT('Ctrl Pts',(-7.07057502871922,-92.8704831180952,
4.08219839617346));
#16813=CARTESIAN_POINT('Ctrl Pts',(-4.71371668580301,-92.6954831180952,
8.16439679232994));
#16814=CARTESIAN_POINT('Ctrl Pts',(1.47018674401621E-11,-92.5204831180952,
8.16439679232146));
#16815=CARTESIAN_POINT('Ctrl Pts',(4.71371668583241,-92.3454831180952,8.16439679231297));
#16816=CARTESIAN_POINT('Ctrl Pts',(7.07057502873392,-92.1704831180952,4.082198396148));
#16817=CARTESIAN_POINT('Ctrl Pts',(9.42743337163542,-91.9954831180952,-1.69756769845304E-11));
#16818=CARTESIAN_POINT('Ctrl Pts',(7.07057502871922,-91.8204831180952,-4.08219839617346));
#16819=CARTESIAN_POINT('Ctrl Pts',(4.71371668580301,-91.6454831180952,-8.16439679232994));
#16820=CARTESIAN_POINT('Ctrl Pts',(-1.4702867290402E-11,-91.4704831180952,
-8.16439679232146));
#16821=CARTESIAN_POINT('Ctrl Pts',(-4.71371668583241,-91.2954831180952,
-8.16439679231297));
#16822=CARTESIAN_POINT('Ctrl Pts',(-7.07057502873392,-91.1204831180952,
-4.082198396148));
#16823=CARTESIAN_POINT('Ctrl Pts',(-9.42743337163542,-90.9454831180952,
1.69768315121407E-11));
#16824=CARTESIAN_POINT('Ctrl Pts',(-7.07057502871922,-90.7704831180952,
4.08219839617346));
#16825=CARTESIAN_POINT('Ctrl Pts',(-4.71371668580301,-90.5954831180952,
8.16439679232994));
#16826=CARTESIAN_POINT('Ctrl Pts',(1.47018674401621E-11,-90.4204831180952,
8.16439679232146));
#16827=CARTESIAN_POINT('Ctrl Pts',(4.71371668583241,-90.2454831180952,8.16439679231297));
#16828=CARTESIAN_POINT('Ctrl Pts',(7.07057502873392,-90.0704831180952,4.082198396148));
#16829=CARTESIAN_POINT('Ctrl Pts',(9.42743337163542,-89.8954831180952,-1.69756769845304E-11));
#16830=CARTESIAN_POINT('Ctrl Pts',(7.07057502871922,-89.7204831180952,-4.08219839617346));
#16831=CARTESIAN_POINT('Ctrl Pts',(4.71371668580301,-89.5454831180952,-8.16439679232994));
#16832=CARTESIAN_POINT('Ctrl Pts',(-1.4702867290402E-11,-89.3704831180952,
-8.16439679232146));
#16833=CARTESIAN_POINT('Ctrl Pts',(-4.71371668583241,-89.1954831180952,
-8.16439679231297));
#16834=CARTESIAN_POINT('Ctrl Pts',(-7.07057502873392,-89.0204831180952,
-4.082198396148));
#16835=CARTESIAN_POINT('Ctrl Pts',(-9.42743337163542,-88.8454831180952,
1.69768315121407E-11));
#16836=CARTESIAN_POINT('Ctrl Pts',(-7.07057502871922,-88.6704831180952,
4.08219839617346));
#16837=CARTESIAN_POINT('Ctrl Pts',(-4.71371668580301,-88.4954831180952,
8.16439679232994));
#16838=CARTESIAN_POINT('Ctrl Pts',(1.47018674401621E-11,-88.3204831180952,
8.16439679232146));
#16839=CARTESIAN_POINT('Ctrl Pts',(4.71371668583241,-88.1454831180952,8.16439679231297));
#16840=CARTESIAN_POINT('Ctrl Pts',(7.07057502873392,-87.9704831180952,4.082198396148));
#16841=CARTESIAN_POINT('Ctrl Pts',(9.42743337163542,-87.7954831180952,-1.69756769845304E-11));
#16842=CARTESIAN_POINT('Ctrl Pts',(7.07057502871922,-87.6204831180952,-4.08219839617346));
#16843=CARTESIAN_POINT('Ctrl Pts',(4.71371668580301,-87.4454831180952,-8.16439679232994));
#16844=CARTESIAN_POINT('Ctrl Pts',(-1.4702867290402E-11,-87.2704831180952,
-8.16439679232146));
#16845=CARTESIAN_POINT('Ctrl Pts',(-4.71371668583241,-87.0954831180952,
-8.16439679231297));
#16846=CARTESIAN_POINT('Ctrl Pts',(-7.07057502873392,-86.9204831180952,
-4.082198396148));
#16847=CARTESIAN_POINT('Ctrl Pts',(-9.42743337163542,-86.7454831180952,
1.69768315121407E-11));
#16848=CARTESIAN_POINT('Ctrl Pts',(-7.07057502871922,-86.5704831180952,
4.08219839617346));
#16849=CARTESIAN_POINT('Ctrl Pts',(-4.71371668580301,-86.3954831180952,
8.16439679232994));
#16850=CARTESIAN_POINT('Ctrl Pts',(1.47018674401621E-11,-86.2204831180952,
8.16439679232146));
#16851=CARTESIAN_POINT('Ctrl Pts',(4.71371668583241,-86.0454831180952,8.16439679231297));
#16852=CARTESIAN_POINT('Ctrl Pts',(7.07057502873392,-85.8704831180952,4.082198396148));
#16853=CARTESIAN_POINT('Ctrl Pts',(9.42743337163542,-85.6954831180952,-1.69756769845304E-11));
#16854=CARTESIAN_POINT('Ctrl Pts',(7.07057502871922,-85.5204831180952,-4.08219839617346));
#16855=CARTESIAN_POINT('Ctrl Pts',(4.71371668580301,-85.3454831180952,-8.16439679232994));
#16856=CARTESIAN_POINT('Ctrl Pts',(-1.4702867290402E-11,-85.1704831180952,
-8.16439679232146));
#16857=CARTESIAN_POINT('Ctrl Pts',(-4.71371668583241,-84.9954831180952,
-8.16439679231297));
#16858=CARTESIAN_POINT('Ctrl Pts',(-7.07057502873392,-84.8204831180952,
-4.082198396148));
#16859=CARTESIAN_POINT('Ctrl Pts',(-9.42743337163542,-84.6454831180952,
1.69768315121407E-11));
#16860=CARTESIAN_POINT('Ctrl Pts',(-7.07057502871922,-84.4704831180952,
4.08219839617346));
#16861=CARTESIAN_POINT('Ctrl Pts',(-4.71371668580301,-84.2954831180952,
8.16439679232994));
#16862=CARTESIAN_POINT('Ctrl Pts',(1.47018674401621E-11,-84.1204831180952,
8.16439679232146));
#16863=CARTESIAN_POINT('Ctrl Pts',(4.71371668583241,-83.9454831180952,8.16439679231297));
#16864=CARTESIAN_POINT('Ctrl Pts',(7.07057502873392,-83.7704831180952,4.082198396148));
#16865=CARTESIAN_POINT('Ctrl Pts',(9.42743337163542,-83.5954831180952,-1.69756769845304E-11));
#16866=CARTESIAN_POINT('Ctrl Pts',(7.07057502871922,-83.4204831180952,-4.08219839617346));
#16867=CARTESIAN_POINT('Ctrl Pts',(4.71371668580301,-83.2454831180952,-8.16439679232994));
#16868=CARTESIAN_POINT('Ctrl Pts',(-1.4702867290402E-11,-83.0704831180952,
-8.16439679232146));
#16869=CARTESIAN_POINT('Ctrl Pts',(-4.71371668583241,-82.8954831180952,
-8.16439679231297));
#16870=CARTESIAN_POINT('Ctrl Pts',(-7.07057502873392,-82.7204831180952,
-4.082198396148));
#16871=CARTESIAN_POINT('Ctrl Pts',(-9.42743337163542,-82.5454831180952,
1.69768315121407E-11));
#16872=CARTESIAN_POINT('Ctrl Pts',(-7.07057502871922,-82.3704831180952,
4.08219839617346));
#16873=CARTESIAN_POINT('Ctrl Pts',(-4.71371668580301,-82.1954831180952,
8.16439679232994));
#16874=CARTESIAN_POINT('Ctrl Pts',(1.47018674401621E-11,-82.0204831180952,
8.16439679232146));
#16875=CARTESIAN_POINT('Ctrl Pts',(4.71371668583241,-81.8454831180952,8.16439679231297));
#16876=CARTESIAN_POINT('Ctrl Pts',(7.07057502873392,-81.6704831180952,4.082198396148));
#16877=CARTESIAN_POINT('Ctrl Pts',(9.42743337163542,-81.4954831180952,-1.69756769845304E-11));
#16878=CARTESIAN_POINT('Ctrl Pts',(7.07057502871922,-81.3204831180952,-4.08219839617346));
#16879=CARTESIAN_POINT('Ctrl Pts',(4.71371668580301,-81.1454831180953,-8.16439679232994));
#16880=CARTESIAN_POINT('Ctrl Pts',(-1.4702867290402E-11,-80.9704831180952,
-8.16439679232146));
#16881=CARTESIAN_POINT('Ctrl Pts',(-4.71371668583241,-80.7954831180952,
-8.16439679231297));
#16882=CARTESIAN_POINT('Ctrl Pts',(-7.07057502873392,-80.6204831180952,
-4.082198396148));
#16883=CARTESIAN_POINT('Ctrl Pts',(-9.42743337163542,-80.4454831180952,
1.69768315121407E-11));
#16884=CARTESIAN_POINT('Ctrl Pts',(-7.07057502871922,-80.2704831180952,
4.08219839617346));
#16885=CARTESIAN_POINT('Ctrl Pts',(-4.71371668580301,-80.0954831180952,
8.16439679232994));
#16886=CARTESIAN_POINT('Ctrl Pts',(1.47018674401621E-11,-79.9204831180952,
8.16439679232146));
#16887=CARTESIAN_POINT('Ctrl Pts',(4.71371668583241,-79.7454831180953,8.16439679231297));
#16888=CARTESIAN_POINT('Ctrl Pts',(7.07057502873392,-79.5704831180952,4.082198396148));
#16889=CARTESIAN_POINT('Ctrl Pts',(9.42743337163542,-79.3954831180952,-1.69756769845304E-11));
#16890=CARTESIAN_POINT('Ctrl Pts',(7.07057502871922,-79.2204831180952,-4.08219839617346));
#16891=CARTESIAN_POINT('Ctrl Pts',(4.71371668580301,-79.0454831180952,-8.16439679232994));
#16892=CARTESIAN_POINT('Ctrl Pts',(-1.4702867290402E-11,-78.8704831180952,
-8.16439679232146));
#16893=CARTESIAN_POINT('Ctrl Pts',(-4.71371668583241,-78.6954831180953,
-8.16439679231297));
#16894=CARTESIAN_POINT('Ctrl Pts',(-7.07057502873392,-78.5204831180952,
-4.082198396148));
#16895=CARTESIAN_POINT('Ctrl Pts',(-9.42743337163542,-78.3454831180952,
1.69768315121407E-11));
#16896=CARTESIAN_POINT('Ctrl Pts',(-7.07057502871922,-78.1704831180953,
4.08219839617346));
#16897=CARTESIAN_POINT('Ctrl Pts',(-4.71371668580301,-77.9954831180953,
8.16439679232994));
#16898=CARTESIAN_POINT('Ctrl Pts',(1.47018674401621E-11,-77.8204831180952,
8.16439679232146));
#16899=CARTESIAN_POINT('Ctrl Pts',(4.71371668583241,-77.6454831180953,8.16439679231297));
#16900=CARTESIAN_POINT('Ctrl Pts',(7.07057502873392,-77.4704831180952,4.082198396148));
#16901=CARTESIAN_POINT('Ctrl Pts',(9.42743337163542,-77.2954831180952,-1.69756769845304E-11));
#16902=CARTESIAN_POINT('Ctrl Pts',(7.07057502871922,-77.1204831180952,-4.08219839617346));
#16903=CARTESIAN_POINT('Ctrl Pts',(4.71371668580301,-76.9454831180952,-8.16439679232994));
#16904=CARTESIAN_POINT('Ctrl Pts',(-1.4702867290402E-11,-76.7704831180952,
-8.16439679232146));
#16905=CARTESIAN_POINT('Ctrl Pts',(-4.71371668583241,-76.5954831180953,
-8.16439679231297));
#16906=CARTESIAN_POINT('Ctrl Pts',(-7.07057502873392,-76.4204831180952,
-4.082198396148));
#16907=CARTESIAN_POINT('Ctrl Pts',(-9.42743337163542,-76.2454831180952,
1.69768315121407E-11));
#16908=CARTESIAN_POINT('Ctrl Pts',(-7.07057502871922,-76.0704831180952,
4.08219839617346));
#16909=CARTESIAN_POINT('Ctrl Pts',(-4.71371668580301,-75.8954831180952,
8.16439679232994));
#16910=CARTESIAN_POINT('Ctrl Pts',(1.47018674401621E-11,-75.7204831180952,
8.16439679232146));
#16911=CARTESIAN_POINT('Ctrl Pts',(4.71371668583241,-75.5454831180952,8.16439679231297));
#16912=CARTESIAN_POINT('Ctrl Pts',(7.07057502873392,-75.3704831180952,4.082198396148));
#16913=CARTESIAN_POINT('Ctrl Pts',(9.42743337163542,-75.1954831180952,-1.69756769845304E-11));
#16914=CARTESIAN_POINT('Ctrl Pts',(7.07057502871922,-75.0204831180952,-4.08219839617346));
#16915=CARTESIAN_POINT('Ctrl Pts',(4.71371668580301,-74.8454831180952,-8.16439679232994));
#16916=CARTESIAN_POINT('Ctrl Pts',(-1.4702867290402E-11,-74.6704831180952,
-8.16439679232146));
#16917=CARTESIAN_POINT('Ctrl Pts',(-4.71371668583241,-74.4954831180953,
-8.16439679231297));
#16918=CARTESIAN_POINT('Ctrl Pts',(-7.07057502873392,-74.3204831180952,
-4.082198396148));
#16919=CARTESIAN_POINT('Ctrl Pts',(-9.42743337163542,-74.1454831180952,
1.69768315121407E-11));
#16920=CARTESIAN_POINT('Ctrl Pts',(-7.07057502871922,-73.9704831180952,
4.08219839617346));
#16921=CARTESIAN_POINT('Ctrl Pts',(-4.71371668580301,-73.7954831180952,
8.16439679232994));
#16922=CARTESIAN_POINT('Ctrl Pts',(1.47018674401621E-11,-73.6204831180952,
8.16439679232146));
#16923=CARTESIAN_POINT('Ctrl Pts',(4.71371668583241,-73.4454831180953,8.16439679231297));
#16924=CARTESIAN_POINT('Ctrl Pts',(7.07057502873392,-73.2704831180952,4.082198396148));
#16925=CARTESIAN_POINT('Ctrl Pts',(9.42743337163542,-73.0954831180953,-1.69756769845304E-11));
#16926=CARTESIAN_POINT('Ctrl Pts',(7.07057502871922,-72.9204831180952,-4.08219839617346));
#16927=CARTESIAN_POINT('Ctrl Pts',(4.71371668580301,-72.7454831180952,-8.16439679232994));
#16928=CARTESIAN_POINT('Ctrl Pts',(-1.4702867290402E-11,-72.5704831180953,
-8.16439679232146));
#16929=CARTESIAN_POINT('Ctrl Pts',(-4.71371668583241,-72.3954831180953,
-8.16439679231297));
#16930=CARTESIAN_POINT('Ctrl Pts',(-7.07057502873392,-72.2204831180952,
-4.082198396148));
#16931=CARTESIAN_POINT('Ctrl Pts',(-9.42743337163542,-72.0454831180953,
1.69768315121407E-11));
#16932=CARTESIAN_POINT('Ctrl Pts',(-7.07057502871922,-71.8704831180952,
4.08219839617346));
#16933=CARTESIAN_POINT('Ctrl Pts',(-4.71371668580301,-71.6954831180952,
8.16439679232994));
#16934=CARTESIAN_POINT('Ctrl Pts',(1.47018674401621E-11,-71.5204831180953,
8.16439679232146));
#16935=CARTESIAN_POINT('Ctrl Pts',(4.71371668583241,-71.3454831180952,8.16439679231297));
#16936=CARTESIAN_POINT('Ctrl Pts',(7.07057502873392,-71.1704831180952,4.082198396148));
#16937=CARTESIAN_POINT('Ctrl Pts',(9.42743337163542,-70.9954831180953,-1.69756769845304E-11));
#16938=CARTESIAN_POINT('Ctrl Pts',(7.07057502871922,-70.8204831180952,-4.08219839617346));
#16939=CARTESIAN_POINT('Ctrl Pts',(4.71371668580301,-70.6454831180952,-8.16439679232994));
#16940=CARTESIAN_POINT('Ctrl Pts',(-1.4702867290402E-11,-70.4704831180953,
-8.16439679232146));
#16941=CARTESIAN_POINT('Ctrl Pts',(-4.71371668583241,-70.2954831180952,
-8.16439679231297));
#16942=CARTESIAN_POINT('Ctrl Pts',(-7.07057502873392,-70.1204831180952,
-4.082198396148));
#16943=CARTESIAN_POINT('Ctrl Pts',(-9.42743337163542,-69.9454831180953,
1.69768315121407E-11));
#16944=CARTESIAN_POINT('Ctrl Pts',(-7.07057502871922,-69.7704831180953,
4.08219839617346));
#16945=CARTESIAN_POINT('Ctrl Pts',(-4.71371668580301,-69.5954831180952,
8.16439679232994));
#16946=CARTESIAN_POINT('Ctrl Pts',(1.47018674401621E-11,-69.4204831180953,
8.16439679232146));
#16947=CARTESIAN_POINT('Ctrl Pts',(4.71371668583241,-69.2454831180953,8.16439679231297));
#16948=CARTESIAN_POINT('Ctrl Pts',(7.07057502873392,-69.0704831180953,4.082198396148));
#16949=CARTESIAN_POINT('Ctrl Pts',(9.42743337163542,-68.8954831180953,-1.69756769845304E-11));
#16950=CARTESIAN_POINT('Ctrl Pts',(7.07057502871922,-68.7204831180952,-4.08219839617346));
#16951=CARTESIAN_POINT('Ctrl Pts',(4.71371668580301,-68.5454831180952,-8.16439679232994));
#16952=CARTESIAN_POINT('Ctrl Pts',(-1.4702867290402E-11,-68.3704831180953,
-8.16439679232146));
#16953=CARTESIAN_POINT('Ctrl Pts',(-4.71371668583241,-68.1954831180952,
-8.16439679231297));
#16954=CARTESIAN_POINT('Ctrl Pts',(-7.07057502873392,-68.0204831180953,
-4.082198396148));
#16955=CARTESIAN_POINT('Ctrl Pts',(-9.42743337163542,-67.8454831180953,
1.69768315121407E-11));
#16956=CARTESIAN_POINT('Ctrl Pts',(-7.07057502871922,-67.6704831180952,
4.08219839617346));
#16957=CARTESIAN_POINT('Ctrl Pts',(-4.71371668580301,-67.4954831180953,
8.16439679232994));
#16958=CARTESIAN_POINT('Ctrl Pts',(1.47018674401621E-11,-67.3204831180953,
8.16439679232146));
#16959=CARTESIAN_POINT('Ctrl Pts',(4.71371668583241,-67.1454831180952,8.16439679231297));
#16960=CARTESIAN_POINT('Ctrl Pts',(7.07057502873392,-66.9704831180952,4.082198396148));
#16961=CARTESIAN_POINT('Ctrl Pts',(9.42743337163542,-66.7954831180953,-1.69756769845304E-11));
#16962=CARTESIAN_POINT('Ctrl Pts',(7.07057502871922,-66.6204831180952,-4.08219839617346));
#16963=CARTESIAN_POINT('Ctrl Pts',(4.71371668580301,-66.4454831180952,-8.16439679232994));
#16964=CARTESIAN_POINT('Ctrl Pts',(-1.4702867290402E-11,-66.2704831180953,
-8.16439679232146));
#16965=CARTESIAN_POINT('Ctrl Pts',(-4.71371668583241,-66.0954831180952,
-8.16439679231297));
#16966=CARTESIAN_POINT('Ctrl Pts',(-7.07057502873392,-65.9204831180952,
-4.082198396148));
#16967=CARTESIAN_POINT('Ctrl Pts',(-9.42743337163542,-65.7454831180953,
1.69768315121407E-11));
#16968=CARTESIAN_POINT('Ctrl Pts',(-7.07057502871922,-65.5704831180953,
4.08219839617346));
#16969=CARTESIAN_POINT('Ctrl Pts',(-4.71371668580301,-65.3954831180953,
8.16439679232994));
#16970=CARTESIAN_POINT('Ctrl Pts',(1.47018674401621E-11,-65.2204831180952,
8.16439679232146));
#16971=CARTESIAN_POINT('Ctrl Pts',(4.71371668583241,-65.0454831180952,8.16439679231297));
#16972=CARTESIAN_POINT('Ctrl Pts',(7.07057502873392,-64.8704831180953,4.082198396148));
#16973=CARTESIAN_POINT('Ctrl Pts',(9.42743337163542,-64.6954831180953,-1.69756769845304E-11));
#16974=CARTESIAN_POINT('Ctrl Pts',(7.07057502871922,-64.5204831180953,-4.08219839617346));
#16975=CARTESIAN_POINT('Ctrl Pts',(4.71371668580301,-64.3454831180953,-8.16439679232994));
#16976=CARTESIAN_POINT('Ctrl Pts',(-1.4702867290402E-11,-64.1704831180952,
-8.16439679232146));
#16977=CARTESIAN_POINT('Ctrl Pts',(-4.71371668583241,-63.9954831180953,
-8.16439679231297));
#16978=CARTESIAN_POINT('Ctrl Pts',(-7.07057502873392,-63.8204831180953,
-4.082198396148));
#16979=CARTESIAN_POINT('Ctrl Pts',(-9.42743337163542,-63.6454831180953,
1.69768315121407E-11));
#16980=CARTESIAN_POINT('Ctrl Pts',(-7.07057502871922,-63.4704831180953,
4.08219839617346));
#16981=CARTESIAN_POINT('Ctrl Pts',(-4.71371668580301,-63.2954831180953,
8.16439679232994));
#16982=CARTESIAN_POINT('Ctrl Pts',(1.47018674401621E-11,-63.1204831180953,
8.16439679232146));
#16983=CARTESIAN_POINT('Ctrl Pts',(4.71371668583241,-62.9454831180952,8.16439679231297));
#16984=CARTESIAN_POINT('Ctrl Pts',(7.07057502873392,-62.7704831180953,4.082198396148));
#16985=CARTESIAN_POINT('Ctrl Pts',(9.42743337163542,-62.5954831180953,-1.69756769845304E-11));
#16986=CARTESIAN_POINT('Ctrl Pts',(7.07057502871922,-62.4204831180953,-4.08219839617346));
#16987=CARTESIAN_POINT('Ctrl Pts',(4.71371668580301,-62.2454831180953,-8.16439679232994));
#16988=CARTESIAN_POINT('Ctrl Pts',(-1.4702867290402E-11,-62.0704831180953,
-8.16439679232146));
#16989=CARTESIAN_POINT('Ctrl Pts',(-4.71371668583241,-61.8954831180952,
-8.16439679231297));
#16990=CARTESIAN_POINT('Ctrl Pts',(-7.07057502873392,-61.7204831180953,
-4.082198396148));
#16991=CARTESIAN_POINT('Ctrl Pts',(-9.42743337163542,-61.5454831180953,
1.69768315121407E-11));
#16992=CARTESIAN_POINT('Ctrl Pts',(-7.07057502871922,-61.3704831180953,
4.08219839617346));
#16993=CARTESIAN_POINT('Ctrl Pts',(-4.71371668580301,-61.1954831180953,
8.16439679232994));
#16994=CARTESIAN_POINT('Ctrl Pts',(1.47018674401621E-11,-61.0204831180953,
8.16439679232146));
#16995=CARTESIAN_POINT('Ctrl Pts',(4.71371668583241,-60.8454831180953,8.16439679231297));
#16996=CARTESIAN_POINT('Ctrl Pts',(7.07057502873392,-60.6704831180953,4.082198396148));
#16997=CARTESIAN_POINT('Ctrl Pts',(9.42743337163542,-60.4954831180953,-1.69756769845304E-11));
#16998=CARTESIAN_POINT('Ctrl Pts',(7.07057502871922,-60.3204831180953,-4.08219839617346));
#16999=CARTESIAN_POINT('Ctrl Pts',(4.71371668580301,-60.1454831180953,-8.16439679232994));
#17000=CARTESIAN_POINT('Ctrl Pts',(-1.4702867290402E-11,-59.9704831180953,
-8.16439679232146));
#17001=CARTESIAN_POINT('Ctrl Pts',(-4.71371668583241,-59.7954831180953,
-8.16439679231297));
#17002=CARTESIAN_POINT('Ctrl Pts',(-7.07057502873392,-59.6204831180953,
-4.082198396148));
#17003=CARTESIAN_POINT('Ctrl Pts',(-9.42743337163542,-59.4454831180953,
1.69768315121407E-11));
#17004=CARTESIAN_POINT('Ctrl Pts',(-7.07057502871922,-59.2704831180953,
4.08219839617346));
#17005=CARTESIAN_POINT('Ctrl Pts',(-4.71371668580301,-59.0954831180953,
8.16439679232994));
#17006=CARTESIAN_POINT('Ctrl Pts',(1.47018674401621E-11,-58.9204831180953,
8.16439679232146));
#17007=CARTESIAN_POINT('Ctrl Pts',(4.71371668583241,-58.7454831180953,8.16439679231297));
#17008=CARTESIAN_POINT('Ctrl Pts',(7.07057502873392,-58.5704831180953,4.082198396148));
#17009=CARTESIAN_POINT('Ctrl Pts',(9.42743337163542,-58.3954831180953,-1.69756769845304E-11));
#17010=CARTESIAN_POINT('Ctrl Pts',(7.07057502871922,-58.2204831180953,-4.08219839617346));
#17011=CARTESIAN_POINT('Ctrl Pts',(4.71371668580301,-58.0454831180953,-8.16439679232994));
#17012=CARTESIAN_POINT('Ctrl Pts',(-1.4702867290402E-11,-57.8704831180952,
-8.16439679232146));
#17013=CARTESIAN_POINT('Ctrl Pts',(-4.71371668583241,-57.6954831180953,
-8.16439679231297));
#17014=CARTESIAN_POINT('Ctrl Pts',(-7.07057502873392,-57.5204831180953,
-4.082198396148));
#17015=CARTESIAN_POINT('Ctrl Pts',(-9.42743337163542,-57.3454831180953,
1.69768315121407E-11));
#17016=CARTESIAN_POINT('Ctrl Pts',(-7.07057502871922,-57.1704831180953,
4.08219839617346));
#17017=CARTESIAN_POINT('Ctrl Pts',(-4.71371668580301,-56.9954831180953,
8.16439679232994));
#17018=CARTESIAN_POINT('Ctrl Pts',(1.47018674401621E-11,-56.8204831180953,
8.16439679232146));
#17019=CARTESIAN_POINT('Ctrl Pts',(4.71371668583241,-56.6454831180953,8.16439679231297));
#17020=CARTESIAN_POINT('Ctrl Pts',(7.07057502873392,-56.4704831180953,4.082198396148));
#17021=CARTESIAN_POINT('Ctrl Pts',(9.42743337163542,-56.2954831180953,-1.69756769845304E-11));
#17022=CARTESIAN_POINT('Ctrl Pts',(7.07057502871922,-56.1204831180953,-4.08219839617346));
#17023=CARTESIAN_POINT('Ctrl Pts',(4.71371668580301,-55.9454831180953,-8.16439679232994));
#17024=CARTESIAN_POINT('Ctrl Pts',(-1.4702867290402E-11,-55.7704831180953,
-8.16439679232146));
#17025=CARTESIAN_POINT('Ctrl Pts',(-4.71371668583241,-55.5954831180953,
-8.16439679231297));
#17026=CARTESIAN_POINT('Ctrl Pts',(-7.07057502873392,-55.4204831180953,
-4.082198396148));
#17027=CARTESIAN_POINT('Ctrl Pts',(-9.42743337163542,-55.2454831180953,
1.69768315121407E-11));
#17028=CARTESIAN_POINT('Ctrl Pts',(-7.07057502871922,-55.0704831180953,
4.08219839617346));
#17029=CARTESIAN_POINT('Ctrl Pts',(-4.71371668580301,-54.8954831180953,
8.16439679232994));
#17030=CARTESIAN_POINT('Ctrl Pts',(1.47018674401621E-11,-54.7204831180953,
8.16439679232146));
#17031=CARTESIAN_POINT('Ctrl Pts',(4.71371668583241,-54.5454831180953,8.16439679231297));
#17032=CARTESIAN_POINT('Ctrl Pts',(7.07057502873392,-54.3704831180953,4.082198396148));
#17033=CARTESIAN_POINT('Ctrl Pts',(9.42743337163542,-54.1954831180953,-1.69756769845304E-11));
#17034=CARTESIAN_POINT('Ctrl Pts',(7.07057502871922,-54.0204831180953,-4.08219839617346));
#17035=CARTESIAN_POINT('Ctrl Pts',(4.71371668580301,-53.8454831180953,-8.16439679232994));
#17036=CARTESIAN_POINT('Ctrl Pts',(-1.4702867290402E-11,-53.6704831180953,
-8.16439679232146));
#17037=CARTESIAN_POINT('Ctrl Pts',(-4.71371668583241,-53.4954831180953,
-8.16439679231297));
#17038=CARTESIAN_POINT('Ctrl Pts',(-7.07057502873392,-53.3204831180953,
-4.082198396148));
#17039=CARTESIAN_POINT('Ctrl Pts',(-9.42743337163542,-53.1454831180953,
1.69768315121407E-11));
#17040=CARTESIAN_POINT('Ctrl Pts',(-7.07057502871922,-52.9704831180953,
4.08219839617346));
#17041=CARTESIAN_POINT('Ctrl Pts',(-4.71371668580301,-52.7954831180953,
8.16439679232994));
#17042=CARTESIAN_POINT('Ctrl Pts',(1.47018674401621E-11,-52.6204831180953,
8.16439679232146));
#17043=CARTESIAN_POINT('Ctrl Pts',(4.71371668583241,-52.4454831180953,8.16439679231297));
#17044=CARTESIAN_POINT('Ctrl Pts',(7.07057502873392,-52.2704831180953,4.082198396148));
#17045=CARTESIAN_POINT('Ctrl Pts',(9.42743337163542,-52.0954831180953,-1.69756769845304E-11));
#17046=CARTESIAN_POINT('Ctrl Pts',(7.07057502871922,-51.9204831180953,-4.08219839617346));
#17047=CARTESIAN_POINT('Ctrl Pts',(4.71371668580301,-51.7454831180953,-8.16439679232994));
#17048=CARTESIAN_POINT('Ctrl Pts',(-1.4702867290402E-11,-51.5704831180953,
-8.16439679232146));
#17049=CARTESIAN_POINT('Ctrl Pts',(-4.71371668583241,-51.3954831180953,
-8.16439679231297));
#17050=CARTESIAN_POINT('Ctrl Pts',(-7.07057502873392,-51.2204831180953,
-4.082198396148));
#17051=CARTESIAN_POINT('Ctrl Pts',(-9.42743337163542,-51.0454831180953,
1.69768315121407E-11));
#17052=CARTESIAN_POINT('Ctrl Pts',(-7.07057502871922,-50.8704831180953,
4.08219839617346));
#17053=CARTESIAN_POINT('Ctrl Pts',(-4.71371668580301,-50.6954831180953,
8.16439679232994));
#17054=CARTESIAN_POINT('Ctrl Pts',(1.47018674401621E-11,-50.5204831180953,
8.16439679232146));
#17055=CARTESIAN_POINT('Ctrl Pts',(4.71371668583241,-50.3454831180953,8.16439679231297));
#17056=CARTESIAN_POINT('Ctrl Pts',(7.07057502873392,-50.1704831180953,4.082198396148));
#17057=CARTESIAN_POINT('Ctrl Pts',(9.42743337163542,-49.9954831180953,-1.69756769845304E-11));
#17058=CARTESIAN_POINT('Ctrl Pts',(7.07057502871922,-49.8204831180953,-4.08219839617346));
#17059=CARTESIAN_POINT('Ctrl Pts',(4.71371668580301,-49.6454831180953,-8.16439679232994));
#17060=CARTESIAN_POINT('Ctrl Pts',(-1.4702867290402E-11,-49.4704831180953,
-8.16439679232146));
#17061=CARTESIAN_POINT('Ctrl Pts',(-4.71371668583241,-49.2954831180953,
-8.16439679231297));
#17062=CARTESIAN_POINT('Ctrl Pts',(-7.07057502873392,-49.1204831180953,
-4.082198396148));
#17063=CARTESIAN_POINT('Ctrl Pts',(-9.42743337163542,-48.9454831180953,
1.69768315121407E-11));
#17064=CARTESIAN_POINT('Ctrl Pts',(-7.07057502871922,-48.7704831180953,
4.08219839617346));
#17065=CARTESIAN_POINT('Ctrl Pts',(-4.71371668580301,-48.5954831180953,
8.16439679232994));
#17066=CARTESIAN_POINT('Ctrl Pts',(1.47018674401621E-11,-48.4204831180953,
8.16439679232146));
#17067=CARTESIAN_POINT('Ctrl Pts',(4.71371668583241,-48.2454831180953,8.16439679231297));
#17068=CARTESIAN_POINT('Ctrl Pts',(7.07057502873392,-48.0704831180953,4.082198396148));
#17069=CARTESIAN_POINT('Ctrl Pts',(9.42743337163542,-47.8954831180953,-1.69756769845304E-11));
#17070=CARTESIAN_POINT('Ctrl Pts',(7.07057502871922,-47.7204831180953,-4.08219839617346));
#17071=CARTESIAN_POINT('Ctrl Pts',(4.71371668580301,-47.5454831180953,-8.16439679232994));
#17072=CARTESIAN_POINT('Ctrl Pts',(-1.4702867290402E-11,-47.3704831180953,
-8.16439679232146));
#17073=CARTESIAN_POINT('Ctrl Pts',(-4.71371668583241,-47.1954831180953,
-8.16439679231297));
#17074=CARTESIAN_POINT('Ctrl Pts',(-7.07057502873392,-47.0204831180953,
-4.082198396148));
#17075=CARTESIAN_POINT('Ctrl Pts',(-9.42743337163542,-46.8454831180953,
1.69768315121407E-11));
#17076=CARTESIAN_POINT('Ctrl Pts',(-7.07057502871922,-46.6704831180953,
4.08219839617346));
#17077=CARTESIAN_POINT('Ctrl Pts',(-4.71371668580301,-46.4954831180953,
8.16439679232994));
#17078=CARTESIAN_POINT('Ctrl Pts',(1.47018674401621E-11,-46.3204831180953,
8.16439679232146));
#17079=CARTESIAN_POINT('Ctrl Pts',(4.71371668583241,-46.1454831180953,8.16439679231297));
#17080=CARTESIAN_POINT('Ctrl Pts',(7.07057502873392,-45.9704831180953,4.082198396148));
#17081=CARTESIAN_POINT('Ctrl Pts',(9.42743337163542,-45.7954831180953,-1.69756769845304E-11));
#17082=CARTESIAN_POINT('Ctrl Pts',(7.07057502871922,-45.6204831180953,-4.08219839617346));
#17083=CARTESIAN_POINT('Ctrl Pts',(4.71371668580301,-45.4454831180953,-8.16439679232994));
#17084=CARTESIAN_POINT('Ctrl Pts',(-1.4702867290402E-11,-45.2704831180953,
-8.16439679232146));
#17085=CARTESIAN_POINT('Ctrl Pts',(-4.71371668583241,-45.0954831180953,
-8.16439679231297));
#17086=CARTESIAN_POINT('Ctrl Pts',(-7.07057502873392,-44.9204831180953,
-4.082198396148));
#17087=CARTESIAN_POINT('Ctrl Pts',(-9.42743337163542,-44.7454831180953,
1.69768315121407E-11));
#17088=CARTESIAN_POINT('Ctrl Pts',(-7.07057502871922,-44.5704831180953,
4.08219839617346));
#17089=CARTESIAN_POINT('Ctrl Pts',(-4.71371668580301,-44.3954831180953,
8.16439679232994));
#17090=CARTESIAN_POINT('Ctrl Pts',(1.47018674401621E-11,-44.2204831180953,
8.16439679232146));
#17091=CARTESIAN_POINT('Ctrl Pts',(4.71371668583241,-44.0454831180953,8.16439679231297));
#17092=CARTESIAN_POINT('Ctrl Pts',(7.07057502873392,-43.8704831180953,4.082198396148));
#17093=CARTESIAN_POINT('Ctrl Pts',(9.42743337163542,-43.6954831180953,-1.69756769845304E-11));
#17094=CARTESIAN_POINT('Ctrl Pts',(7.07057502871922,-43.5204831180953,-4.08219839617346));
#17095=CARTESIAN_POINT('Ctrl Pts',(4.71371668580301,-43.3454831180953,-8.16439679232994));
#17096=CARTESIAN_POINT('Ctrl Pts',(-1.4702867290402E-11,-43.1704831180953,
-8.16439679232146));
#17097=CARTESIAN_POINT('Ctrl Pts',(-4.71371668583241,-42.9954831180953,
-8.16439679231297));
#17098=CARTESIAN_POINT('Ctrl Pts',(-7.07057502873392,-42.8204831180953,
-4.082198396148));
#17099=CARTESIAN_POINT('Ctrl Pts',(-9.42743337163542,-42.6454831180953,
1.69768315121407E-11));
#17100=CARTESIAN_POINT('Ctrl Pts',(-7.07057502871922,-42.4704831180953,
4.08219839617346));
#17101=CARTESIAN_POINT('Ctrl Pts',(-4.71371668580301,-42.2954831180953,
8.16439679232994));
#17102=CARTESIAN_POINT('Ctrl Pts',(1.47018674401621E-11,-42.1204831180953,
8.16439679232146));
#17103=CARTESIAN_POINT('Ctrl Pts',(4.71371668583241,-41.9454831180953,8.16439679231297));
#17104=CARTESIAN_POINT('Ctrl Pts',(7.07057502873392,-41.7704831180953,4.082198396148));
#17105=CARTESIAN_POINT('Ctrl Pts',(9.42743337163542,-41.5954831180953,-1.69756769845304E-11));
#17106=CARTESIAN_POINT('Ctrl Pts',(7.07057502871922,-41.4204831180953,-4.08219839617346));
#17107=CARTESIAN_POINT('Ctrl Pts',(4.71371668580301,-41.2454831180953,-8.16439679232994));
#17108=CARTESIAN_POINT('Ctrl Pts',(-1.4702867290402E-11,-41.0704831180953,
-8.16439679232146));
#17109=CARTESIAN_POINT('Ctrl Pts',(-4.71371668583241,-40.8954831180953,
-8.16439679231297));
#17110=CARTESIAN_POINT('Ctrl Pts',(-7.07057502873392,-40.7204831180953,
-4.082198396148));
#17111=CARTESIAN_POINT('Ctrl Pts',(-9.42743337163542,-40.5454831180953,
1.69768315121407E-11));
#17112=CARTESIAN_POINT('Ctrl Pts',(-7.07057502871922,-40.3704831180953,
4.08219839617346));
#17113=CARTESIAN_POINT('Ctrl Pts',(-4.71371668580301,-40.1954831180953,
8.16439679232994));
#17114=CARTESIAN_POINT('Ctrl Pts',(1.47018674401621E-11,-40.0204831180953,
8.16439679232146));
#17115=CARTESIAN_POINT('Ctrl Pts',(4.71371668583241,-39.8454831180953,8.16439679231297));
#17116=CARTESIAN_POINT('Ctrl Pts',(7.07057502873392,-39.6704831180953,4.082198396148));
#17117=CARTESIAN_POINT('Ctrl Pts',(9.42743337163542,-39.4954831180953,-1.69756769845304E-11));
#17118=CARTESIAN_POINT('Ctrl Pts',(7.07057502871922,-39.3204831180953,-4.08219839617346));
#17119=CARTESIAN_POINT('Ctrl Pts',(4.71371668580301,-39.1454831180953,-8.16439679232994));
#17120=CARTESIAN_POINT('Ctrl Pts',(-1.4702867290402E-11,-38.9704831180953,
-8.16439679232146));
#17121=CARTESIAN_POINT('Ctrl Pts',(-4.71371668583241,-38.7954831180953,
-8.16439679231297));
#17122=CARTESIAN_POINT('Ctrl Pts',(-7.07057502873392,-38.6204831180953,
-4.082198396148));
#17123=CARTESIAN_POINT('Ctrl Pts',(-9.42743337163542,-38.4454831180953,
1.69768315121407E-11));
#17124=CARTESIAN_POINT('Ctrl Pts',(-7.07057502871922,-38.2704831180953,
4.08219839617346));
#17125=CARTESIAN_POINT('Ctrl Pts',(-4.71371668580301,-38.0954831180953,
8.16439679232994));
#17126=CARTESIAN_POINT('Ctrl Pts',(1.47018674401621E-11,-37.9204831180953,
8.16439679232146));
#17127=CARTESIAN_POINT('Ctrl Pts',(4.71371668583241,-37.7454831180953,8.16439679231297));
#17128=CARTESIAN_POINT('Ctrl Pts',(7.07057502873392,-37.5704831180953,4.082198396148));
#17129=CARTESIAN_POINT('Ctrl Pts',(9.42743337163542,-37.3954831180953,-1.69756769845304E-11));
#17130=CARTESIAN_POINT('Ctrl Pts',(7.07057502871922,-37.2204831180953,-4.08219839617346));
#17131=CARTESIAN_POINT('Ctrl Pts',(4.71371668580301,-37.0454831180953,-8.16439679232994));
#17132=CARTESIAN_POINT('Ctrl Pts',(-1.4702867290402E-11,-36.8704831180953,
-8.16439679232146));
#17133=CARTESIAN_POINT('Ctrl Pts',(-4.71371668583241,-36.6954831180953,
-8.16439679231297));
#17134=CARTESIAN_POINT('Ctrl Pts',(-7.07057502873392,-36.5204831180953,
-4.082198396148));
#17135=CARTESIAN_POINT('Ctrl Pts',(-9.42743337163542,-36.3454831180953,
1.69768315121407E-11));
#17136=CARTESIAN_POINT('Ctrl Pts',(-7.07057502871922,-36.1704831180953,
4.08219839617346));
#17137=CARTESIAN_POINT('Ctrl Pts',(-4.71371668580301,-35.9954831180953,
8.16439679232994));
#17138=CARTESIAN_POINT('Ctrl Pts',(1.47018674401621E-11,-35.8204831180953,
8.16439679232146));
#17139=CARTESIAN_POINT('Ctrl Pts',(4.71371668583241,-35.6454831180953,8.16439679231297));
#17140=CARTESIAN_POINT('Ctrl Pts',(7.07057502873392,-35.4704831180953,4.082198396148));
#17141=CARTESIAN_POINT('Ctrl Pts',(9.42743337163542,-35.2954831180953,-1.69756769845304E-11));
#17142=CARTESIAN_POINT('Ctrl Pts',(7.07057502871922,-35.1204831180953,-4.08219839617346));
#17143=CARTESIAN_POINT('Ctrl Pts',(4.71371668580301,-34.9454831180953,-8.16439679232994));
#17144=CARTESIAN_POINT('Ctrl Pts',(-1.4702867290402E-11,-34.7704831180953,
-8.16439679232146));
#17145=CARTESIAN_POINT('Ctrl Pts',(-4.71371668583241,-34.5954831180953,
-8.16439679231297));
#17146=CARTESIAN_POINT('Ctrl Pts',(-7.07057502873392,-34.4204831180953,
-4.082198396148));
#17147=CARTESIAN_POINT('Ctrl Pts',(-9.42743337163542,-34.2454831180953,
1.69768315121407E-11));
#17148=CARTESIAN_POINT('Ctrl Pts',(-7.07057502871922,-34.0704831180953,
4.08219839617346));
#17149=CARTESIAN_POINT('Ctrl Pts',(-4.71371668580301,-33.8954831180953,
8.16439679232994));
#17150=CARTESIAN_POINT('Ctrl Pts',(1.47018674401621E-11,-33.7204831180953,
8.16439679232146));
#17151=CARTESIAN_POINT('Ctrl Pts',(4.71371668583241,-33.5454831180953,8.16439679231297));
#17152=CARTESIAN_POINT('Ctrl Pts',(7.07057502873392,-33.3704831180953,4.082198396148));
#17153=CARTESIAN_POINT('Ctrl Pts',(9.42743337163542,-33.1954831180953,-1.69756769845304E-11));
#17154=CARTESIAN_POINT('Ctrl Pts',(7.07057502871922,-33.0204831180953,-4.08219839617346));
#17155=CARTESIAN_POINT('Ctrl Pts',(4.71371668580301,-32.8454831180953,-8.16439679232994));
#17156=CARTESIAN_POINT('Ctrl Pts',(-1.4702867290402E-11,-32.6704831180953,
-8.16439679232146));
#17157=CARTESIAN_POINT('Ctrl Pts',(-4.71371668583241,-32.4954831180953,
-8.16439679231297));
#17158=CARTESIAN_POINT('Ctrl Pts',(-7.07057502873392,-32.3204831180953,
-4.082198396148));
#17159=CARTESIAN_POINT('Ctrl Pts',(-9.42743337163542,-32.1454831180953,
1.69768315121407E-11));
#17160=CARTESIAN_POINT('Ctrl Pts',(-7.07057502871922,-31.9704831180953,
4.08219839617346));
#17161=CARTESIAN_POINT('Ctrl Pts',(-4.71371668580301,-31.7954831180953,
8.16439679232994));
#17162=CARTESIAN_POINT('Ctrl Pts',(1.47018674401621E-11,-31.6204831180953,
8.16439679232146));
#17163=CARTESIAN_POINT('Ctrl Pts',(4.71371668583241,-31.4454831180953,8.16439679231297));
#17164=CARTESIAN_POINT('Ctrl Pts',(7.07057502873392,-31.2704831180953,4.082198396148));
#17165=CARTESIAN_POINT('Ctrl Pts',(9.42743337163542,-31.0954831180953,-1.69756769845304E-11));
#17166=CARTESIAN_POINT('Ctrl Pts',(7.07057502871922,-30.9204831180953,-4.08219839617346));
#17167=CARTESIAN_POINT('Ctrl Pts',(4.71371668580301,-30.7454831180953,-8.16439679232994));
#17168=CARTESIAN_POINT('Ctrl Pts',(-1.4702867290402E-11,-30.5704831180953,
-8.16439679232146));
#17169=CARTESIAN_POINT('Ctrl Pts',(-4.71371668583241,-30.3954831180953,
-8.16439679231297));
#17170=CARTESIAN_POINT('Ctrl Pts',(-7.07057502873392,-30.2204831180953,
-4.082198396148));
#17171=CARTESIAN_POINT('Ctrl Pts',(-9.42743337163542,-30.0454831180953,
1.69768315121407E-11));
#17172=CARTESIAN_POINT('Ctrl Pts',(-7.07057502871922,-29.8704831180953,
4.08219839617346));
#17173=CARTESIAN_POINT('Ctrl Pts',(-4.71371668580301,-29.6954831180953,
8.16439679232994));
#17174=CARTESIAN_POINT('Ctrl Pts',(1.47018674401621E-11,-29.5204831180953,
8.16439679232146));
#17175=CARTESIAN_POINT('Ctrl Pts',(4.71371668583241,-29.3454831180953,8.16439679231297));
#17176=CARTESIAN_POINT('Ctrl Pts',(7.07057502873392,-29.1704831180953,4.082198396148));
#17177=CARTESIAN_POINT('Ctrl Pts',(9.42743337163542,-28.9954831180954,-1.69756769845304E-11));
#17178=CARTESIAN_POINT('Ctrl Pts',(7.07057502871922,-28.8204831180953,-4.08219839617346));
#17179=CARTESIAN_POINT('Ctrl Pts',(4.71371668580301,-28.6454831180953,-8.16439679232994));
#17180=CARTESIAN_POINT('Ctrl Pts',(-1.4702867290402E-11,-28.4704831180953,
-8.16439679232146));
#17181=CARTESIAN_POINT('Ctrl Pts',(-4.71371668583241,-28.2954831180953,
-8.16439679231297));
#17182=CARTESIAN_POINT('Ctrl Pts',(-7.07057502873392,-28.1204831180953,
-4.082198396148));
#17183=CARTESIAN_POINT('Ctrl Pts',(-9.42743337163542,-27.9454831180954,
1.69768315121407E-11));
#17184=CARTESIAN_POINT('Ctrl Pts',(-7.07057502871922,-27.7704831180953,
4.08219839617346));
#17185=CARTESIAN_POINT('Ctrl Pts',(-4.71371668580301,-27.5954831180953,
8.16439679232994));
#17186=CARTESIAN_POINT('Ctrl Pts',(1.47018674401621E-11,-27.4204831180953,
8.16439679232146));
#17187=CARTESIAN_POINT('Ctrl Pts',(4.71371668583241,-27.2454831180954,8.16439679231297));
#17188=CARTESIAN_POINT('Ctrl Pts',(7.07057502873392,-27.0704831180953,4.082198396148));
#17189=CARTESIAN_POINT('Ctrl Pts',(9.42743337163542,-26.8954831180954,-1.69756769845304E-11));
#17190=CARTESIAN_POINT('Ctrl Pts',(7.07057502871922,-26.7204831180953,-4.08219839617346));
#17191=CARTESIAN_POINT('Ctrl Pts',(4.71371668580301,-26.5454831180953,-8.16439679232994));
#17192=CARTESIAN_POINT('Ctrl Pts',(-1.4702867290402E-11,-26.3704831180953,
-8.16439679232146));
#17193=CARTESIAN_POINT('Ctrl Pts',(-4.71371668583241,-26.1954831180954,
-8.16439679231297));
#17194=CARTESIAN_POINT('Ctrl Pts',(-7.07057502873392,-26.0204831180953,
-4.082198396148));
#17195=CARTESIAN_POINT('Ctrl Pts',(-9.42743337163542,-25.8454831180953,
1.69768315121407E-11));
#17196=CARTESIAN_POINT('Ctrl Pts',(-7.07057502871922,-25.6704831180953,
4.08219839617346));
#17197=CARTESIAN_POINT('Ctrl Pts',(-4.71371668580301,-25.4954831180954,
8.16439679232994));
#17198=CARTESIAN_POINT('Ctrl Pts',(1.47018674401621E-11,-25.3204831180953,
8.16439679232146));
#17199=CARTESIAN_POINT('Ctrl Pts',(4.71371668583241,-25.1454831180954,8.16439679231297));
#17200=CARTESIAN_POINT('Ctrl Pts',(7.07057502873392,-24.9704831180954,4.082198396148));
#17201=CARTESIAN_POINT('Ctrl Pts',(9.42743337163542,-24.7954831180953,-1.69756769845304E-11));
#17202=CARTESIAN_POINT('Ctrl Pts',(7.07057502871922,-24.6204831180954,-4.08219839617346));
#17203=CARTESIAN_POINT('Ctrl Pts',(4.71371668580301,-24.4454831180954,-8.16439679232994));
#17204=CARTESIAN_POINT('Ctrl Pts',(-1.4702867290402E-11,-24.2704831180953,
-8.16439679232146));
#17205=CARTESIAN_POINT('Ctrl Pts',(-4.71371668583241,-24.0954831180954,
-8.16439679231297));
#17206=CARTESIAN_POINT('Ctrl Pts',(-7.07057502873392,-23.9204831180953,
-4.082198396148));
#17207=CARTESIAN_POINT('Ctrl Pts',(-9.42743337163542,-23.7454831180954,
1.69768315121407E-11));
#17208=CARTESIAN_POINT('Ctrl Pts',(-7.07057502871922,-23.5704831180954,
4.08219839617346));
#17209=CARTESIAN_POINT('Ctrl Pts',(-4.71371668580301,-23.3954831180954,
8.16439679232994));
#17210=CARTESIAN_POINT('Ctrl Pts',(1.47018674401621E-11,-23.2204831180953,
8.16439679232146));
#17211=CARTESIAN_POINT('Ctrl Pts',(4.71371668583241,-23.0454831180954,8.16439679231297));
#17212=CARTESIAN_POINT('Ctrl Pts',(7.07057502873392,-22.8704831180954,4.082198396148));
#17213=CARTESIAN_POINT('Ctrl Pts',(9.42743337163542,-22.6954831180954,-1.69756769845304E-11));
#17214=CARTESIAN_POINT('Ctrl Pts',(7.07057502871922,-22.5204831180954,-4.08219839617346));
#17215=CARTESIAN_POINT('Ctrl Pts',(4.71371668580301,-22.3454831180954,-8.16439679232994));
#17216=CARTESIAN_POINT('Ctrl Pts',(-1.4702867290402E-11,-22.1704831180954,
-8.16439679232146));
#17217=CARTESIAN_POINT('Ctrl Pts',(-4.71371668583241,-21.9954831180954,
-8.16439679231297));
#17218=CARTESIAN_POINT('Ctrl Pts',(-7.07057502873392,-21.8204831180954,
-4.082198396148));
#17219=CARTESIAN_POINT('Ctrl Pts',(-9.42743337163542,-21.6454831180954,
1.69768315121407E-11));
#17220=CARTESIAN_POINT('Ctrl Pts',(-7.07057502871922,-21.4704831180953,
4.08219839617346));
#17221=CARTESIAN_POINT('Ctrl Pts',(-4.71371668580301,-21.2954831180954,
8.16439679232994));
#17222=CARTESIAN_POINT('Ctrl Pts',(1.47018674401621E-11,-21.1204831180954,
8.16439679232146));
#17223=CARTESIAN_POINT('Ctrl Pts',(4.71371668583241,-20.9454831180954,8.16439679231297));
#17224=CARTESIAN_POINT('Ctrl Pts',(7.07057502873392,-20.7704831180954,4.082198396148));
#17225=CARTESIAN_POINT('Ctrl Pts',(9.42743337163542,-20.5954831180954,-1.69756769845304E-11));
#17226=CARTESIAN_POINT('Ctrl Pts',(7.07057502871922,-20.4204831180954,-4.08219839617346));
#17227=CARTESIAN_POINT('Ctrl Pts',(4.71371668580301,-20.2454831180954,-8.16439679232994));
#17228=CARTESIAN_POINT('Ctrl Pts',(-1.4702867290402E-11,-20.0704831180954,
-8.16439679232146));
#17229=CARTESIAN_POINT('Ctrl Pts',(-4.71371668583241,-19.8954831180954,
-8.16439679231297));
#17230=CARTESIAN_POINT('Ctrl Pts',(-7.07057502873392,-19.7204831180954,
-4.082198396148));
#17231=CARTESIAN_POINT('Ctrl Pts',(-9.42743337163542,-19.5454831180954,
1.69768315121407E-11));
#17232=CARTESIAN_POINT('Ctrl Pts',(-7.07057502871922,-19.3704831180954,
4.08219839617346));
#17233=CARTESIAN_POINT('Ctrl Pts',(-4.71371668580301,-19.1954831180954,
8.16439679232994));
#17234=CARTESIAN_POINT('Ctrl Pts',(1.47018674401621E-11,-19.0204831180954,
8.16439679232146));
#17235=CARTESIAN_POINT('Ctrl Pts',(4.71371668583241,-18.8454831180954,8.16439679231297));
#17236=CARTESIAN_POINT('Ctrl Pts',(7.07057502873392,-18.6704831180954,4.082198396148));
#17237=CARTESIAN_POINT('Ctrl Pts',(9.42743337163542,-18.4954831180954,-1.69756769845304E-11));
#17238=CARTESIAN_POINT('Ctrl Pts',(7.07057502871922,-18.3204831180954,-4.08219839617346));
#17239=CARTESIAN_POINT('Ctrl Pts',(4.71371668580301,-18.1454831180954,-8.16439679232994));
#17240=CARTESIAN_POINT('Ctrl Pts',(-1.4702867290402E-11,-17.9704831180954,
-8.16439679232146));
#17241=CARTESIAN_POINT('Ctrl Pts',(-4.71371668583241,-17.7954831180954,
-8.16439679231297));
#17242=CARTESIAN_POINT('Ctrl Pts',(-7.07057502873392,-17.6204831180954,
-4.082198396148));
#17243=CARTESIAN_POINT('Ctrl Pts',(-9.42743337163542,-17.4454831180954,
1.69768315121407E-11));
#17244=CARTESIAN_POINT('Ctrl Pts',(-7.07057502871922,-17.2704831180954,
4.08219839617346));
#17245=CARTESIAN_POINT('Ctrl Pts',(-4.71371668580301,-17.0954831180954,
8.16439679232994));
#17246=CARTESIAN_POINT('Ctrl Pts',(1.47018674401621E-11,-16.9204831180954,
8.16439679232146));
#17247=CARTESIAN_POINT('Ctrl Pts',(4.71371668583241,-16.7454831180954,8.16439679231297));
#17248=CARTESIAN_POINT('Ctrl Pts',(7.07057502873392,-16.5704831180954,4.082198396148));
#17249=CARTESIAN_POINT('Ctrl Pts',(9.42743337163542,-16.3954831180954,-1.69756769845304E-11));
#17250=CARTESIAN_POINT('Ctrl Pts',(7.07057502871922,-16.2204831180954,-4.08219839617346));
#17251=CARTESIAN_POINT('Ctrl Pts',(4.71371668580301,-16.0454831180954,-8.16439679232994));
#17252=CARTESIAN_POINT('Ctrl Pts',(-1.4702867290402E-11,-15.8704831180954,
-8.16439679232146));
#17253=CARTESIAN_POINT('Ctrl Pts',(-4.71371668583241,-15.6954831180954,
-8.16439679231297));
#17254=CARTESIAN_POINT('Ctrl Pts',(-7.07057502873392,-15.5204831180954,
-4.082198396148));
#17255=CARTESIAN_POINT('Ctrl Pts',(-9.42743337163542,-15.3454831180954,
1.69768315121407E-11));
#17256=CARTESIAN_POINT('Ctrl Pts',(-7.07057502871922,-15.1704831180954,
4.08219839617346));
#17257=CARTESIAN_POINT('Ctrl Pts',(-4.71371668580301,-14.9954831180954,
8.16439679232994));
#17258=CARTESIAN_POINT('Ctrl Pts',(1.47018674401621E-11,-14.8204831180954,
8.16439679232146));
#17259=CARTESIAN_POINT('Ctrl Pts',(4.71371668583241,-14.6454831180954,8.16439679231297));
#17260=CARTESIAN_POINT('Ctrl Pts',(7.07057502873392,-14.4704831180954,4.082198396148));
#17261=CARTESIAN_POINT('Ctrl Pts',(9.42743337163542,-14.2954831180954,-1.69756769845304E-11));
#17262=CARTESIAN_POINT('Ctrl Pts',(7.07057502871922,-14.1204831180954,-4.08219839617346));
#17263=CARTESIAN_POINT('Ctrl Pts',(4.71371668580301,-13.9454831180954,-8.16439679232994));
#17264=CARTESIAN_POINT('Ctrl Pts',(-1.4702867290402E-11,-13.7704831180954,
-8.16439679232146));
#17265=CARTESIAN_POINT('Ctrl Pts',(-4.71371668583241,-13.5954831180954,
-8.16439679231297));
#17266=CARTESIAN_POINT('Ctrl Pts',(-7.07057502873392,-13.4204831180954,
-4.082198396148));
#17267=CARTESIAN_POINT('Ctrl Pts',(-9.42743337163542,-13.2454831180954,
1.69768315121407E-11));
#17268=CARTESIAN_POINT('Ctrl Pts',(-7.07057502871922,-13.0704831180954,
4.08219839617346));
#17269=CARTESIAN_POINT('Ctrl Pts',(-4.71371668580301,-12.8954831180954,
8.16439679232994));
#17270=CARTESIAN_POINT('Ctrl Pts',(1.47018674401621E-11,-12.7204831180954,
8.16439679232146));
#17271=CARTESIAN_POINT('Ctrl Pts',(4.71371668583241,-12.5454831180954,8.16439679231297));
#17272=CARTESIAN_POINT('Ctrl Pts',(7.07057502873392,-12.3704831180954,4.082198396148));
#17273=CARTESIAN_POINT('Ctrl Pts',(9.42743337163542,-12.1954831180954,-1.69756769845304E-11));
#17274=CARTESIAN_POINT('Ctrl Pts',(7.07057502871922,-12.0204831180954,-4.08219839617346));
#17275=CARTESIAN_POINT('Ctrl Pts',(4.71371668580301,-11.8454831180954,-8.16439679232994));
#17276=CARTESIAN_POINT('Ctrl Pts',(-1.4702867290402E-11,-11.6704831180954,
-8.16439679232146));
#17277=CARTESIAN_POINT('Ctrl Pts',(-4.71371668583241,-11.4954831180954,
-8.16439679231297));
#17278=CARTESIAN_POINT('Ctrl Pts',(-7.07057502873392,-11.3204831180954,
-4.082198396148));
#17279=CARTESIAN_POINT('Ctrl Pts',(-9.42743337163542,-11.1454831180954,
1.69768315121407E-11));
#17280=CARTESIAN_POINT('Ctrl Pts',(-7.07057502871922,-10.9704831180954,
4.08219839617346));
#17281=CARTESIAN_POINT('Ctrl Pts',(-4.71371668580301,-10.7954831180954,
8.16439679232994));
#17282=CARTESIAN_POINT('Ctrl Pts',(1.47018674401621E-11,-10.6204831180954,
8.16439679232146));
#17283=CARTESIAN_POINT('Ctrl Pts',(4.71371668583241,-10.4454831180954,8.16439679231297));
#17284=CARTESIAN_POINT('Ctrl Pts',(7.07057502873392,-10.2704831180954,4.082198396148));
#17285=CARTESIAN_POINT('Ctrl Pts',(9.42743337163542,-10.0954831180954,-1.69756769845304E-11));
#17286=CARTESIAN_POINT('Ctrl Pts',(7.07057502871922,-9.92048311809537,-4.08219839617346));
#17287=CARTESIAN_POINT('Ctrl Pts',(4.71371668580301,-9.74548311809539,-8.16439679232994));
#17288=CARTESIAN_POINT('Ctrl Pts',(-1.4702867290402E-11,-9.57048311809539,
-8.16439679232146));
#17289=CARTESIAN_POINT('Ctrl Pts',(-4.71371668583241,-9.39548311809538,
-8.16439679231297));
#17290=CARTESIAN_POINT('Ctrl Pts',(-7.07057502873392,-9.22048311809539,
-4.082198396148));
#17291=CARTESIAN_POINT('Ctrl Pts',(-9.42743337163542,-9.04548311809539,
1.69768315121407E-11));
#17292=CARTESIAN_POINT('Ctrl Pts',(-7.07057502871922,-8.87048311809537,
4.08219839617346));
#17293=CARTESIAN_POINT('Ctrl Pts',(-4.71371668580301,-8.6954831180954,8.16439679232994));
#17294=CARTESIAN_POINT('Ctrl Pts',(1.47018674401621E-11,-8.52048311809539,
8.16439679232146));
#17295=CARTESIAN_POINT('Ctrl Pts',(4.71371668583241,-8.34548311809539,8.16439679231297));
#17296=CARTESIAN_POINT('Ctrl Pts',(7.07057502873392,-8.1704831180954,4.082198396148));
#17297=CARTESIAN_POINT('Ctrl Pts',(9.42743337163542,-7.9954831180954,-1.69756769845304E-11));
#17298=CARTESIAN_POINT('Ctrl Pts',(7.07057502871922,-7.82048311809538,-4.08219839617346));
#17299=CARTESIAN_POINT('Ctrl Pts',(4.71371668580301,-7.64548311809541,-8.16439679232994));
#17300=CARTESIAN_POINT('Ctrl Pts',(-1.4702867290402E-11,-7.47048311809539,
-8.16439679232146));
#17301=CARTESIAN_POINT('Ctrl Pts',(-4.71371668583241,-7.29548311809539,
-8.16439679231297));
#17302=CARTESIAN_POINT('Ctrl Pts',(-7.07057502873392,-7.12048311809538,
-4.082198396148));
#17303=CARTESIAN_POINT('Ctrl Pts',(-9.42743337163542,-6.94548311809541,
1.69768315121407E-11));
#17304=CARTESIAN_POINT('Ctrl Pts',(-7.07057502871922,-6.77048311809538,
4.08219839617346));
#17305=CARTESIAN_POINT('Ctrl Pts',(-4.71371668580301,-6.59548311809539,
8.16439679232994));
#17306=CARTESIAN_POINT('Ctrl Pts',(1.47018674401621E-11,-6.4204831180954,
8.16439679232146));
#17307=CARTESIAN_POINT('Ctrl Pts',(4.71371668583241,-6.24548311809539,8.16439679231297));
#17308=CARTESIAN_POINT('Ctrl Pts',(7.07057502873392,-6.07048311809538,4.082198396148));
#17309=CARTESIAN_POINT('Ctrl Pts',(9.42743337163542,-5.89548311809541,-1.69756769845304E-11));
#17310=CARTESIAN_POINT('Ctrl Pts',(7.07057502871922,-5.72048311809538,-4.08219839617346));
#17311=CARTESIAN_POINT('Ctrl Pts',(4.71371668580301,-5.54548311809539,-8.16439679232994));
#17312=CARTESIAN_POINT('Ctrl Pts',(-1.4702867290402E-11,-5.3704831180954,
-8.16439679232146));
#17313=CARTESIAN_POINT('Ctrl Pts',(-4.71371668583241,-5.19548311809541,
-8.16439679231297));
#17314=CARTESIAN_POINT('Ctrl Pts',(-7.07057502873392,-5.02048311809538,
-4.082198396148));
#17315=CARTESIAN_POINT('Ctrl Pts',(-9.42743337163542,-4.84548311809541,
1.69768315121407E-11));
#17316=CARTESIAN_POINT('Ctrl Pts',(-7.07057502871922,-4.6704831180954,4.08219839617346));
#17317=CARTESIAN_POINT('Ctrl Pts',(-4.71371668580301,-4.49548311809539,
8.16439679232994));
#17318=CARTESIAN_POINT('Ctrl Pts',(1.47018674401621E-11,-4.3204831180954,
8.16439679232146));
#17319=CARTESIAN_POINT('Ctrl Pts',(4.71371668583241,-4.14548311809541,8.16439679231297));
#17320=CARTESIAN_POINT('Ctrl Pts',(7.07057502873392,-3.97048311809539,4.082198396148));
#17321=CARTESIAN_POINT('Ctrl Pts',(9.42743337163542,-3.79548311809541,-1.69756769845304E-11));
#17322=CARTESIAN_POINT('Ctrl Pts',(7.07057502871922,-3.6204831180954,-4.08219839617346));
#17323=CARTESIAN_POINT('Ctrl Pts',(4.71371668580301,-3.44548311809539,-8.16439679232994));
#17324=CARTESIAN_POINT('Ctrl Pts',(-1.4702867290402E-11,-3.27048311809541,
-8.16439679232146));
#17325=CARTESIAN_POINT('Ctrl Pts',(-4.71371668583241,-3.09548311809541,
-8.16439679231297));
#17326=CARTESIAN_POINT('Ctrl Pts',(-7.07057502873392,-2.92048311809539,
-4.082198396148));
#17327=CARTESIAN_POINT('Ctrl Pts',(-9.42743337163542,-2.74548311809539,
1.69768315121407E-11));
#17328=CARTESIAN_POINT('Ctrl Pts',(-7.07057502871922,-2.5704831180954,4.08219839617346));
#17329=CARTESIAN_POINT('Ctrl Pts',(-4.71371668580301,-2.3954831180954,8.16439679232994));
#17330=CARTESIAN_POINT('Ctrl Pts',(1.47018674401621E-11,-2.22048311809539,
8.16439679232146));
#17331=CARTESIAN_POINT('Ctrl Pts',(4.71371668583241,-2.04548311809541,8.16439679231297));
#17332=CARTESIAN_POINT('Ctrl Pts',(7.07057502873392,-1.87048311809539,4.082198396148));
#17333=CARTESIAN_POINT('Ctrl Pts',(9.42743337163542,-1.69548311809539,-1.69756769845304E-11));
#17334=CARTESIAN_POINT('Ctrl Pts',(7.07057502871922,-1.52048311809541,-4.08219839617346));
#17335=CARTESIAN_POINT('Ctrl Pts',(4.71371668580301,-1.34548311809541,-8.16439679232994));
#17336=CARTESIAN_POINT('Ctrl Pts',(-1.4702867290402E-11,-1.17048311809539,
-8.16439679232146));
#17337=CARTESIAN_POINT('Ctrl Pts',(-4.71371668583241,-0.995483118095416,
-8.16439679231297));
#17338=CARTESIAN_POINT('Ctrl Pts',(-7.07057502873392,-0.820483118095406,
-4.082198396148));
#17339=CARTESIAN_POINT('Ctrl Pts',(-9.42743337163542,-0.645483118095396,
1.69768315121407E-11));
#17340=CARTESIAN_POINT('Ctrl Pts',(-7.07057502871922,-0.47048311809541,
4.08219839617346));
#17341=CARTESIAN_POINT('Ctrl Pts',(-4.71371668580301,-0.295483118095414,
8.16439679232994));
#17342=CARTESIAN_POINT('Ctrl Pts',(1.47018674401621E-11,-0.120483118095393,
8.16439679232146));
#17343=CARTESIAN_POINT('Ctrl Pts',(4.71371668583241,0.054516881904581,8.16439679231297));
#17344=CARTESIAN_POINT('Ctrl Pts',(7.07057502873392,0.229516881904591,4.082198396148));
#17345=CARTESIAN_POINT('Ctrl Pts',(9.42743337163542,0.404516881904601,-1.69756769845304E-11));
#17346=CARTESIAN_POINT('Ctrl Pts',(7.07057502871922,0.579516881904587,-4.08219839617346));
#17347=CARTESIAN_POINT('Ctrl Pts',(4.71371668580301,0.754516881904583,-8.16439679232994));
#17348=CARTESIAN_POINT('Ctrl Pts',(-1.4702867290402E-11,0.929516881904604,
-8.16439679232146));
#17349=CARTESIAN_POINT('Ctrl Pts',(-4.71371668583241,1.10451688190458,-8.16439679231297));
#17350=CARTESIAN_POINT('Ctrl Pts',(-7.07057502873392,1.27951688190459,-4.082198396148));
#17351=CARTESIAN_POINT('Ctrl Pts',(-9.42743337163542,1.4545168819046,1.69768315121407E-11));
#17352=CARTESIAN_POINT('Ctrl Pts',(-7.07057502871922,1.62951688190461,4.08219839617346));
#17353=CARTESIAN_POINT('Ctrl Pts',(-4.71371668580301,1.80451688190458,8.16439679232994));
#17354=CARTESIAN_POINT('Ctrl Pts',(1.47018674401621E-11,1.9795168819046,
8.16439679232146));
#17355=CARTESIAN_POINT('Ctrl Pts',(4.71371668583241,2.1545168819046,8.16439679231297));
#17356=CARTESIAN_POINT('Ctrl Pts',(7.07057502873392,2.32951688190458,4.082198396148));
#17357=CARTESIAN_POINT('Ctrl Pts',(9.42743337163542,2.50451688190458,-1.69756769845304E-11));
#17358=CARTESIAN_POINT('Ctrl Pts',(7.07057502871922,2.6795168819046,-4.08219839617346));
#17359=CARTESIAN_POINT('Ctrl Pts',(4.71371668580301,2.85451688190458,-8.16439679232994));
#17360=CARTESIAN_POINT('Ctrl Pts',(-1.4702867290402E-11,3.02951688190459,
-8.16439679232146));
#17361=CARTESIAN_POINT('Ctrl Pts',(-4.71371668583241,3.2045168819046,-8.16439679231297));
#17362=CARTESIAN_POINT('Ctrl Pts',(-7.07057502873392,3.37951688190458,-4.082198396148));
#17363=CARTESIAN_POINT('Ctrl Pts',(-9.42743337163542,3.55451688190458,1.69768315121407E-11));
#17364=CARTESIAN_POINT('Ctrl Pts',(-7.07057502871922,3.7295168819046,4.08219839617346));
#17365=CARTESIAN_POINT('Ctrl Pts',(-4.71371668580301,3.90451688190458,8.16439679232994));
#17366=CARTESIAN_POINT('Ctrl Pts',(1.47018674401621E-11,4.07951688190458,
8.16439679232146));
#17367=CARTESIAN_POINT('Ctrl Pts',(4.71371668583241,4.2545168819046,8.16439679231297));
#17368=CARTESIAN_POINT('Ctrl Pts',(7.07057502873392,4.42951688190458,4.082198396148));
#17369=CARTESIAN_POINT('Ctrl Pts',(9.42743337163542,4.60451688190458,-1.69756769845304E-11));
#17370=CARTESIAN_POINT('Ctrl Pts',(7.07057502871922,4.7795168819046,-4.08219839617346));
#17371=CARTESIAN_POINT('Ctrl Pts',(4.71371668580301,4.95451688190457,-8.16439679232994));
#17372=CARTESIAN_POINT('Ctrl Pts',(-1.4702867290402E-11,5.12951688190458,
-8.16439679232146));
#17373=CARTESIAN_POINT('Ctrl Pts',(-4.71371668583241,5.30451688190459,-8.16439679231297));
#17374=CARTESIAN_POINT('Ctrl Pts',(-7.07057502873392,5.47951688190458,-4.082198396148));
#17375=CARTESIAN_POINT('Ctrl Pts',(-9.42743337163542,5.65451688190458,1.69768315121407E-11));
#17376=CARTESIAN_POINT('Ctrl Pts',(-7.07057502871922,5.82951688190459,4.08219839617346));
#17377=CARTESIAN_POINT('Ctrl Pts',(-4.71371668580301,6.00451688190457,8.16439679232994));
#17378=CARTESIAN_POINT('Ctrl Pts',(1.47018674401621E-11,6.17951688190458,
8.16439679232146));
#17379=CARTESIAN_POINT('Ctrl Pts',(4.71371668583241,6.35451688190459,8.16439679231297));
#17380=CARTESIAN_POINT('Ctrl Pts',(7.07057502873392,6.52951688190459,4.082198396148));
#17381=CARTESIAN_POINT('Ctrl Pts',(9.42743337163542,6.70451688190457,-1.69756769845304E-11));
#17382=CARTESIAN_POINT('Ctrl Pts',(7.07057502871922,6.87951688190458,-4.08219839617346));
#17383=CARTESIAN_POINT('Ctrl Pts',(4.71371668580301,7.05451688190459,-8.16439679232994));
#17384=CARTESIAN_POINT('Ctrl Pts',(-1.4702867290402E-11,7.22951688190457,
-8.16439679232146));
#17385=CARTESIAN_POINT('Ctrl Pts',(-4.71371668583241,7.40451688190458,-8.16439679231297));
#17386=CARTESIAN_POINT('Ctrl Pts',(-7.07057502873392,7.57951688190459,-4.082198396148));
#17387=CARTESIAN_POINT('Ctrl Pts',(-9.42743337163542,7.75451688190457,1.69768315121407E-11));
#17388=CARTESIAN_POINT('Ctrl Pts',(-7.07057502871922,7.92951688190458,4.08219839617346));
#17389=CARTESIAN_POINT('Ctrl Pts',(-4.71371668580301,8.10451688190458,8.16439679232994));
#17390=CARTESIAN_POINT('Ctrl Pts',(1.47018674401621E-11,8.27951688190457,
8.16439679232146));
#17391=CARTESIAN_POINT('Ctrl Pts',(4.71371668583241,8.45451688190457,8.16439679231297));
#17392=CARTESIAN_POINT('Ctrl Pts',(7.07057502873392,8.62951688190459,4.082198396148));
#17393=CARTESIAN_POINT('Ctrl Pts',(9.42743337163542,8.80451688190457,-1.69756769845304E-11));
#17394=CARTESIAN_POINT('Ctrl Pts',(7.07057502871922,8.97951688190457,-4.08219839617346));
#17395=CARTESIAN_POINT('Ctrl Pts',(4.71371668580301,9.15451688190458,-8.16439679232994));
#17396=CARTESIAN_POINT('Ctrl Pts',(-1.4702867290402E-11,9.32951688190457,
-8.16439679232146));
#17397=CARTESIAN_POINT('Ctrl Pts',(-4.71371668583241,9.50451688190457,-8.16439679231297));
#17398=CARTESIAN_POINT('Ctrl Pts',(-7.07057502873392,9.67951688190458,-4.082198396148));
#17399=CARTESIAN_POINT('Ctrl Pts',(-9.42743337163542,9.85451688190457,1.69768315121407E-11));
#17400=CARTESIAN_POINT('Ctrl Pts',(-7.07057502871922,10.0295168819046,4.08219839617346));
#17401=CARTESIAN_POINT('Ctrl Pts',(-4.71371668580301,10.2045168819046,8.16439679232994));
#17402=CARTESIAN_POINT('Ctrl Pts',(1.47018674401621E-11,10.3795168819046,
8.16439679232146));
#17403=CARTESIAN_POINT('Ctrl Pts',(4.71371668583241,10.5545168819046,8.16439679231297));
#17404=CARTESIAN_POINT('Ctrl Pts',(7.07057502873392,10.7295168819046,4.082198396148));
#17405=CARTESIAN_POINT('Ctrl Pts',(9.42743337163542,10.9045168819046,-1.69756769845304E-11));
#17406=CARTESIAN_POINT('Ctrl Pts',(7.07057502871922,11.0795168819046,-4.08219839617346));
#17407=CARTESIAN_POINT('Ctrl Pts',(4.71371668580301,11.2545168819046,-8.16439679232994));
#17408=CARTESIAN_POINT('Ctrl Pts',(-1.4702867290402E-11,11.4295168819046,
-8.16439679232146));
#17409=CARTESIAN_POINT('Ctrl Pts',(-4.71371668583241,11.6045168819046,-8.16439679231297));
#17410=CARTESIAN_POINT('Ctrl Pts',(-7.07057502873392,11.7795168819046,-4.082198396148));
#17411=CARTESIAN_POINT('Ctrl Pts',(-9.42743337163542,11.9545168819046,1.69768315121407E-11));
#17412=CARTESIAN_POINT('Ctrl Pts',(-7.07057502871922,12.1295168819046,4.08219839617346));
#17413=CARTESIAN_POINT('Ctrl Pts',(-4.71371668580301,12.3045168819046,8.16439679232994));
#17414=CARTESIAN_POINT('Ctrl Pts',(1.47018674401621E-11,12.4795168819046,
8.16439679232146));
#17415=CARTESIAN_POINT('Ctrl Pts',(4.71371668583241,12.6545168819046,8.16439679231297));
#17416=CARTESIAN_POINT('Ctrl Pts',(7.07057502873392,12.8295168819046,4.082198396148));
#17417=CARTESIAN_POINT('Ctrl Pts',(9.42743337163542,13.0045168819046,-1.69756769845304E-11));
#17418=CARTESIAN_POINT('Ctrl Pts',(7.07057502871922,13.1795168819046,-4.08219839617346));
#17419=CARTESIAN_POINT('Ctrl Pts',(4.71371668580301,13.3545168819046,-8.16439679232994));
#17420=CARTESIAN_POINT('Ctrl Pts',(-1.4702867290402E-11,13.5295168819046,
-8.16439679232146));
#17421=CARTESIAN_POINT('Ctrl Pts',(-4.71371668583241,13.7045168819046,-8.16439679231297));
#17422=CARTESIAN_POINT('Ctrl Pts',(-7.07057502873392,13.8795168819046,-4.082198396148));
#17423=CARTESIAN_POINT('Ctrl Pts',(-9.42743337163542,14.0545168819046,1.69768315121407E-11));
#17424=CARTESIAN_POINT('Ctrl Pts',(-7.07057502871922,14.2295168819046,4.08219839617346));
#17425=CARTESIAN_POINT('Ctrl Pts',(-4.71371668580301,14.4045168819046,8.16439679232994));
#17426=CARTESIAN_POINT('Ctrl Pts',(1.47018674401621E-11,14.5795168819046,
8.16439679232146));
#17427=CARTESIAN_POINT('Ctrl Pts',(4.71371668583241,14.7545168819045,8.16439679231297));
#17428=CARTESIAN_POINT('Ctrl Pts',(7.07057502873392,14.9295168819046,4.082198396148));
#17429=CARTESIAN_POINT('Ctrl Pts',(9.42743337163542,15.1045168819046,-1.69756769845304E-11));
#17430=CARTESIAN_POINT('Ctrl Pts',(7.07057502871922,15.2795168819046,-4.08219839617346));
#17431=CARTESIAN_POINT('Ctrl Pts',(4.71371668580301,15.4545168819046,-8.16439679232994));
#17432=CARTESIAN_POINT('Ctrl Pts',(-1.4702867290402E-11,15.6295168819046,
-8.16439679232146));
#17433=CARTESIAN_POINT('Ctrl Pts',(-4.71371668583241,15.8045168819046,-8.16439679231297));
#17434=CARTESIAN_POINT('Ctrl Pts',(-7.07057502873392,15.9795168819046,-4.082198396148));
#17435=CARTESIAN_POINT('Ctrl Pts',(-9.42743337163542,16.1545168819046,1.69768315121407E-11));
#17436=CARTESIAN_POINT('Ctrl Pts',(-7.07057502871922,16.3295168819046,4.08219839617346));
#17437=CARTESIAN_POINT('Ctrl Pts',(-4.71371668580301,16.5045168819046,8.16439679232994));
#17438=CARTESIAN_POINT('Ctrl Pts',(1.47018674401621E-11,16.6795168819046,
8.16439679232146));
#17439=CARTESIAN_POINT('Ctrl Pts',(4.71371668583241,16.8545168819046,8.16439679231297));
#17440=CARTESIAN_POINT('Ctrl Pts',(7.07057502873392,17.0295168819046,4.082198396148));
#17441=CARTESIAN_POINT('Ctrl Pts',(9.42743337163542,17.2045168819045,-1.69756769845304E-11));
#17442=CARTESIAN_POINT('Ctrl Pts',(7.07057502871922,17.3795168819046,-4.08219839617346));
#17443=CARTESIAN_POINT('Ctrl Pts',(4.71371668580301,17.5545168819045,-8.16439679232994));
#17444=CARTESIAN_POINT('Ctrl Pts',(-1.4702867290402E-11,17.7295168819046,
-8.16439679232146));
#17445=CARTESIAN_POINT('Ctrl Pts',(-4.71371668583241,17.9045168819046,-8.16439679231297));
#17446=CARTESIAN_POINT('Ctrl Pts',(-7.07057502873392,18.0795168819045,-4.082198396148));
#17447=CARTESIAN_POINT('Ctrl Pts',(-9.42743337163542,18.2545168819045,1.69768315121407E-11));
#17448=CARTESIAN_POINT('Ctrl Pts',(-7.07057502871922,18.4295168819046,4.08219839617346));
#17449=CARTESIAN_POINT('Ctrl Pts',(-4.71371668580301,18.6045168819045,8.16439679232994));
#17450=CARTESIAN_POINT('Ctrl Pts',(1.47018674401621E-11,18.7795168819046,
8.16439679232146));
#17451=CARTESIAN_POINT('Ctrl Pts',(4.71371668583241,18.9545168819045,8.16439679231297));
#17452=CARTESIAN_POINT('Ctrl Pts',(7.07057502873392,19.1295168819045,4.082198396148));
#17453=CARTESIAN_POINT('Ctrl Pts',(9.42743337163542,19.3045168819045,-1.69756769845304E-11));
#17454=CARTESIAN_POINT('Ctrl Pts',(7.07057502871922,19.4795168819046,-4.08219839617346));
#17455=CARTESIAN_POINT('Ctrl Pts',(4.71371668580301,19.6545168819046,-8.16439679232994));
#17456=CARTESIAN_POINT('Ctrl Pts',(-1.4702867290402E-11,19.8295168819045,
-8.16439679232146));
#17457=CARTESIAN_POINT('Ctrl Pts',(-4.71371668583241,20.0045168819045,-8.16439679231297));
#17458=CARTESIAN_POINT('Ctrl Pts',(-7.07057502873392,20.1795168819046,-4.082198396148));
#17459=CARTESIAN_POINT('Ctrl Pts',(-9.42743337163542,20.3545168819045,1.69768315121407E-11));
#17460=CARTESIAN_POINT('Ctrl Pts',(-7.07057502871922,20.5295168819046,4.08219839617346));
#17461=CARTESIAN_POINT('Ctrl Pts',(-4.71371668580301,20.7045168819046,8.16439679232994));
#17462=CARTESIAN_POINT('Ctrl Pts',(1.47018674401621E-11,20.8795168819045,
8.16439679232146));
#17463=CARTESIAN_POINT('Ctrl Pts',(4.71371668583241,21.0545168819045,8.16439679231297));
#17464=CARTESIAN_POINT('Ctrl Pts',(7.07057502873392,21.2295168819046,4.082198396148));
#17465=CARTESIAN_POINT('Ctrl Pts',(9.42743337163542,21.4045168819045,-1.69756769845304E-11));
#17466=CARTESIAN_POINT('Ctrl Pts',(7.07057502871922,21.5795168819045,-4.08219839617346));
#17467=CARTESIAN_POINT('Ctrl Pts',(4.71371668580301,21.7545168819045,-8.16439679232994));
#17468=CARTESIAN_POINT('Ctrl Pts',(-1.4702867290402E-11,21.9295168819045,
-8.16439679232146));
#17469=CARTESIAN_POINT('Ctrl Pts',(-4.71371668583241,22.1045168819045,-8.16439679231297));
#17470=CARTESIAN_POINT('Ctrl Pts',(-7.07057502873392,22.2795168819046,-4.082198396148));
#17471=CARTESIAN_POINT('Ctrl Pts',(-9.42743337163542,22.4545168819045,1.69768315121407E-11));
#17472=CARTESIAN_POINT('Ctrl Pts',(-7.07057502871922,22.6295168819045,4.08219839617346));
#17473=CARTESIAN_POINT('Ctrl Pts',(-4.71371668580301,22.8045168819045,8.16439679232994));
#17474=CARTESIAN_POINT('Ctrl Pts',(1.47018674401621E-11,22.9795168819045,
8.16439679232146));
#17475=CARTESIAN_POINT('Ctrl Pts',(4.71371668583241,23.1545168819045,8.16439679231297));
#17476=CARTESIAN_POINT('Ctrl Pts',(7.07057502873392,23.3295168819046,4.082198396148));
#17477=CARTESIAN_POINT('Ctrl Pts',(9.42743337163542,23.5045168819045,-1.69756769845304E-11));
#17478=CARTESIAN_POINT('Ctrl Pts',(7.07057502871922,23.6795168819045,-4.08219839617346));
#17479=CARTESIAN_POINT('Ctrl Pts',(4.71371668580301,23.8545168819045,-8.16439679232994));
#17480=CARTESIAN_POINT('Ctrl Pts',(-1.4702867290402E-11,24.0295168819045,
-8.16439679232146));
#17481=CARTESIAN_POINT('Ctrl Pts',(-4.71371668583241,24.2045168819045,-8.16439679231297));
#17482=CARTESIAN_POINT('Ctrl Pts',(-7.07057502873392,24.3795168819046,-4.082198396148));
#17483=CARTESIAN_POINT('Ctrl Pts',(-9.42743337163542,24.5545168819046,1.69768315121407E-11));
#17484=CARTESIAN_POINT('Ctrl Pts',(-7.07057502871922,24.7295168819045,4.08219839617346));
#17485=CARTESIAN_POINT('Ctrl Pts',(-4.71371668580301,24.9045168819045,8.16439679232994));
#17486=CARTESIAN_POINT('Ctrl Pts',(1.47018674401621E-11,25.0795168819046,
8.16439679232146));
#17487=CARTESIAN_POINT('Ctrl Pts',(4.71371668583241,25.2545168819045,8.16439679231297));
#17488=CARTESIAN_POINT('Ctrl Pts',(7.07057502873392,25.4295168819045,4.082198396148));
#17489=CARTESIAN_POINT('Ctrl Pts',(9.42743337163542,25.6045168819045,-1.69756769845304E-11));
#17490=CARTESIAN_POINT('Ctrl Pts',(7.07057502871922,25.7795168819045,-4.08219839617346));
#17491=CARTESIAN_POINT('Ctrl Pts',(4.71371668580301,25.9545168819045,-8.16439679232994));
#17492=CARTESIAN_POINT('Ctrl Pts',(-1.4702867290402E-11,26.1295168819045,
-8.16439679232146));
#17493=CARTESIAN_POINT('Ctrl Pts',(-1.4702867290402E-11,-143.703019107145,
-8.16439679232146));
#17494=CARTESIAN_POINT('Ctrl Pts',(-4.71371668583241,-143.528019107145,
-8.16439679231297));
#17495=CARTESIAN_POINT('Ctrl Pts',(-7.07057502873392,-143.353019107145,
-4.082198396148));
#17496=CARTESIAN_POINT('Ctrl Pts',(-9.42743337163542,-143.178019107145,
1.69768315121407E-11));
#17497=CARTESIAN_POINT('Ctrl Pts',(-7.07057502871922,-143.003019107145,
4.08219839617346));
#17498=CARTESIAN_POINT('Ctrl Pts',(-4.71371668580301,-142.828019107145,
8.16439679232994));
#17499=CARTESIAN_POINT('Ctrl Pts',(1.47018674401621E-11,-142.653019107145,
8.16439679232146));
#17500=CARTESIAN_POINT('Ctrl Pts',(4.71371668583241,-142.478019107145,8.16439679231297));
#17501=CARTESIAN_POINT('Ctrl Pts',(7.07057502873392,-142.303019107145,4.082198396148));
#17502=CARTESIAN_POINT('Ctrl Pts',(9.42743337163542,-142.128019107145,-1.69756769845304E-11));
#17503=CARTESIAN_POINT('Ctrl Pts',(7.07057502871922,-141.953019107145,-4.08219839617346));
#17504=CARTESIAN_POINT('Ctrl Pts',(4.71371668580301,-141.778019107145,-8.16439679232994));
#17505=CARTESIAN_POINT('Ctrl Pts',(-1.4702867290402E-11,-141.603019107145,
-8.16439679232146));
#17506=CARTESIAN_POINT('Ctrl Pts',(-4.71371668583241,-141.428019107145,
-8.16439679231297));
#17507=CARTESIAN_POINT('Ctrl Pts',(-7.07057502873392,-141.253019107145,
-4.082198396148));
#17508=CARTESIAN_POINT('Ctrl Pts',(-9.42743337163542,-141.078019107145,
1.69768315121407E-11));
#17509=CARTESIAN_POINT('Ctrl Pts',(-7.07057502871922,-140.903019107145,
4.08219839617346));
#17510=CARTESIAN_POINT('Ctrl Pts',(-4.71371668580301,-140.728019107145,
8.16439679232994));
#17511=CARTESIAN_POINT('Ctrl Pts',(1.47018674401621E-11,-140.553019107145,
8.16439679232146));
#17512=CARTESIAN_POINT('Ctrl Pts',(4.71371668583241,-140.378019107145,8.16439679231297));
#17513=CARTESIAN_POINT('Ctrl Pts',(7.07057502873392,-140.203019107145,4.082198396148));
#17514=CARTESIAN_POINT('Ctrl Pts',(9.42743337163542,-140.028019107145,-1.69756769845304E-11));
#17515=CARTESIAN_POINT('Ctrl Pts',(7.07057502871922,-139.853019107145,-4.08219839617346));
#17516=CARTESIAN_POINT('Ctrl Pts',(4.71371668580301,-139.678019107145,-8.16439679232994));
#17517=CARTESIAN_POINT('Ctrl Pts',(-1.4702867290402E-11,-139.503019107145,
-8.16439679232146));
#17518=CARTESIAN_POINT('Ctrl Pts',(-4.71371668583241,-139.328019107145,
-8.16439679231297));
#17519=CARTESIAN_POINT('Ctrl Pts',(-7.07057502873392,-139.153019107145,
-4.082198396148));
#17520=CARTESIAN_POINT('Ctrl Pts',(-9.42743337163542,-138.978019107145,
1.69768315121407E-11));
#17521=CARTESIAN_POINT('Ctrl Pts',(-7.07057502871922,-138.803019107145,
4.08219839617346));
#17522=CARTESIAN_POINT('Ctrl Pts',(-4.71371668580301,-138.628019107145,
8.16439679232994));
#17523=CARTESIAN_POINT('Ctrl Pts',(1.47018674401621E-11,-138.453019107145,
8.16439679232146));
#17524=CARTESIAN_POINT('Ctrl Pts',(4.71371668583241,-138.278019107145,8.16439679231297));
#17525=CARTESIAN_POINT('Ctrl Pts',(7.07057502873392,-138.103019107145,4.082198396148));
#17526=CARTESIAN_POINT('Ctrl Pts',(9.42743337163542,-137.928019107145,-1.69756769845304E-11));
#17527=CARTESIAN_POINT('Ctrl Pts',(7.07057502871922,-137.753019107145,-4.08219839617346));
#17528=CARTESIAN_POINT('Ctrl Pts',(4.71371668580301,-137.578019107145,-8.16439679232994));
#17529=CARTESIAN_POINT('Ctrl Pts',(-1.4702867290402E-11,-137.403019107145,
-8.16439679232146));
#17530=CARTESIAN_POINT('Ctrl Pts',(-4.71371668583241,-137.228019107145,
-8.16439679231297));
#17531=CARTESIAN_POINT('Ctrl Pts',(-7.07057502873392,-137.053019107145,
-4.082198396148));
#17532=CARTESIAN_POINT('Ctrl Pts',(-9.42743337163542,-136.878019107145,
1.69768315121407E-11));
#17533=CARTESIAN_POINT('Ctrl Pts',(-7.07057502871922,-136.703019107145,
4.08219839617346));
#17534=CARTESIAN_POINT('Ctrl Pts',(-4.71371668580301,-136.528019107145,
8.16439679232994));
#17535=CARTESIAN_POINT('Ctrl Pts',(1.47018674401621E-11,-136.353019107145,
8.16439679232146));
#17536=CARTESIAN_POINT('Ctrl Pts',(4.71371668583241,-136.178019107145,8.16439679231297));
#17537=CARTESIAN_POINT('Ctrl Pts',(7.07057502873392,-136.003019107145,4.082198396148));
#17538=CARTESIAN_POINT('Ctrl Pts',(9.42743337163542,-135.828019107145,-1.69756769845304E-11));
#17539=CARTESIAN_POINT('Ctrl Pts',(7.07057502871922,-135.653019107145,-4.08219839617346));
#17540=CARTESIAN_POINT('Ctrl Pts',(4.71371668580301,-135.478019107145,-8.16439679232994));
#17541=CARTESIAN_POINT('Ctrl Pts',(-1.4702867290402E-11,-135.303019107145,
-8.16439679232146));
#17542=CARTESIAN_POINT('Ctrl Pts',(-4.71371668583241,-135.128019107145,
-8.16439679231297));
#17543=CARTESIAN_POINT('Ctrl Pts',(-7.07057502873392,-134.953019107145,
-4.082198396148));
#17544=CARTESIAN_POINT('Ctrl Pts',(-9.42743337163542,-134.778019107145,
1.69768315121407E-11));
#17545=CARTESIAN_POINT('Ctrl Pts',(-7.07057502871922,-134.603019107145,
4.08219839617346));
#17546=CARTESIAN_POINT('Ctrl Pts',(-4.71371668580301,-134.428019107145,
8.16439679232994));
#17547=CARTESIAN_POINT('Ctrl Pts',(1.47018674401621E-11,-134.253019107145,
8.16439679232146));
#17548=CARTESIAN_POINT('Ctrl Pts',(4.71371668583241,-134.078019107145,8.16439679231297));
#17549=CARTESIAN_POINT('Ctrl Pts',(7.07057502873392,-133.903019107145,4.082198396148));
#17550=CARTESIAN_POINT('Ctrl Pts',(9.42743337163542,-133.728019107145,-1.69756769845304E-11));
#17551=CARTESIAN_POINT('Ctrl Pts',(7.07057502871922,-133.553019107145,-4.08219839617346));
#17552=CARTESIAN_POINT('Ctrl Pts',(4.71371668580301,-133.378019107145,-8.16439679232994));
#17553=CARTESIAN_POINT('Ctrl Pts',(-1.4702867290402E-11,-133.203019107145,
-8.16439679232146));
#17554=CARTESIAN_POINT('Ctrl Pts',(-4.71371668583241,-133.028019107145,
-8.16439679231297));
#17555=CARTESIAN_POINT('Ctrl Pts',(-7.07057502873392,-132.853019107145,
-4.082198396148));
#17556=CARTESIAN_POINT('Ctrl Pts',(-9.42743337163542,-132.678019107145,
1.69768315121407E-11));
#17557=CARTESIAN_POINT('Ctrl Pts',(-7.07057502871922,-132.503019107145,
4.08219839617346));
#17558=CARTESIAN_POINT('Ctrl Pts',(-4.71371668580301,-132.328019107145,
8.16439679232994));
#17559=CARTESIAN_POINT('Ctrl Pts',(1.47018674401621E-11,-132.153019107145,
8.16439679232146));
#17560=CARTESIAN_POINT('Ctrl Pts',(4.71371668583241,-131.978019107145,8.16439679231297));
#17561=CARTESIAN_POINT('Ctrl Pts',(7.07057502873392,-131.803019107145,4.082198396148));
#17562=CARTESIAN_POINT('Ctrl Pts',(9.42743337163542,-131.628019107145,-1.69756769845304E-11));
#17563=CARTESIAN_POINT('Ctrl Pts',(7.07057502871922,-131.453019107145,-4.08219839617346));
#17564=CARTESIAN_POINT('Ctrl Pts',(4.71371668580301,-131.278019107145,-8.16439679232994));
#17565=CARTESIAN_POINT('Ctrl Pts',(-1.4702867290402E-11,-131.103019107145,
-8.16439679232146));
#17566=CARTESIAN_POINT('Ctrl Pts',(-4.71371668583241,-130.928019107145,
-8.16439679231297));
#17567=CARTESIAN_POINT('Ctrl Pts',(-7.07057502873392,-130.753019107145,
-4.082198396148));
#17568=CARTESIAN_POINT('Ctrl Pts',(-9.42743337163542,-130.578019107145,
1.69768315121407E-11));
#17569=CARTESIAN_POINT('Ctrl Pts',(-7.07057502871922,-130.403019107145,
4.08219839617346));
#17570=CARTESIAN_POINT('Ctrl Pts',(-4.71371668580301,-130.228019107145,
8.16439679232994));
#17571=CARTESIAN_POINT('Ctrl Pts',(1.47018674401621E-11,-130.053019107145,
8.16439679232146));
#17572=CARTESIAN_POINT('Ctrl Pts',(4.71371668583241,-129.878019107145,8.16439679231297));
#17573=CARTESIAN_POINT('Ctrl Pts',(7.07057502873392,-129.703019107145,4.082198396148));
#17574=CARTESIAN_POINT('Ctrl Pts',(9.42743337163542,-129.528019107145,-1.69756769845304E-11));
#17575=CARTESIAN_POINT('Ctrl Pts',(7.07057502871922,-129.353019107145,-4.08219839617346));
#17576=CARTESIAN_POINT('Ctrl Pts',(4.71371668580301,-129.178019107145,-8.16439679232994));
#17577=CARTESIAN_POINT('Ctrl Pts',(-1.4702867290402E-11,-129.003019107145,
-8.16439679232146));
#17578=CARTESIAN_POINT('Ctrl Pts',(-4.71371668583241,-128.828019107145,
-8.16439679231297));
#17579=CARTESIAN_POINT('Ctrl Pts',(-7.07057502873392,-128.653019107145,
-4.082198396148));
#17580=CARTESIAN_POINT('Ctrl Pts',(-9.42743337163542,-128.478019107145,
1.69768315121407E-11));
#17581=CARTESIAN_POINT('Ctrl Pts',(-7.07057502871922,-128.303019107145,
4.08219839617346));
#17582=CARTESIAN_POINT('Ctrl Pts',(-4.71371668580301,-128.128019107145,
8.16439679232994));
#17583=CARTESIAN_POINT('Ctrl Pts',(1.47018674401621E-11,-127.953019107145,
8.16439679232146));
#17584=CARTESIAN_POINT('Ctrl Pts',(4.71371668583241,-127.778019107145,8.16439679231297));
#17585=CARTESIAN_POINT('Ctrl Pts',(7.07057502873392,-127.603019107145,4.082198396148));
#17586=CARTESIAN_POINT('Ctrl Pts',(9.42743337163542,-127.428019107145,-1.69756769845304E-11));
#17587=CARTESIAN_POINT('Ctrl Pts',(7.07057502871922,-127.253019107145,-4.08219839617346));
#17588=CARTESIAN_POINT('Ctrl Pts',(4.71371668580301,-127.078019107145,-8.16439679232994));
#17589=CARTESIAN_POINT('Ctrl Pts',(-1.4702867290402E-11,-126.903019107145,
-8.16439679232146));
#17590=CARTESIAN_POINT('Ctrl Pts',(-4.71371668583241,-126.728019107145,
-8.16439679231297));
#17591=CARTESIAN_POINT('Ctrl Pts',(-7.07057502873392,-126.553019107145,
-4.082198396148));
#17592=CARTESIAN_POINT('Ctrl Pts',(-9.42743337163542,-126.378019107145,
1.69768315121407E-11));
#17593=CARTESIAN_POINT('Ctrl Pts',(-7.07057502871922,-126.203019107145,
4.08219839617346));
#17594=CARTESIAN_POINT('Ctrl Pts',(-4.71371668580301,-126.028019107145,
8.16439679232994));
#17595=CARTESIAN_POINT('Ctrl Pts',(1.47018674401621E-11,-125.853019107145,
8.16439679232146));
#17596=CARTESIAN_POINT('Ctrl Pts',(4.71371668583241,-125.678019107145,8.16439679231297));
#17597=CARTESIAN_POINT('Ctrl Pts',(7.07057502873392,-125.503019107145,4.082198396148));
#17598=CARTESIAN_POINT('Ctrl Pts',(9.42743337163542,-125.328019107145,-1.69756769845304E-11));
#17599=CARTESIAN_POINT('Ctrl Pts',(7.07057502871922,-125.153019107145,-4.08219839617346));
#17600=CARTESIAN_POINT('Ctrl Pts',(4.71371668580301,-124.978019107145,-8.16439679232994));
#17601=CARTESIAN_POINT('Ctrl Pts',(-1.4702867290402E-11,-124.803019107145,
-8.16439679232146));
#17602=CARTESIAN_POINT('Ctrl Pts',(-4.71371668583241,-124.628019107145,
-8.16439679231297));
#17603=CARTESIAN_POINT('Ctrl Pts',(-7.07057502873392,-124.453019107145,
-4.082198396148));
#17604=CARTESIAN_POINT('Ctrl Pts',(-9.42743337163542,-124.278019107145,
1.69768315121407E-11));
#17605=CARTESIAN_POINT('Ctrl Pts',(-7.07057502871922,-124.103019107145,
4.08219839617346));
#17606=CARTESIAN_POINT('Ctrl Pts',(-4.71371668580301,-123.928019107145,
8.16439679232994));
#17607=CARTESIAN_POINT('Ctrl Pts',(1.47018674401621E-11,-123.753019107145,
8.16439679232146));
#17608=CARTESIAN_POINT('Ctrl Pts',(4.71371668583241,-123.578019107145,8.16439679231297));
#17609=CARTESIAN_POINT('Ctrl Pts',(7.07057502873392,-123.403019107145,4.082198396148));
#17610=CARTESIAN_POINT('Ctrl Pts',(9.42743337163542,-123.228019107145,-1.69756769845304E-11));
#17611=CARTESIAN_POINT('Ctrl Pts',(7.07057502871922,-123.053019107145,-4.08219839617346));
#17612=CARTESIAN_POINT('Ctrl Pts',(4.71371668580301,-122.878019107145,-8.16439679232994));
#17613=CARTESIAN_POINT('Ctrl Pts',(-1.4702867290402E-11,-122.703019107145,
-8.16439679232146));
#17614=CARTESIAN_POINT('Ctrl Pts',(-4.71371668583241,-122.528019107145,
-8.16439679231297));
#17615=CARTESIAN_POINT('Ctrl Pts',(-7.07057502873392,-122.353019107145,
-4.082198396148));
#17616=CARTESIAN_POINT('Ctrl Pts',(-9.42743337163542,-122.178019107145,
1.69768315121407E-11));
#17617=CARTESIAN_POINT('Ctrl Pts',(-7.07057502871922,-122.003019107145,
4.08219839617346));
#17618=CARTESIAN_POINT('Ctrl Pts',(-4.71371668580301,-121.828019107145,
8.16439679232994));
#17619=CARTESIAN_POINT('Ctrl Pts',(1.47018674401621E-11,-121.653019107145,
8.16439679232146));
#17620=CARTESIAN_POINT('Ctrl Pts',(4.71371668583241,-121.478019107145,8.16439679231297));
#17621=CARTESIAN_POINT('Ctrl Pts',(7.07057502873392,-121.303019107145,4.082198396148));
#17622=CARTESIAN_POINT('Ctrl Pts',(9.42743337163542,-121.128019107145,-1.69756769845304E-11));
#17623=CARTESIAN_POINT('Ctrl Pts',(7.07057502871922,-120.953019107145,-4.08219839617346));
#17624=CARTESIAN_POINT('Ctrl Pts',(4.71371668580301,-120.778019107145,-8.16439679232994));
#17625=CARTESIAN_POINT('Ctrl Pts',(-1.4702867290402E-11,-120.603019107145,
-8.16439679232146));
#17626=CARTESIAN_POINT('Ctrl Pts',(-4.71371668583241,-120.428019107145,
-8.16439679231297));
#17627=CARTESIAN_POINT('Ctrl Pts',(-7.07057502873392,-120.253019107145,
-4.082198396148));
#17628=CARTESIAN_POINT('Ctrl Pts',(-9.42743337163542,-120.078019107145,
1.69768315121407E-11));
#17629=CARTESIAN_POINT('Ctrl Pts',(-7.07057502871922,-119.903019107145,
4.08219839617346));
#17630=CARTESIAN_POINT('Ctrl Pts',(-4.71371668580301,-119.728019107145,
8.16439679232994));
#17631=CARTESIAN_POINT('Ctrl Pts',(1.47018674401621E-11,-119.553019107145,
8.16439679232146));
#17632=CARTESIAN_POINT('Ctrl Pts',(4.71371668583241,-119.378019107145,8.16439679231297));
#17633=CARTESIAN_POINT('Ctrl Pts',(7.07057502873392,-119.203019107145,4.082198396148));
#17634=CARTESIAN_POINT('Ctrl Pts',(9.42743337163542,-119.028019107145,-1.69756769845304E-11));
#17635=CARTESIAN_POINT('Ctrl Pts',(7.07057502871922,-118.853019107145,-4.08219839617346));
#17636=CARTESIAN_POINT('Ctrl Pts',(4.71371668580301,-118.678019107145,-8.16439679232994));
#17637=CARTESIAN_POINT('Ctrl Pts',(-1.4702867290402E-11,-118.503019107145,
-8.16439679232146));
#17638=CARTESIAN_POINT('Ctrl Pts',(-4.71371668583241,-118.328019107145,
-8.16439679231297));
#17639=CARTESIAN_POINT('Ctrl Pts',(-7.07057502873392,-118.153019107145,
-4.082198396148));
#17640=CARTESIAN_POINT('Ctrl Pts',(-9.42743337163542,-117.978019107145,
1.69768315121407E-11));
#17641=CARTESIAN_POINT('Ctrl Pts',(-7.07057502871922,-117.803019107145,
4.08219839617346));
#17642=CARTESIAN_POINT('Ctrl Pts',(-4.71371668580301,-117.628019107145,
8.16439679232994));
#17643=CARTESIAN_POINT('Ctrl Pts',(1.47018674401621E-11,-117.453019107145,
8.16439679232146));
#17644=CARTESIAN_POINT('Ctrl Pts',(4.71371668583241,-117.278019107145,8.16439679231297));
#17645=CARTESIAN_POINT('Ctrl Pts',(7.07057502873392,-117.103019107145,4.082198396148));
#17646=CARTESIAN_POINT('Ctrl Pts',(9.42743337163542,-116.928019107145,-1.69756769845304E-11));
#17647=CARTESIAN_POINT('Ctrl Pts',(7.07057502871922,-116.753019107145,-4.08219839617346));
#17648=CARTESIAN_POINT('Ctrl Pts',(4.71371668580301,-116.578019107145,-8.16439679232994));
#17649=CARTESIAN_POINT('Ctrl Pts',(-1.4702867290402E-11,-116.403019107145,
-8.16439679232146));
#17650=CARTESIAN_POINT('Ctrl Pts',(-4.71371668583241,-116.228019107145,
-8.16439679231297));
#17651=CARTESIAN_POINT('Ctrl Pts',(-7.07057502873392,-116.053019107145,
-4.082198396148));
#17652=CARTESIAN_POINT('Ctrl Pts',(-9.42743337163542,-115.878019107145,
1.69768315121407E-11));
#17653=CARTESIAN_POINT('Ctrl Pts',(-7.07057502871922,-115.703019107145,
4.08219839617346));
#17654=CARTESIAN_POINT('Ctrl Pts',(-4.71371668580301,-115.528019107145,
8.16439679232994));
#17655=CARTESIAN_POINT('Ctrl Pts',(1.47018674401621E-11,-115.353019107145,
8.16439679232146));
#17656=CARTESIAN_POINT('Ctrl Pts',(4.71371668583241,-115.178019107145,8.16439679231297));
#17657=CARTESIAN_POINT('Ctrl Pts',(7.07057502873392,-115.003019107145,4.082198396148));
#17658=CARTESIAN_POINT('Ctrl Pts',(9.42743337163542,-114.828019107145,-1.69756769845304E-11));
#17659=CARTESIAN_POINT('Ctrl Pts',(7.07057502871922,-114.653019107145,-4.08219839617346));
#17660=CARTESIAN_POINT('Ctrl Pts',(4.71371668580301,-114.478019107145,-8.16439679232994));
#17661=CARTESIAN_POINT('Ctrl Pts',(-1.4702867290402E-11,-114.303019107145,
-8.16439679232146));
#17662=CARTESIAN_POINT('Ctrl Pts',(-4.71371668583241,-114.128019107145,
-8.16439679231297));
#17663=CARTESIAN_POINT('Ctrl Pts',(-7.07057502873392,-113.953019107145,
-4.082198396148));
#17664=CARTESIAN_POINT('Ctrl Pts',(-9.42743337163542,-113.778019107145,
1.69768315121407E-11));
#17665=CARTESIAN_POINT('Ctrl Pts',(-7.07057502871922,-113.603019107145,
4.08219839617346));
#17666=CARTESIAN_POINT('Ctrl Pts',(-4.71371668580301,-113.428019107145,
8.16439679232994));
#17667=CARTESIAN_POINT('Ctrl Pts',(1.47018674401621E-11,-113.253019107145,
8.16439679232146));
#17668=CARTESIAN_POINT('Ctrl Pts',(4.71371668583241,-113.078019107145,8.16439679231297));
#17669=CARTESIAN_POINT('Ctrl Pts',(7.07057502873392,-112.903019107145,4.082198396148));
#17670=CARTESIAN_POINT('Ctrl Pts',(9.42743337163542,-112.728019107145,-1.69756769845304E-11));
#17671=CARTESIAN_POINT('Ctrl Pts',(7.07057502871922,-112.553019107145,-4.08219839617346));
#17672=CARTESIAN_POINT('Ctrl Pts',(4.71371668580301,-112.378019107145,-8.16439679232994));
#17673=CARTESIAN_POINT('Ctrl Pts',(-1.4702867290402E-11,-112.203019107145,
-8.16439679232146));
#17674=CARTESIAN_POINT('Ctrl Pts',(-4.71371668583241,-112.028019107145,
-8.16439679231297));
#17675=CARTESIAN_POINT('Ctrl Pts',(-7.07057502873392,-111.853019107145,
-4.082198396148));
#17676=CARTESIAN_POINT('Ctrl Pts',(-9.42743337163542,-111.678019107145,
1.69768315121407E-11));
#17677=CARTESIAN_POINT('Ctrl Pts',(-7.07057502871922,-111.503019107145,
4.08219839617346));
#17678=CARTESIAN_POINT('Ctrl Pts',(-4.71371668580301,-111.328019107145,
8.16439679232994));
#17679=CARTESIAN_POINT('Ctrl Pts',(1.47018674401621E-11,-111.153019107145,
8.16439679232146));
#17680=CARTESIAN_POINT('Ctrl Pts',(4.71371668583241,-110.978019107145,8.16439679231297));
#17681=CARTESIAN_POINT('Ctrl Pts',(7.07057502873392,-110.803019107145,4.082198396148));
#17682=CARTESIAN_POINT('Ctrl Pts',(9.42743337163542,-110.628019107145,-1.69756769845304E-11));
#17683=CARTESIAN_POINT('Ctrl Pts',(7.07057502871922,-110.453019107145,-4.08219839617346));
#17684=CARTESIAN_POINT('Ctrl Pts',(4.71371668580301,-110.278019107145,-8.16439679232994));
#17685=CARTESIAN_POINT('Ctrl Pts',(-1.4702867290402E-11,-110.103019107145,
-8.16439679232146));
#17686=CARTESIAN_POINT('Ctrl Pts',(-4.71371668583241,-109.928019107145,
-8.16439679231297));
#17687=CARTESIAN_POINT('Ctrl Pts',(-7.07057502873392,-109.753019107145,
-4.082198396148));
#17688=CARTESIAN_POINT('Ctrl Pts',(-9.42743337163542,-109.578019107145,
1.69768315121407E-11));
#17689=CARTESIAN_POINT('Ctrl Pts',(-7.07057502871922,-109.403019107145,
4.08219839617346));
#17690=CARTESIAN_POINT('Ctrl Pts',(-4.71371668580301,-109.228019107145,
8.16439679232994));
#17691=CARTESIAN_POINT('Ctrl Pts',(1.47018674401621E-11,-109.053019107145,
8.16439679232146));
#17692=CARTESIAN_POINT('Ctrl Pts',(4.71371668583241,-108.878019107145,8.16439679231297));
#17693=CARTESIAN_POINT('Ctrl Pts',(7.07057502873392,-108.703019107145,4.082198396148));
#17694=CARTESIAN_POINT('Ctrl Pts',(9.42743337163542,-108.528019107145,-1.69756769845304E-11));
#17695=CARTESIAN_POINT('Ctrl Pts',(7.07057502871922,-108.353019107145,-4.08219839617346));
#17696=CARTESIAN_POINT('Ctrl Pts',(4.71371668580301,-108.178019107145,-8.16439679232994));
#17697=CARTESIAN_POINT('Ctrl Pts',(-1.4702867290402E-11,-108.003019107145,
-8.16439679232146));
#17698=CARTESIAN_POINT('Ctrl Pts',(-4.71371668583241,-107.828019107145,
-8.16439679231297));
#17699=CARTESIAN_POINT('Ctrl Pts',(-7.07057502873392,-107.653019107145,
-4.082198396148));
#17700=CARTESIAN_POINT('Ctrl Pts',(-9.42743337163542,-107.478019107145,
1.69768315121407E-11));
#17701=CARTESIAN_POINT('Ctrl Pts',(-7.07057502871922,-107.303019107145,
4.08219839617346));
#17702=CARTESIAN_POINT('Ctrl Pts',(-4.71371668580301,-107.128019107145,
8.16439679232994));
#17703=CARTESIAN_POINT('Ctrl Pts',(1.47018674401621E-11,-106.953019107145,
8.16439679232146));
#17704=CARTESIAN_POINT('Ctrl Pts',(4.71371668583241,-106.778019107145,8.16439679231297));
#17705=CARTESIAN_POINT('Ctrl Pts',(7.07057502873392,-106.603019107145,4.082198396148));
#17706=CARTESIAN_POINT('Ctrl Pts',(9.42743337163542,-106.428019107145,-1.69756769845304E-11));
#17707=CARTESIAN_POINT('Ctrl Pts',(7.07057502871922,-106.253019107145,-4.08219839617346));
#17708=CARTESIAN_POINT('Ctrl Pts',(4.71371668580301,-106.078019107145,-8.16439679232994));
#17709=CARTESIAN_POINT('Ctrl Pts',(-1.4702867290402E-11,-105.903019107145,
-8.16439679232146));
#17710=CARTESIAN_POINT('Ctrl Pts',(-4.71371668583241,-105.728019107145,
-8.16439679231297));
#17711=CARTESIAN_POINT('Ctrl Pts',(-7.07057502873392,-105.553019107145,
-4.082198396148));
#17712=CARTESIAN_POINT('Ctrl Pts',(-9.42743337163542,-105.378019107145,
1.69768315121407E-11));
#17713=CARTESIAN_POINT('Ctrl Pts',(-7.07057502871922,-105.203019107145,
4.08219839617346));
#17714=CARTESIAN_POINT('Ctrl Pts',(-4.71371668580301,-105.028019107145,
8.16439679232994));
#17715=CARTESIAN_POINT('Ctrl Pts',(1.47018674401621E-11,-104.853019107145,
8.16439679232146));
#17716=CARTESIAN_POINT('Ctrl Pts',(4.71371668583241,-104.678019107145,8.16439679231297));
#17717=CARTESIAN_POINT('Ctrl Pts',(7.07057502873392,-104.503019107145,4.082198396148));
#17718=CARTESIAN_POINT('Ctrl Pts',(9.42743337163542,-104.328019107145,-1.69756769845304E-11));
#17719=CARTESIAN_POINT('Ctrl Pts',(7.07057502871922,-104.153019107145,-4.08219839617346));
#17720=CARTESIAN_POINT('Ctrl Pts',(4.71371668580301,-103.978019107145,-8.16439679232994));
#17721=CARTESIAN_POINT('Ctrl Pts',(-1.4702867290402E-11,-103.803019107145,
-8.16439679232146));
#17722=CARTESIAN_POINT('Ctrl Pts',(-4.71371668583241,-103.628019107145,
-8.16439679231297));
#17723=CARTESIAN_POINT('Ctrl Pts',(-7.07057502873392,-103.453019107145,
-4.082198396148));
#17724=CARTESIAN_POINT('Ctrl Pts',(-9.42743337163542,-103.278019107145,
1.69768315121407E-11));
#17725=CARTESIAN_POINT('Ctrl Pts',(-7.07057502871922,-103.103019107145,
4.08219839617346));
#17726=CARTESIAN_POINT('Ctrl Pts',(-4.71371668580301,-102.928019107145,
8.16439679232994));
#17727=CARTESIAN_POINT('Ctrl Pts',(1.47018674401621E-11,-102.753019107145,
8.16439679232146));
#17728=CARTESIAN_POINT('Ctrl Pts',(4.71371668583241,-102.578019107145,8.16439679231297));
#17729=CARTESIAN_POINT('Ctrl Pts',(7.07057502873392,-102.403019107145,4.082198396148));
#17730=CARTESIAN_POINT('Ctrl Pts',(9.42743337163542,-102.228019107145,-1.69756769845304E-11));
#17731=CARTESIAN_POINT('Ctrl Pts',(7.07057502871922,-102.053019107145,-4.08219839617346));
#17732=CARTESIAN_POINT('Ctrl Pts',(4.71371668580301,-101.878019107145,-8.16439679232994));
#17733=CARTESIAN_POINT('Ctrl Pts',(-1.4702867290402E-11,-101.703019107145,
-8.16439679232146));
#17734=CARTESIAN_POINT('Ctrl Pts',(-4.71371668583241,-101.528019107145,
-8.16439679231297));
#17735=CARTESIAN_POINT('Ctrl Pts',(-7.07057502873392,-101.353019107145,
-4.082198396148));
#17736=CARTESIAN_POINT('Ctrl Pts',(-9.42743337163542,-101.178019107145,
1.69768315121407E-11));
#17737=CARTESIAN_POINT('Ctrl Pts',(-7.07057502871922,-101.003019107145,
4.08219839617346));
#17738=CARTESIAN_POINT('Ctrl Pts',(-4.71371668580301,-100.828019107145,
8.16439679232994));
#17739=CARTESIAN_POINT('Ctrl Pts',(1.47018674401621E-11,-100.653019107145,
8.16439679232146));
#17740=CARTESIAN_POINT('Ctrl Pts',(4.71371668583241,-100.478019107145,8.16439679231297));
#17741=CARTESIAN_POINT('Ctrl Pts',(7.07057502873392,-100.303019107145,4.082198396148));
#17742=CARTESIAN_POINT('Ctrl Pts',(9.42743337163542,-100.128019107145,-1.69756769845304E-11));
#17743=CARTESIAN_POINT('Ctrl Pts',(7.07057502871922,-99.953019107145,-4.08219839617346));
#17744=CARTESIAN_POINT('Ctrl Pts',(4.71371668580301,-99.7780191071449,-8.16439679232994));
#17745=CARTESIAN_POINT('Ctrl Pts',(-1.4702867290402E-11,-99.6030191071449,
-8.16439679232146));
#17746=CARTESIAN_POINT('Ctrl Pts',(-4.71371668583241,-99.4280191071449,
-8.16439679231297));
#17747=CARTESIAN_POINT('Ctrl Pts',(-7.07057502873392,-99.253019107145,-4.082198396148));
#17748=CARTESIAN_POINT('Ctrl Pts',(-9.42743337163542,-99.078019107145,1.69768315121407E-11));
#17749=CARTESIAN_POINT('Ctrl Pts',(-7.07057502871922,-98.903019107145,4.08219839617346));
#17750=CARTESIAN_POINT('Ctrl Pts',(-4.71371668580301,-98.7280191071449,
8.16439679232994));
#17751=CARTESIAN_POINT('Ctrl Pts',(1.47018674401621E-11,-98.5530191071449,
8.16439679232146));
#17752=CARTESIAN_POINT('Ctrl Pts',(4.71371668583241,-98.378019107145,8.16439679231297));
#17753=CARTESIAN_POINT('Ctrl Pts',(7.07057502873392,-98.2030191071449,4.082198396148));
#17754=CARTESIAN_POINT('Ctrl Pts',(9.42743337163542,-98.0280191071449,-1.69756769845304E-11));
#17755=CARTESIAN_POINT('Ctrl Pts',(7.07057502871922,-97.8530191071449,-4.08219839617346));
#17756=CARTESIAN_POINT('Ctrl Pts',(4.71371668580301,-97.6780191071449,-8.16439679232994));
#17757=CARTESIAN_POINT('Ctrl Pts',(-1.4702867290402E-11,-97.503019107145,
-8.16439679232146));
#17758=CARTESIAN_POINT('Ctrl Pts',(-4.71371668583241,-97.328019107145,-8.16439679231297));
#17759=CARTESIAN_POINT('Ctrl Pts',(-7.07057502873392,-97.153019107145,-4.082198396148));
#17760=CARTESIAN_POINT('Ctrl Pts',(-9.42743337163542,-96.978019107145,1.69768315121407E-11));
#17761=CARTESIAN_POINT('Ctrl Pts',(-7.07057502871922,-96.803019107145,4.08219839617346));
#17762=CARTESIAN_POINT('Ctrl Pts',(-4.71371668580301,-96.6280191071449,
8.16439679232994));
#17763=CARTESIAN_POINT('Ctrl Pts',(1.47018674401621E-11,-96.453019107145,
8.16439679232146));
#17764=CARTESIAN_POINT('Ctrl Pts',(4.71371668583241,-96.278019107145,8.16439679231297));
#17765=CARTESIAN_POINT('Ctrl Pts',(7.07057502873392,-96.103019107145,4.082198396148));
#17766=CARTESIAN_POINT('Ctrl Pts',(9.42743337163542,-95.928019107145,-1.69756769845304E-11));
#17767=CARTESIAN_POINT('Ctrl Pts',(7.07057502871922,-95.753019107145,-4.08219839617346));
#17768=CARTESIAN_POINT('Ctrl Pts',(4.71371668580301,-95.5780191071449,-8.16439679232994));
#17769=CARTESIAN_POINT('Ctrl Pts',(-1.4702867290402E-11,-95.403019107145,
-8.16439679232146));
#17770=CARTESIAN_POINT('Ctrl Pts',(-4.71371668583241,-95.228019107145,-8.16439679231297));
#17771=CARTESIAN_POINT('Ctrl Pts',(-7.07057502873392,-95.053019107145,-4.082198396148));
#17772=CARTESIAN_POINT('Ctrl Pts',(-9.42743337163542,-94.8780191071449,
1.69768315121407E-11));
#17773=CARTESIAN_POINT('Ctrl Pts',(-7.07057502871922,-94.703019107145,4.08219839617346));
#17774=CARTESIAN_POINT('Ctrl Pts',(-4.71371668580301,-94.528019107145,8.16439679232994));
#17775=CARTESIAN_POINT('Ctrl Pts',(1.47018674401621E-11,-94.3530191071449,
8.16439679232146));
#17776=CARTESIAN_POINT('Ctrl Pts',(4.71371668583241,-94.178019107145,8.16439679231297));
#17777=CARTESIAN_POINT('Ctrl Pts',(7.07057502873392,-94.003019107145,4.082198396148));
#17778=CARTESIAN_POINT('Ctrl Pts',(9.42743337163542,-93.8280191071449,-1.69756769845304E-11));
#17779=CARTESIAN_POINT('Ctrl Pts',(7.07057502871922,-93.6530191071449,-4.08219839617346));
#17780=CARTESIAN_POINT('Ctrl Pts',(4.71371668580301,-93.4780191071449,-8.16439679232994));
#17781=CARTESIAN_POINT('Ctrl Pts',(-1.4702867290402E-11,-93.3030191071449,
-8.16439679232146));
#17782=CARTESIAN_POINT('Ctrl Pts',(-4.71371668583241,-93.128019107145,-8.16439679231297));
#17783=CARTESIAN_POINT('Ctrl Pts',(-7.07057502873392,-92.953019107145,-4.082198396148));
#17784=CARTESIAN_POINT('Ctrl Pts',(-9.42743337163542,-92.7780191071449,
1.69768315121407E-11));
#17785=CARTESIAN_POINT('Ctrl Pts',(-7.07057502871922,-92.6030191071449,
4.08219839617346));
#17786=CARTESIAN_POINT('Ctrl Pts',(-4.71371668580301,-92.428019107145,8.16439679232994));
#17787=CARTESIAN_POINT('Ctrl Pts',(1.47018674401621E-11,-92.253019107145,
8.16439679232146));
#17788=CARTESIAN_POINT('Ctrl Pts',(4.71371668583241,-92.0780191071449,8.16439679231297));
#17789=CARTESIAN_POINT('Ctrl Pts',(7.07057502873392,-91.903019107145,4.082198396148));
#17790=CARTESIAN_POINT('Ctrl Pts',(9.42743337163542,-91.728019107145,-1.69756769845304E-11));
#17791=CARTESIAN_POINT('Ctrl Pts',(7.07057502871922,-91.553019107145,-4.08219839617346));
#17792=CARTESIAN_POINT('Ctrl Pts',(4.71371668580301,-91.378019107145,-8.16439679232994));
#17793=CARTESIAN_POINT('Ctrl Pts',(-1.4702867290402E-11,-91.203019107145,
-8.16439679232146));
#17794=CARTESIAN_POINT('Ctrl Pts',(-4.71371668583241,-91.028019107145,-8.16439679231297));
#17795=CARTESIAN_POINT('Ctrl Pts',(-7.07057502873392,-90.853019107145,-4.082198396148));
#17796=CARTESIAN_POINT('Ctrl Pts',(-9.42743337163542,-90.678019107145,1.69768315121407E-11));
#17797=CARTESIAN_POINT('Ctrl Pts',(-7.07057502871922,-90.503019107145,4.08219839617346));
#17798=CARTESIAN_POINT('Ctrl Pts',(-4.71371668580301,-90.328019107145,8.16439679232994));
#17799=CARTESIAN_POINT('Ctrl Pts',(1.47018674401621E-11,-90.153019107145,
8.16439679232146));
#17800=CARTESIAN_POINT('Ctrl Pts',(4.71371668583241,-89.978019107145,8.16439679231297));
#17801=CARTESIAN_POINT('Ctrl Pts',(7.07057502873392,-89.803019107145,4.082198396148));
#17802=CARTESIAN_POINT('Ctrl Pts',(9.42743337163542,-89.628019107145,-1.69756769845304E-11));
#17803=CARTESIAN_POINT('Ctrl Pts',(7.07057502871922,-89.4530191071449,-4.08219839617346));
#17804=CARTESIAN_POINT('Ctrl Pts',(4.71371668580301,-89.278019107145,-8.16439679232994));
#17805=CARTESIAN_POINT('Ctrl Pts',(-1.4702867290402E-11,-89.103019107145,
-8.16439679232146));
#17806=CARTESIAN_POINT('Ctrl Pts',(-4.71371668583241,-88.9280191071449,
-8.16439679231297));
#17807=CARTESIAN_POINT('Ctrl Pts',(-7.07057502873392,-88.753019107145,-4.082198396148));
#17808=CARTESIAN_POINT('Ctrl Pts',(-9.42743337163542,-88.578019107145,1.69768315121407E-11));
#17809=CARTESIAN_POINT('Ctrl Pts',(-7.07057502871922,-88.403019107145,4.08219839617346));
#17810=CARTESIAN_POINT('Ctrl Pts',(-4.71371668580301,-88.228019107145,8.16439679232994));
#17811=CARTESIAN_POINT('Ctrl Pts',(1.47018674401621E-11,-88.053019107145,
8.16439679232146));
#17812=CARTESIAN_POINT('Ctrl Pts',(4.71371668583241,-87.878019107145,8.16439679231297));
#17813=CARTESIAN_POINT('Ctrl Pts',(7.07057502873392,-87.703019107145,4.082198396148));
#17814=CARTESIAN_POINT('Ctrl Pts',(9.42743337163542,-87.528019107145,-1.69756769845304E-11));
#17815=CARTESIAN_POINT('Ctrl Pts',(7.07057502871922,-87.353019107145,-4.08219839617346));
#17816=CARTESIAN_POINT('Ctrl Pts',(4.71371668580301,-87.178019107145,-8.16439679232994));
#17817=CARTESIAN_POINT('Ctrl Pts',(-1.4702867290402E-11,-87.003019107145,
-8.16439679232146));
#17818=CARTESIAN_POINT('Ctrl Pts',(-4.71371668583241,-86.828019107145,-8.16439679231297));
#17819=CARTESIAN_POINT('Ctrl Pts',(-7.07057502873392,-86.653019107145,-4.082198396148));
#17820=CARTESIAN_POINT('Ctrl Pts',(-9.42743337163542,-86.478019107145,1.69768315121407E-11));
#17821=CARTESIAN_POINT('Ctrl Pts',(-7.07057502871922,-86.303019107145,4.08219839617346));
#17822=CARTESIAN_POINT('Ctrl Pts',(-4.71371668580301,-86.128019107145,8.16439679232994));
#17823=CARTESIAN_POINT('Ctrl Pts',(1.47018674401621E-11,-85.953019107145,
8.16439679232146));
#17824=CARTESIAN_POINT('Ctrl Pts',(4.71371668583241,-85.778019107145,8.16439679231297));
#17825=CARTESIAN_POINT('Ctrl Pts',(7.07057502873392,-85.603019107145,4.082198396148));
#17826=CARTESIAN_POINT('Ctrl Pts',(9.42743337163542,-85.428019107145,-1.69756769845304E-11));
#17827=CARTESIAN_POINT('Ctrl Pts',(7.07057502871922,-85.253019107145,-4.08219839617346));
#17828=CARTESIAN_POINT('Ctrl Pts',(4.71371668580301,-85.078019107145,-8.16439679232994));
#17829=CARTESIAN_POINT('Ctrl Pts',(-1.4702867290402E-11,-84.903019107145,
-8.16439679232146));
#17830=CARTESIAN_POINT('Ctrl Pts',(-4.71371668583241,-84.728019107145,-8.16439679231297));
#17831=CARTESIAN_POINT('Ctrl Pts',(-7.07057502873392,-84.553019107145,-4.082198396148));
#17832=CARTESIAN_POINT('Ctrl Pts',(-9.42743337163542,-84.378019107145,1.69768315121407E-11));
#17833=CARTESIAN_POINT('Ctrl Pts',(-7.07057502871922,-84.203019107145,4.08219839617346));
#17834=CARTESIAN_POINT('Ctrl Pts',(-4.71371668580301,-84.028019107145,8.16439679232994));
#17835=CARTESIAN_POINT('Ctrl Pts',(1.47018674401621E-11,-83.853019107145,
8.16439679232146));
#17836=CARTESIAN_POINT('Ctrl Pts',(4.71371668583241,-83.678019107145,8.16439679231297));
#17837=CARTESIAN_POINT('Ctrl Pts',(7.07057502873392,-83.503019107145,4.082198396148));
#17838=CARTESIAN_POINT('Ctrl Pts',(9.42743337163542,-83.328019107145,-1.69756769845304E-11));
#17839=CARTESIAN_POINT('Ctrl Pts',(7.07057502871922,-83.153019107145,-4.08219839617346));
#17840=CARTESIAN_POINT('Ctrl Pts',(4.71371668580301,-82.978019107145,-8.16439679232994));
#17841=CARTESIAN_POINT('Ctrl Pts',(-1.4702867290402E-11,-82.803019107145,
-8.16439679232146));
#17842=CARTESIAN_POINT('Ctrl Pts',(-4.71371668583241,-82.628019107145,-8.16439679231297));
#17843=CARTESIAN_POINT('Ctrl Pts',(-7.07057502873392,-82.453019107145,-4.082198396148));
#17844=CARTESIAN_POINT('Ctrl Pts',(-9.42743337163542,-82.278019107145,1.69768315121407E-11));
#17845=CARTESIAN_POINT('Ctrl Pts',(-7.07057502871922,-82.103019107145,4.08219839617346));
#17846=CARTESIAN_POINT('Ctrl Pts',(-4.71371668580301,-81.928019107145,8.16439679232994));
#17847=CARTESIAN_POINT('Ctrl Pts',(1.47018674401621E-11,-81.753019107145,
8.16439679232146));
#17848=CARTESIAN_POINT('Ctrl Pts',(4.71371668583241,-81.578019107145,8.16439679231297));
#17849=CARTESIAN_POINT('Ctrl Pts',(7.07057502873392,-81.403019107145,4.082198396148));
#17850=CARTESIAN_POINT('Ctrl Pts',(9.42743337163542,-81.228019107145,-1.69756769845304E-11));
#17851=CARTESIAN_POINT('Ctrl Pts',(7.07057502871922,-81.053019107145,-4.08219839617346));
#17852=CARTESIAN_POINT('Ctrl Pts',(4.71371668580301,-80.878019107145,-8.16439679232994));
#17853=CARTESIAN_POINT('Ctrl Pts',(-1.4702867290402E-11,-80.703019107145,
-8.16439679232146));
#17854=CARTESIAN_POINT('Ctrl Pts',(-4.71371668583241,-80.528019107145,-8.16439679231297));
#17855=CARTESIAN_POINT('Ctrl Pts',(-7.07057502873392,-80.353019107145,-4.082198396148));
#17856=CARTESIAN_POINT('Ctrl Pts',(-9.42743337163542,-80.178019107145,1.69768315121407E-11));
#17857=CARTESIAN_POINT('Ctrl Pts',(-7.07057502871922,-80.003019107145,4.08219839617346));
#17858=CARTESIAN_POINT('Ctrl Pts',(-4.71371668580301,-79.828019107145,8.16439679232994));
#17859=CARTESIAN_POINT('Ctrl Pts',(1.47018674401621E-11,-79.653019107145,
8.16439679232146));
#17860=CARTESIAN_POINT('Ctrl Pts',(4.71371668583241,-79.478019107145,8.16439679231297));
#17861=CARTESIAN_POINT('Ctrl Pts',(7.07057502873392,-79.303019107145,4.082198396148));
#17862=CARTESIAN_POINT('Ctrl Pts',(9.42743337163542,-79.128019107145,-1.69756769845304E-11));
#17863=CARTESIAN_POINT('Ctrl Pts',(7.07057502871922,-78.953019107145,-4.08219839617346));
#17864=CARTESIAN_POINT('Ctrl Pts',(4.71371668580301,-78.778019107145,-8.16439679232994));
#17865=CARTESIAN_POINT('Ctrl Pts',(-1.4702867290402E-11,-78.603019107145,
-8.16439679232146));
#17866=CARTESIAN_POINT('Ctrl Pts',(-4.71371668583241,-78.428019107145,-8.16439679231297));
#17867=CARTESIAN_POINT('Ctrl Pts',(-7.07057502873392,-78.253019107145,-4.082198396148));
#17868=CARTESIAN_POINT('Ctrl Pts',(-9.42743337163542,-78.078019107145,1.69768315121407E-11));
#17869=CARTESIAN_POINT('Ctrl Pts',(-7.07057502871922,-77.903019107145,4.08219839617346));
#17870=CARTESIAN_POINT('Ctrl Pts',(-4.71371668580301,-77.728019107145,8.16439679232994));
#17871=CARTESIAN_POINT('Ctrl Pts',(1.47018674401621E-11,-77.553019107145,
8.16439679232146));
#17872=CARTESIAN_POINT('Ctrl Pts',(4.71371668583241,-77.378019107145,8.16439679231297));
#17873=CARTESIAN_POINT('Ctrl Pts',(7.07057502873392,-77.203019107145,4.082198396148));
#17874=CARTESIAN_POINT('Ctrl Pts',(9.42743337163542,-77.028019107145,-1.69756769845304E-11));
#17875=CARTESIAN_POINT('Ctrl Pts',(7.07057502871922,-76.853019107145,-4.08219839617346));
#17876=CARTESIAN_POINT('Ctrl Pts',(4.71371668580301,-76.678019107145,-8.16439679232994));
#17877=CARTESIAN_POINT('Ctrl Pts',(-1.4702867290402E-11,-76.503019107145,
-8.16439679232146));
#17878=CARTESIAN_POINT('Ctrl Pts',(-4.71371668583241,-76.328019107145,-8.16439679231297));
#17879=CARTESIAN_POINT('Ctrl Pts',(-7.07057502873392,-76.153019107145,-4.082198396148));
#17880=CARTESIAN_POINT('Ctrl Pts',(-9.42743337163542,-75.978019107145,1.69768315121407E-11));
#17881=CARTESIAN_POINT('Ctrl Pts',(-7.07057502871922,-75.803019107145,4.08219839617346));
#17882=CARTESIAN_POINT('Ctrl Pts',(-4.71371668580301,-75.628019107145,8.16439679232994));
#17883=CARTESIAN_POINT('Ctrl Pts',(1.47018674401621E-11,-75.453019107145,
8.16439679232146));
#17884=CARTESIAN_POINT('Ctrl Pts',(4.71371668583241,-75.278019107145,8.16439679231297));
#17885=CARTESIAN_POINT('Ctrl Pts',(7.07057502873392,-75.103019107145,4.082198396148));
#17886=CARTESIAN_POINT('Ctrl Pts',(9.42743337163542,-74.928019107145,-1.69756769845304E-11));
#17887=CARTESIAN_POINT('Ctrl Pts',(7.07057502871922,-74.753019107145,-4.08219839617346));
#17888=CARTESIAN_POINT('Ctrl Pts',(4.71371668580301,-74.578019107145,-8.16439679232994));
#17889=CARTESIAN_POINT('Ctrl Pts',(-1.4702867290402E-11,-74.403019107145,
-8.16439679232146));
#17890=CARTESIAN_POINT('Ctrl Pts',(-4.71371668583241,-74.228019107145,-8.16439679231297));
#17891=CARTESIAN_POINT('Ctrl Pts',(-7.07057502873392,-74.053019107145,-4.082198396148));
#17892=CARTESIAN_POINT('Ctrl Pts',(-9.42743337163542,-73.878019107145,1.69768315121407E-11));
#17893=CARTESIAN_POINT('Ctrl Pts',(-7.07057502871922,-73.703019107145,4.08219839617346));
#17894=CARTESIAN_POINT('Ctrl Pts',(-4.71371668580301,-73.528019107145,8.16439679232994));
#17895=CARTESIAN_POINT('Ctrl Pts',(1.47018674401621E-11,-73.353019107145,
8.16439679232146));
#17896=CARTESIAN_POINT('Ctrl Pts',(4.71371668583241,-73.178019107145,8.16439679231297));
#17897=CARTESIAN_POINT('Ctrl Pts',(7.07057502873392,-73.003019107145,4.082198396148));
#17898=CARTESIAN_POINT('Ctrl Pts',(9.42743337163542,-72.828019107145,-1.69756769845304E-11));
#17899=CARTESIAN_POINT('Ctrl Pts',(7.07057502871922,-72.653019107145,-4.08219839617346));
#17900=CARTESIAN_POINT('Ctrl Pts',(4.71371668580301,-72.478019107145,-8.16439679232994));
#17901=CARTESIAN_POINT('Ctrl Pts',(-1.4702867290402E-11,-72.303019107145,
-8.16439679232146));
#17902=CARTESIAN_POINT('Ctrl Pts',(-4.71371668583241,-72.128019107145,-8.16439679231297));
#17903=CARTESIAN_POINT('Ctrl Pts',(-7.07057502873392,-71.953019107145,-4.082198396148));
#17904=CARTESIAN_POINT('Ctrl Pts',(-9.42743337163542,-71.778019107145,1.69768315121407E-11));
#17905=CARTESIAN_POINT('Ctrl Pts',(-7.07057502871922,-71.603019107145,4.08219839617346));
#17906=CARTESIAN_POINT('Ctrl Pts',(-4.71371668580301,-71.428019107145,8.16439679232994));
#17907=CARTESIAN_POINT('Ctrl Pts',(1.47018674401621E-11,-71.253019107145,
8.16439679232146));
#17908=CARTESIAN_POINT('Ctrl Pts',(4.71371668583241,-71.078019107145,8.16439679231297));
#17909=CARTESIAN_POINT('Ctrl Pts',(7.07057502873392,-70.903019107145,4.082198396148));
#17910=CARTESIAN_POINT('Ctrl Pts',(9.42743337163542,-70.728019107145,-1.69756769845304E-11));
#17911=CARTESIAN_POINT('Ctrl Pts',(7.07057502871922,-70.553019107145,-4.08219839617346));
#17912=CARTESIAN_POINT('Ctrl Pts',(4.71371668580301,-70.378019107145,-8.16439679232994));
#17913=CARTESIAN_POINT('Ctrl Pts',(-1.4702867290402E-11,-70.203019107145,
-8.16439679232146));
#17914=CARTESIAN_POINT('Ctrl Pts',(-4.71371668583241,-70.028019107145,-8.16439679231297));
#17915=CARTESIAN_POINT('Ctrl Pts',(-7.07057502873392,-69.853019107145,-4.082198396148));
#17916=CARTESIAN_POINT('Ctrl Pts',(-9.42743337163542,-69.678019107145,1.69768315121407E-11));
#17917=CARTESIAN_POINT('Ctrl Pts',(-7.07057502871922,-69.503019107145,4.08219839617346));
#17918=CARTESIAN_POINT('Ctrl Pts',(-4.71371668580301,-69.328019107145,8.16439679232994));
#17919=CARTESIAN_POINT('Ctrl Pts',(1.47018674401621E-11,-69.153019107145,
8.16439679232146));
#17920=CARTESIAN_POINT('Ctrl Pts',(4.71371668583241,-68.978019107145,8.16439679231297));
#17921=CARTESIAN_POINT('Ctrl Pts',(7.07057502873392,-68.803019107145,4.082198396148));
#17922=CARTESIAN_POINT('Ctrl Pts',(9.42743337163542,-68.6280191071451,-1.69756769845304E-11));
#17923=CARTESIAN_POINT('Ctrl Pts',(7.07057502871922,-68.453019107145,-4.08219839617346));
#17924=CARTESIAN_POINT('Ctrl Pts',(4.71371668580301,-68.278019107145,-8.16439679232994));
#17925=CARTESIAN_POINT('Ctrl Pts',(-1.4702867290402E-11,-68.103019107145,
-8.16439679232146));
#17926=CARTESIAN_POINT('Ctrl Pts',(-4.71371668583241,-67.928019107145,-8.16439679231297));
#17927=CARTESIAN_POINT('Ctrl Pts',(-7.07057502873392,-67.753019107145,-4.082198396148));
#17928=CARTESIAN_POINT('Ctrl Pts',(-9.42743337163542,-67.5780191071451,
1.69768315121407E-11));
#17929=CARTESIAN_POINT('Ctrl Pts',(-7.07057502871922,-67.403019107145,4.08219839617346));
#17930=CARTESIAN_POINT('Ctrl Pts',(-4.71371668580301,-67.228019107145,8.16439679232994));
#17931=CARTESIAN_POINT('Ctrl Pts',(1.47018674401621E-11,-67.053019107145,
8.16439679232146));
#17932=CARTESIAN_POINT('Ctrl Pts',(4.71371668583241,-66.878019107145,8.16439679231297));
#17933=CARTESIAN_POINT('Ctrl Pts',(7.07057502873392,-66.703019107145,4.082198396148));
#17934=CARTESIAN_POINT('Ctrl Pts',(9.42743337163542,-66.5280191071451,-1.69756769845304E-11));
#17935=CARTESIAN_POINT('Ctrl Pts',(7.07057502871922,-66.353019107145,-4.08219839617346));
#17936=CARTESIAN_POINT('Ctrl Pts',(4.71371668580301,-66.178019107145,-8.16439679232994));
#17937=CARTESIAN_POINT('Ctrl Pts',(-1.4702867290402E-11,-66.003019107145,
-8.16439679232146));
#17938=CARTESIAN_POINT('Ctrl Pts',(-4.71371668583241,-65.828019107145,-8.16439679231297));
#17939=CARTESIAN_POINT('Ctrl Pts',(-7.07057502873392,-65.653019107145,-4.082198396148));
#17940=CARTESIAN_POINT('Ctrl Pts',(-9.42743337163542,-65.478019107145,1.69768315121407E-11));
#17941=CARTESIAN_POINT('Ctrl Pts',(-7.07057502871922,-65.303019107145,4.08219839617346));
#17942=CARTESIAN_POINT('Ctrl Pts',(-4.71371668580301,-65.1280191071451,
8.16439679232994));
#17943=CARTESIAN_POINT('Ctrl Pts',(1.47018674401621E-11,-64.953019107145,
8.16439679232146));
#17944=CARTESIAN_POINT('Ctrl Pts',(4.71371668583241,-64.778019107145,8.16439679231297));
#17945=CARTESIAN_POINT('Ctrl Pts',(7.07057502873392,-64.603019107145,4.082198396148));
#17946=CARTESIAN_POINT('Ctrl Pts',(9.42743337163542,-64.428019107145,-1.69756769845304E-11));
#17947=CARTESIAN_POINT('Ctrl Pts',(7.07057502871922,-64.253019107145,-4.08219839617346));
#17948=CARTESIAN_POINT('Ctrl Pts',(4.71371668580301,-64.0780191071451,-8.16439679232994));
#17949=CARTESIAN_POINT('Ctrl Pts',(-1.4702867290402E-11,-63.903019107145,
-8.16439679232146));
#17950=CARTESIAN_POINT('Ctrl Pts',(-4.71371668583241,-63.728019107145,-8.16439679231297));
#17951=CARTESIAN_POINT('Ctrl Pts',(-7.07057502873392,-63.553019107145,-4.082198396148));
#17952=CARTESIAN_POINT('Ctrl Pts',(-9.42743337163542,-63.378019107145,1.69768315121407E-11));
#17953=CARTESIAN_POINT('Ctrl Pts',(-7.07057502871922,-63.203019107145,4.08219839617346));
#17954=CARTESIAN_POINT('Ctrl Pts',(-4.71371668580301,-63.028019107145,8.16439679232994));
#17955=CARTESIAN_POINT('Ctrl Pts',(1.47018674401621E-11,-62.853019107145,
8.16439679232146));
#17956=CARTESIAN_POINT('Ctrl Pts',(4.71371668583241,-62.678019107145,8.16439679231297));
#17957=CARTESIAN_POINT('Ctrl Pts',(7.07057502873392,-62.503019107145,4.082198396148));
#17958=CARTESIAN_POINT('Ctrl Pts',(9.42743337163542,-62.328019107145,-1.69756769845304E-11));
#17959=CARTESIAN_POINT('Ctrl Pts',(7.07057502871922,-62.153019107145,-4.08219839617346));
#17960=CARTESIAN_POINT('Ctrl Pts',(4.71371668580301,-61.978019107145,-8.16439679232994));
#17961=CARTESIAN_POINT('Ctrl Pts',(-1.4702867290402E-11,-61.803019107145,
-8.16439679232146));
#17962=CARTESIAN_POINT('Ctrl Pts',(-4.71371668583241,-61.628019107145,-8.16439679231297));
#17963=CARTESIAN_POINT('Ctrl Pts',(-7.07057502873392,-61.453019107145,-4.082198396148));
#17964=CARTESIAN_POINT('Ctrl Pts',(-9.42743337163542,-61.278019107145,1.69768315121407E-11));
#17965=CARTESIAN_POINT('Ctrl Pts',(-7.07057502871922,-61.103019107145,4.08219839617346));
#17966=CARTESIAN_POINT('Ctrl Pts',(-4.71371668580301,-60.9280191071451,
8.16439679232994));
#17967=CARTESIAN_POINT('Ctrl Pts',(1.47018674401621E-11,-60.753019107145,
8.16439679232146));
#17968=CARTESIAN_POINT('Ctrl Pts',(4.71371668583241,-60.578019107145,8.16439679231297));
#17969=CARTESIAN_POINT('Ctrl Pts',(7.07057502873392,-60.403019107145,4.082198396148));
#17970=CARTESIAN_POINT('Ctrl Pts',(9.42743337163542,-60.228019107145,-1.69756769845304E-11));
#17971=CARTESIAN_POINT('Ctrl Pts',(7.07057502871922,-60.053019107145,-4.08219839617346));
#17972=CARTESIAN_POINT('Ctrl Pts',(4.71371668580301,-59.8780191071451,-8.16439679232994));
#17973=CARTESIAN_POINT('Ctrl Pts',(-1.4702867290402E-11,-59.703019107145,
-8.16439679232146));
#17974=CARTESIAN_POINT('Ctrl Pts',(-4.71371668583241,-59.528019107145,-8.16439679231297));
#17975=CARTESIAN_POINT('Ctrl Pts',(-7.07057502873392,-59.3530191071451,
-4.082198396148));
#17976=CARTESIAN_POINT('Ctrl Pts',(-9.42743337163542,-59.178019107145,1.69768315121407E-11));
#17977=CARTESIAN_POINT('Ctrl Pts',(-7.07057502871922,-59.003019107145,4.08219839617346));
#17978=CARTESIAN_POINT('Ctrl Pts',(-4.71371668580301,-58.8280191071451,
8.16439679232994));
#17979=CARTESIAN_POINT('Ctrl Pts',(1.47018674401621E-11,-58.653019107145,
8.16439679232146));
#17980=CARTESIAN_POINT('Ctrl Pts',(4.71371668583241,-58.478019107145,8.16439679231297));
#17981=CARTESIAN_POINT('Ctrl Pts',(7.07057502873392,-58.303019107145,4.082198396148));
#17982=CARTESIAN_POINT('Ctrl Pts',(9.42743337163542,-58.128019107145,-1.69756769845304E-11));
#17983=CARTESIAN_POINT('Ctrl Pts',(7.07057502871922,-57.953019107145,-4.08219839617346));
#17984=CARTESIAN_POINT('Ctrl Pts',(4.71371668580301,-57.7780191071451,-8.16439679232994));
#17985=CARTESIAN_POINT('Ctrl Pts',(-1.4702867290402E-11,-57.603019107145,
-8.16439679232146));
#17986=CARTESIAN_POINT('Ctrl Pts',(-4.71371668583241,-57.428019107145,-8.16439679231297));
#17987=CARTESIAN_POINT('Ctrl Pts',(-7.07057502873392,-57.253019107145,-4.082198396148));
#17988=CARTESIAN_POINT('Ctrl Pts',(-9.42743337163542,-57.078019107145,1.69768315121407E-11));
#17989=CARTESIAN_POINT('Ctrl Pts',(-7.07057502871922,-56.903019107145,4.08219839617346));
#17990=CARTESIAN_POINT('Ctrl Pts',(-4.71371668580301,-56.728019107145,8.16439679232994));
#17991=CARTESIAN_POINT('Ctrl Pts',(1.47018674401621E-11,-56.553019107145,
8.16439679232146));
#17992=CARTESIAN_POINT('Ctrl Pts',(4.71371668583241,-56.3780191071451,8.16439679231297));
#17993=CARTESIAN_POINT('Ctrl Pts',(7.07057502873392,-56.203019107145,4.082198396148));
#17994=CARTESIAN_POINT('Ctrl Pts',(9.42743337163542,-56.028019107145,-1.69756769845304E-11));
#17995=CARTESIAN_POINT('Ctrl Pts',(7.07057502871922,-55.8530191071451,-4.08219839617346));
#17996=CARTESIAN_POINT('Ctrl Pts',(4.71371668580301,-55.678019107145,-8.16439679232994));
#17997=CARTESIAN_POINT('Ctrl Pts',(-1.4702867290402E-11,-55.503019107145,
-8.16439679232146));
#17998=CARTESIAN_POINT('Ctrl Pts',(-4.71371668583241,-55.3280191071451,
-8.16439679231297));
#17999=CARTESIAN_POINT('Ctrl Pts',(-7.07057502873392,-55.153019107145,-4.082198396148));
#18000=CARTESIAN_POINT('Ctrl Pts',(-9.42743337163542,-54.9780191071451,
1.69768315121407E-11));
#18001=CARTESIAN_POINT('Ctrl Pts',(-7.07057502871922,-54.8030191071451,
4.08219839617346));
#18002=CARTESIAN_POINT('Ctrl Pts',(-4.71371668580301,-54.628019107145,8.16439679232994));
#18003=CARTESIAN_POINT('Ctrl Pts',(1.47018674401621E-11,-54.453019107145,
8.16439679232146));
#18004=CARTESIAN_POINT('Ctrl Pts',(4.71371668583241,-54.278019107145,8.16439679231297));
#18005=CARTESIAN_POINT('Ctrl Pts',(7.07057502873392,-54.1030191071451,4.082198396148));
#18006=CARTESIAN_POINT('Ctrl Pts',(9.42743337163542,-53.9280191071451,-1.69756769845304E-11));
#18007=CARTESIAN_POINT('Ctrl Pts',(7.07057502871922,-53.7530191071451,-4.08219839617346));
#18008=CARTESIAN_POINT('Ctrl Pts',(4.71371668580301,-53.5780191071451,-8.16439679232994));
#18009=CARTESIAN_POINT('Ctrl Pts',(-1.4702867290402E-11,-53.403019107145,
-8.16439679232146));
#18010=CARTESIAN_POINT('Ctrl Pts',(-4.71371668583241,-53.228019107145,-8.16439679231297));
#18011=CARTESIAN_POINT('Ctrl Pts',(-7.07057502873392,-53.0530191071451,
-4.082198396148));
#18012=CARTESIAN_POINT('Ctrl Pts',(-9.42743337163542,-52.878019107145,1.69768315121407E-11));
#18013=CARTESIAN_POINT('Ctrl Pts',(-7.07057502871922,-52.703019107145,4.08219839617346));
#18014=CARTESIAN_POINT('Ctrl Pts',(-4.71371668580301,-52.528019107145,8.16439679232994));
#18015=CARTESIAN_POINT('Ctrl Pts',(1.47018674401621E-11,-52.3530191071451,
8.16439679232146));
#18016=CARTESIAN_POINT('Ctrl Pts',(4.71371668583241,-52.178019107145,8.16439679231297));
#18017=CARTESIAN_POINT('Ctrl Pts',(7.07057502873392,-52.0030191071451,4.082198396148));
#18018=CARTESIAN_POINT('Ctrl Pts',(9.42743337163542,-51.828019107145,-1.69756769845304E-11));
#18019=CARTESIAN_POINT('Ctrl Pts',(7.07057502871922,-51.6530191071451,-4.08219839617346));
#18020=CARTESIAN_POINT('Ctrl Pts',(4.71371668580301,-51.4780191071451,-8.16439679232994));
#18021=CARTESIAN_POINT('Ctrl Pts',(-1.4702867290402E-11,-51.303019107145,
-8.16439679232146));
#18022=CARTESIAN_POINT('Ctrl Pts',(-4.71371668583241,-51.1280191071451,
-8.16439679231297));
#18023=CARTESIAN_POINT('Ctrl Pts',(-7.07057502873392,-50.9530191071451,
-4.082198396148));
#18024=CARTESIAN_POINT('Ctrl Pts',(-9.42743337163542,-50.778019107145,1.69768315121407E-11));
#18025=CARTESIAN_POINT('Ctrl Pts',(-7.07057502871922,-50.6030191071451,
4.08219839617346));
#18026=CARTESIAN_POINT('Ctrl Pts',(-4.71371668580301,-50.4280191071451,
8.16439679232994));
#18027=CARTESIAN_POINT('Ctrl Pts',(1.47018674401621E-11,-50.253019107145,
8.16439679232146));
#18028=CARTESIAN_POINT('Ctrl Pts',(4.71371668583241,-50.0780191071451,8.16439679231297));
#18029=CARTESIAN_POINT('Ctrl Pts',(7.07057502873392,-49.9030191071451,4.082198396148));
#18030=CARTESIAN_POINT('Ctrl Pts',(9.42743337163542,-49.728019107145,-1.69756769845304E-11));
#18031=CARTESIAN_POINT('Ctrl Pts',(7.07057502871922,-49.5530191071451,-4.08219839617346));
#18032=CARTESIAN_POINT('Ctrl Pts',(4.71371668580301,-49.3780191071451,-8.16439679232994));
#18033=CARTESIAN_POINT('Ctrl Pts',(-1.4702867290402E-11,-49.2030191071451,
-8.16439679232146));
#18034=CARTESIAN_POINT('Ctrl Pts',(-4.71371668583241,-49.028019107145,-8.16439679231297));
#18035=CARTESIAN_POINT('Ctrl Pts',(-7.07057502873392,-48.853019107145,-4.082198396148));
#18036=CARTESIAN_POINT('Ctrl Pts',(-9.42743337163542,-48.6780191071451,
1.69768315121407E-11));
#18037=CARTESIAN_POINT('Ctrl Pts',(-7.07057502871922,-48.5030191071451,
4.08219839617346));
#18038=CARTESIAN_POINT('Ctrl Pts',(-4.71371668580301,-48.3280191071451,
8.16439679232994));
#18039=CARTESIAN_POINT('Ctrl Pts',(1.47018674401621E-11,-48.1530191071451,
8.16439679232146));
#18040=CARTESIAN_POINT('Ctrl Pts',(4.71371668583241,-47.9780191071451,8.16439679231297));
#18041=CARTESIAN_POINT('Ctrl Pts',(7.07057502873392,-47.8030191071451,4.082198396148));
#18042=CARTESIAN_POINT('Ctrl Pts',(9.42743337163542,-47.6280191071451,-1.69756769845304E-11));
#18043=CARTESIAN_POINT('Ctrl Pts',(7.07057502871922,-47.4530191071451,-4.08219839617346));
#18044=CARTESIAN_POINT('Ctrl Pts',(4.71371668580301,-47.2780191071451,-8.16439679232994));
#18045=CARTESIAN_POINT('Ctrl Pts',(-1.4702867290402E-11,-47.1030191071451,
-8.16439679232146));
#18046=CARTESIAN_POINT('Ctrl Pts',(-4.71371668583241,-46.9280191071451,
-8.16439679231297));
#18047=CARTESIAN_POINT('Ctrl Pts',(-7.07057502873392,-46.7530191071451,
-4.082198396148));
#18048=CARTESIAN_POINT('Ctrl Pts',(-9.42743337163542,-46.5780191071451,
1.69768315121407E-11));
#18049=CARTESIAN_POINT('Ctrl Pts',(-7.07057502871922,-46.4030191071451,
4.08219839617346));
#18050=CARTESIAN_POINT('Ctrl Pts',(-4.71371668580301,-46.2280191071451,
8.16439679232994));
#18051=CARTESIAN_POINT('Ctrl Pts',(1.47018674401621E-11,-46.0530191071451,
8.16439679232146));
#18052=CARTESIAN_POINT('Ctrl Pts',(4.71371668583241,-45.8780191071451,8.16439679231297));
#18053=CARTESIAN_POINT('Ctrl Pts',(7.07057502873392,-45.7030191071451,4.082198396148));
#18054=CARTESIAN_POINT('Ctrl Pts',(9.42743337163542,-45.5280191071451,-1.69756769845304E-11));
#18055=CARTESIAN_POINT('Ctrl Pts',(7.07057502871922,-45.3530191071451,-4.08219839617346));
#18056=CARTESIAN_POINT('Ctrl Pts',(4.71371668580301,-45.1780191071451,-8.16439679232994));
#18057=CARTESIAN_POINT('Ctrl Pts',(-1.4702867290402E-11,-45.0030191071451,
-8.16439679232146));
#18058=CARTESIAN_POINT('Ctrl Pts',(-4.71371668583241,-44.8280191071451,
-8.16439679231297));
#18059=CARTESIAN_POINT('Ctrl Pts',(-7.07057502873392,-44.6530191071451,
-4.082198396148));
#18060=CARTESIAN_POINT('Ctrl Pts',(-9.42743337163542,-44.4780191071451,
1.69768315121407E-11));
#18061=CARTESIAN_POINT('Ctrl Pts',(-7.07057502871922,-44.3030191071451,
4.08219839617346));
#18062=CARTESIAN_POINT('Ctrl Pts',(-4.71371668580301,-44.1280191071451,
8.16439679232994));
#18063=CARTESIAN_POINT('Ctrl Pts',(1.47018674401621E-11,-43.9530191071451,
8.16439679232146));
#18064=CARTESIAN_POINT('Ctrl Pts',(4.71371668583241,-43.7780191071451,8.16439679231297));
#18065=CARTESIAN_POINT('Ctrl Pts',(7.07057502873392,-43.6030191071451,4.082198396148));
#18066=CARTESIAN_POINT('Ctrl Pts',(9.42743337163542,-43.4280191071451,-1.69756769845304E-11));
#18067=CARTESIAN_POINT('Ctrl Pts',(7.07057502871922,-43.2530191071451,-4.08219839617346));
#18068=CARTESIAN_POINT('Ctrl Pts',(4.71371668580301,-43.0780191071451,-8.16439679232994));
#18069=CARTESIAN_POINT('Ctrl Pts',(-1.4702867290402E-11,-42.9030191071451,
-8.16439679232146));
#18070=CARTESIAN_POINT('Ctrl Pts',(-4.71371668583241,-42.7280191071451,
-8.16439679231297));
#18071=CARTESIAN_POINT('Ctrl Pts',(-7.07057502873392,-42.5530191071451,
-4.082198396148));
#18072=CARTESIAN_POINT('Ctrl Pts',(-9.42743337163542,-42.3780191071451,
1.69768315121407E-11));
#18073=CARTESIAN_POINT('Ctrl Pts',(-7.07057502871922,-42.2030191071451,
4.08219839617346));
#18074=CARTESIAN_POINT('Ctrl Pts',(-4.71371668580301,-42.0280191071451,
8.16439679232994));
#18075=CARTESIAN_POINT('Ctrl Pts',(1.47018674401621E-11,-41.8530191071451,
8.16439679232146));
#18076=CARTESIAN_POINT('Ctrl Pts',(4.71371668583241,-41.6780191071451,8.16439679231297));
#18077=CARTESIAN_POINT('Ctrl Pts',(7.07057502873392,-41.5030191071451,4.082198396148));
#18078=CARTESIAN_POINT('Ctrl Pts',(9.42743337163542,-41.3280191071451,-1.69756769845304E-11));
#18079=CARTESIAN_POINT('Ctrl Pts',(7.07057502871922,-41.1530191071451,-4.08219839617346));
#18080=CARTESIAN_POINT('Ctrl Pts',(4.71371668580301,-40.9780191071451,-8.16439679232994));
#18081=CARTESIAN_POINT('Ctrl Pts',(-1.4702867290402E-11,-40.8030191071451,
-8.16439679232146));
#18082=CARTESIAN_POINT('Ctrl Pts',(-4.71371668583241,-40.6280191071451,
-8.16439679231297));
#18083=CARTESIAN_POINT('Ctrl Pts',(-7.07057502873392,-40.4530191071451,
-4.082198396148));
#18084=CARTESIAN_POINT('Ctrl Pts',(-9.42743337163542,-40.2780191071451,
1.69768315121407E-11));
#18085=CARTESIAN_POINT('Ctrl Pts',(-7.07057502871922,-40.1030191071451,
4.08219839617346));
#18086=CARTESIAN_POINT('Ctrl Pts',(-4.71371668580301,-39.9280191071451,
8.16439679232994));
#18087=CARTESIAN_POINT('Ctrl Pts',(1.47018674401621E-11,-39.7530191071451,
8.16439679232146));
#18088=CARTESIAN_POINT('Ctrl Pts',(4.71371668583241,-39.5780191071451,8.16439679231297));
#18089=CARTESIAN_POINT('Ctrl Pts',(7.07057502873392,-39.4030191071451,4.082198396148));
#18090=CARTESIAN_POINT('Ctrl Pts',(9.42743337163542,-39.2280191071451,-1.69756769845304E-11));
#18091=CARTESIAN_POINT('Ctrl Pts',(7.07057502871922,-39.0530191071451,-4.08219839617346));
#18092=CARTESIAN_POINT('Ctrl Pts',(4.71371668580301,-38.8780191071451,-8.16439679232994));
#18093=CARTESIAN_POINT('Ctrl Pts',(-1.4702867290402E-11,-38.7030191071451,
-8.16439679232146));
#18094=CARTESIAN_POINT('Ctrl Pts',(-4.71371668583241,-38.5280191071451,
-8.16439679231297));
#18095=CARTESIAN_POINT('Ctrl Pts',(-7.07057502873392,-38.3530191071451,
-4.082198396148));
#18096=CARTESIAN_POINT('Ctrl Pts',(-9.42743337163542,-38.1780191071451,
1.69768315121407E-11));
#18097=CARTESIAN_POINT('Ctrl Pts',(-7.07057502871922,-38.0030191071451,
4.08219839617346));
#18098=CARTESIAN_POINT('Ctrl Pts',(-4.71371668580301,-37.8280191071451,
8.16439679232994));
#18099=CARTESIAN_POINT('Ctrl Pts',(1.47018674401621E-11,-37.6530191071451,
8.16439679232146));
#18100=CARTESIAN_POINT('Ctrl Pts',(4.71371668583241,-37.4780191071451,8.16439679231297));
#18101=CARTESIAN_POINT('Ctrl Pts',(7.07057502873392,-37.3030191071451,4.082198396148));
#18102=CARTESIAN_POINT('Ctrl Pts',(9.42743337163542,-37.1280191071451,-1.69756769845304E-11));
#18103=CARTESIAN_POINT('Ctrl Pts',(7.07057502871922,-36.9530191071451,-4.08219839617346));
#18104=CARTESIAN_POINT('Ctrl Pts',(4.71371668580301,-36.7780191071451,-8.16439679232994));
#18105=CARTESIAN_POINT('Ctrl Pts',(-1.4702867290402E-11,-36.6030191071451,
-8.16439679232146));
#18106=CARTESIAN_POINT('Ctrl Pts',(-4.71371668583241,-36.4280191071451,
-8.16439679231297));
#18107=CARTESIAN_POINT('Ctrl Pts',(-7.07057502873392,-36.2530191071451,
-4.082198396148));
#18108=CARTESIAN_POINT('Ctrl Pts',(-9.42743337163542,-36.0780191071451,
1.69768315121407E-11));
#18109=CARTESIAN_POINT('Ctrl Pts',(-7.07057502871922,-35.9030191071451,
4.08219839617346));
#18110=CARTESIAN_POINT('Ctrl Pts',(-4.71371668580301,-35.7280191071451,
8.16439679232994));
#18111=CARTESIAN_POINT('Ctrl Pts',(1.47018674401621E-11,-35.5530191071451,
8.16439679232146));
#18112=CARTESIAN_POINT('Ctrl Pts',(4.71371668583241,-35.3780191071451,8.16439679231297));
#18113=CARTESIAN_POINT('Ctrl Pts',(7.07057502873392,-35.2030191071451,4.082198396148));
#18114=CARTESIAN_POINT('Ctrl Pts',(9.42743337163542,-35.0280191071451,-1.69756769845304E-11));
#18115=CARTESIAN_POINT('Ctrl Pts',(7.07057502871922,-34.8530191071451,-4.08219839617346));
#18116=CARTESIAN_POINT('Ctrl Pts',(4.71371668580301,-34.6780191071451,-8.16439679232994));
#18117=CARTESIAN_POINT('Ctrl Pts',(-1.4702867290402E-11,-34.5030191071451,
-8.16439679232146));
#18118=CARTESIAN_POINT('Ctrl Pts',(-4.71371668583241,-34.3280191071451,
-8.16439679231297));
#18119=CARTESIAN_POINT('Ctrl Pts',(-7.07057502873392,-34.1530191071451,
-4.082198396148));
#18120=CARTESIAN_POINT('Ctrl Pts',(-9.42743337163542,-33.9780191071451,
1.69768315121407E-11));
#18121=CARTESIAN_POINT('Ctrl Pts',(-7.07057502871922,-33.8030191071451,
4.08219839617346));
#18122=CARTESIAN_POINT('Ctrl Pts',(-4.71371668580301,-33.6280191071451,
8.16439679232994));
#18123=CARTESIAN_POINT('Ctrl Pts',(1.47018674401621E-11,-33.4530191071451,
8.16439679232146));
#18124=CARTESIAN_POINT('Ctrl Pts',(4.71371668583241,-33.2780191071451,8.16439679231297));
#18125=CARTESIAN_POINT('Ctrl Pts',(7.07057502873392,-33.1030191071451,4.082198396148));
#18126=CARTESIAN_POINT('Ctrl Pts',(9.42743337163542,-32.9280191071451,-1.69756769845304E-11));
#18127=CARTESIAN_POINT('Ctrl Pts',(7.07057502871922,-32.7530191071451,-4.08219839617346));
#18128=CARTESIAN_POINT('Ctrl Pts',(4.71371668580301,-32.5780191071451,-8.16439679232994));
#18129=CARTESIAN_POINT('Ctrl Pts',(-1.4702867290402E-11,-32.4030191071451,
-8.16439679232146));
#18130=CARTESIAN_POINT('Ctrl Pts',(-4.71371668583241,-32.2280191071451,
-8.16439679231297));
#18131=CARTESIAN_POINT('Ctrl Pts',(-7.07057502873392,-32.0530191071451,
-4.082198396148));
#18132=CARTESIAN_POINT('Ctrl Pts',(-9.42743337163542,-31.8780191071451,
1.69768315121407E-11));
#18133=CARTESIAN_POINT('Ctrl Pts',(-7.07057502871922,-31.7030191071451,
4.08219839617346));
#18134=CARTESIAN_POINT('Ctrl Pts',(-4.71371668580301,-31.5280191071451,
8.16439679232994));
#18135=CARTESIAN_POINT('Ctrl Pts',(1.47018674401621E-11,-31.3530191071451,
8.16439679232146));
#18136=CARTESIAN_POINT('Ctrl Pts',(4.71371668583241,-31.1780191071451,8.16439679231297));
#18137=CARTESIAN_POINT('Ctrl Pts',(7.07057502873392,-31.0030191071451,4.082198396148));
#18138=CARTESIAN_POINT('Ctrl Pts',(9.42743337163542,-30.8280191071451,-1.69756769845304E-11));
#18139=CARTESIAN_POINT('Ctrl Pts',(7.07057502871922,-30.6530191071451,-4.08219839617346));
#18140=CARTESIAN_POINT('Ctrl Pts',(4.71371668580301,-30.4780191071451,-8.16439679232994));
#18141=CARTESIAN_POINT('Ctrl Pts',(-1.4702867290402E-11,-30.3030191071451,
-8.16439679232146));
#18142=CARTESIAN_POINT('Ctrl Pts',(-4.71371668583241,-30.1280191071451,
-8.16439679231297));
#18143=CARTESIAN_POINT('Ctrl Pts',(-7.07057502873392,-29.9530191071451,
-4.082198396148));
#18144=CARTESIAN_POINT('Ctrl Pts',(-9.42743337163542,-29.7780191071451,
1.69768315121407E-11));
#18145=CARTESIAN_POINT('Ctrl Pts',(-7.07057502871922,-29.6030191071451,
4.08219839617346));
#18146=CARTESIAN_POINT('Ctrl Pts',(-4.71371668580301,-29.4280191071451,
8.16439679232994));
#18147=CARTESIAN_POINT('Ctrl Pts',(1.47018674401621E-11,-29.2530191071451,
8.16439679232146));
#18148=CARTESIAN_POINT('Ctrl Pts',(4.71371668583241,-29.0780191071451,8.16439679231297));
#18149=CARTESIAN_POINT('Ctrl Pts',(7.07057502873392,-28.9030191071451,4.082198396148));
#18150=CARTESIAN_POINT('Ctrl Pts',(9.42743337163542,-28.7280191071451,-1.69756769845304E-11));
#18151=CARTESIAN_POINT('Ctrl Pts',(7.07057502871922,-28.5530191071451,-4.08219839617346));
#18152=CARTESIAN_POINT('Ctrl Pts',(4.71371668580301,-28.3780191071451,-8.16439679232994));
#18153=CARTESIAN_POINT('Ctrl Pts',(-1.4702867290402E-11,-28.2030191071451,
-8.16439679232146));
#18154=CARTESIAN_POINT('Ctrl Pts',(-4.71371668583241,-28.0280191071451,
-8.16439679231297));
#18155=CARTESIAN_POINT('Ctrl Pts',(-7.07057502873392,-27.8530191071451,
-4.082198396148));
#18156=CARTESIAN_POINT('Ctrl Pts',(-9.42743337163542,-27.6780191071451,
1.69768315121407E-11));
#18157=CARTESIAN_POINT('Ctrl Pts',(-7.07057502871922,-27.5030191071451,
4.08219839617346));
#18158=CARTESIAN_POINT('Ctrl Pts',(-4.71371668580301,-27.3280191071451,
8.16439679232994));
#18159=CARTESIAN_POINT('Ctrl Pts',(1.47018674401621E-11,-27.1530191071451,
8.16439679232146));
#18160=CARTESIAN_POINT('Ctrl Pts',(4.71371668583241,-26.9780191071451,8.16439679231297));
#18161=CARTESIAN_POINT('Ctrl Pts',(7.07057502873392,-26.8030191071451,4.082198396148));
#18162=CARTESIAN_POINT('Ctrl Pts',(9.42743337163542,-26.6280191071451,-1.69756769845304E-11));
#18163=CARTESIAN_POINT('Ctrl Pts',(7.07057502871922,-26.4530191071451,-4.08219839617346));
#18164=CARTESIAN_POINT('Ctrl Pts',(4.71371668580301,-26.2780191071451,-8.16439679232994));
#18165=CARTESIAN_POINT('Ctrl Pts',(-1.4702867290402E-11,-26.1030191071451,
-8.16439679232146));
#18166=CARTESIAN_POINT('Ctrl Pts',(-4.71371668583241,-25.9280191071451,
-8.16439679231297));
#18167=CARTESIAN_POINT('Ctrl Pts',(-7.07057502873392,-25.7530191071451,
-4.082198396148));
#18168=CARTESIAN_POINT('Ctrl Pts',(-9.42743337163542,-25.5780191071451,
1.69768315121407E-11));
#18169=CARTESIAN_POINT('Ctrl Pts',(-7.07057502871922,-25.4030191071451,
4.08219839617346));
#18170=CARTESIAN_POINT('Ctrl Pts',(-4.71371668580301,-25.2280191071451,
8.16439679232994));
#18171=CARTESIAN_POINT('Ctrl Pts',(1.47018674401621E-11,-25.0530191071451,
8.16439679232146));
#18172=CARTESIAN_POINT('Ctrl Pts',(4.71371668583241,-24.8780191071451,8.16439679231297));
#18173=CARTESIAN_POINT('Ctrl Pts',(7.07057502873392,-24.7030191071451,4.082198396148));
#18174=CARTESIAN_POINT('Ctrl Pts',(9.42743337163542,-24.5280191071451,-1.69756769845304E-11));
#18175=CARTESIAN_POINT('Ctrl Pts',(7.07057502871922,-24.3530191071451,-4.08219839617346));
#18176=CARTESIAN_POINT('Ctrl Pts',(4.71371668580301,-24.1780191071451,-8.16439679232994));
#18177=CARTESIAN_POINT('Ctrl Pts',(-1.4702867290402E-11,-24.0030191071451,
-8.16439679232146));
#18178=CARTESIAN_POINT('Ctrl Pts',(-4.71371668583241,-23.8280191071451,
-8.16439679231297));
#18179=CARTESIAN_POINT('Ctrl Pts',(-7.07057502873392,-23.6530191071451,
-4.082198396148));
#18180=CARTESIAN_POINT('Ctrl Pts',(-9.42743337163542,-23.4780191071451,
1.69768315121407E-11));
#18181=CARTESIAN_POINT('Ctrl Pts',(-7.07057502871922,-23.3030191071451,
4.08219839617346));
#18182=CARTESIAN_POINT('Ctrl Pts',(-4.71371668580301,-23.1280191071451,
8.16439679232994));
#18183=CARTESIAN_POINT('Ctrl Pts',(1.47018674401621E-11,-22.9530191071451,
8.16439679232146));
#18184=CARTESIAN_POINT('Ctrl Pts',(4.71371668583241,-22.7780191071451,8.16439679231297));
#18185=CARTESIAN_POINT('Ctrl Pts',(7.07057502873392,-22.6030191071451,4.082198396148));
#18186=CARTESIAN_POINT('Ctrl Pts',(9.42743337163542,-22.4280191071451,-1.69756769845304E-11));
#18187=CARTESIAN_POINT('Ctrl Pts',(7.07057502871922,-22.2530191071451,-4.08219839617346));
#18188=CARTESIAN_POINT('Ctrl Pts',(4.71371668580301,-22.0780191071451,-8.16439679232994));
#18189=CARTESIAN_POINT('Ctrl Pts',(-1.4702867290402E-11,-21.9030191071451,
-8.16439679232146));
#18190=CARTESIAN_POINT('Ctrl Pts',(-4.71371668583241,-21.7280191071451,
-8.16439679231297));
#18191=CARTESIAN_POINT('Ctrl Pts',(-7.07057502873392,-21.5530191071451,
-4.082198396148));
#18192=CARTESIAN_POINT('Ctrl Pts',(-9.42743337163542,-21.3780191071451,
1.69768315121407E-11));
#18193=CARTESIAN_POINT('Ctrl Pts',(-7.07057502871922,-21.2030191071451,
4.08219839617346));
#18194=CARTESIAN_POINT('Ctrl Pts',(-4.71371668580301,-21.0280191071451,
8.16439679232994));
#18195=CARTESIAN_POINT('Ctrl Pts',(1.47018674401621E-11,-20.8530191071451,
8.16439679232146));
#18196=CARTESIAN_POINT('Ctrl Pts',(4.71371668583241,-20.6780191071451,8.16439679231297));
#18197=CARTESIAN_POINT('Ctrl Pts',(7.07057502873392,-20.5030191071451,4.082198396148));
#18198=CARTESIAN_POINT('Ctrl Pts',(9.42743337163542,-20.3280191071451,-1.69756769845304E-11));
#18199=CARTESIAN_POINT('Ctrl Pts',(7.07057502871922,-20.1530191071451,-4.08219839617346));
#18200=CARTESIAN_POINT('Ctrl Pts',(4.71371668580301,-19.9780191071451,-8.16439679232994));
#18201=CARTESIAN_POINT('Ctrl Pts',(-1.4702867290402E-11,-19.8030191071451,
-8.16439679232146));
#18202=CARTESIAN_POINT('Ctrl Pts',(-4.71371668583241,-19.6280191071451,
-8.16439679231297));
#18203=CARTESIAN_POINT('Ctrl Pts',(-7.07057502873392,-19.4530191071451,
-4.082198396148));
#18204=CARTESIAN_POINT('Ctrl Pts',(-9.42743337163542,-19.2780191071451,
1.69768315121407E-11));
#18205=CARTESIAN_POINT('Ctrl Pts',(-7.07057502871922,-19.1030191071451,
4.08219839617346));
#18206=CARTESIAN_POINT('Ctrl Pts',(-4.71371668580301,-18.9280191071451,
8.16439679232994));
#18207=CARTESIAN_POINT('Ctrl Pts',(1.47018674401621E-11,-18.7530191071451,
8.16439679232146));
#18208=CARTESIAN_POINT('Ctrl Pts',(4.71371668583241,-18.5780191071451,8.16439679231297));
#18209=CARTESIAN_POINT('Ctrl Pts',(7.07057502873392,-18.4030191071451,4.082198396148));
#18210=CARTESIAN_POINT('Ctrl Pts',(9.42743337163542,-18.2280191071451,-1.69756769845304E-11));
#18211=CARTESIAN_POINT('Ctrl Pts',(7.07057502871922,-18.0530191071451,-4.08219839617346));
#18212=CARTESIAN_POINT('Ctrl Pts',(4.71371668580301,-17.8780191071451,-8.16439679232994));
#18213=CARTESIAN_POINT('Ctrl Pts',(-1.4702867290402E-11,-17.7030191071451,
-8.16439679232146));
#18214=CARTESIAN_POINT('Ctrl Pts',(-4.71371668583241,-17.5280191071451,
-8.16439679231297));
#18215=CARTESIAN_POINT('Ctrl Pts',(-7.07057502873392,-17.3530191071451,
-4.082198396148));
#18216=CARTESIAN_POINT('Ctrl Pts',(-9.42743337163542,-17.1780191071451,
1.69768315121407E-11));
#18217=CARTESIAN_POINT('Ctrl Pts',(-7.07057502871922,-17.0030191071451,
4.08219839617346));
#18218=CARTESIAN_POINT('Ctrl Pts',(-4.71371668580301,-16.8280191071451,
8.16439679232994));
#18219=CARTESIAN_POINT('Ctrl Pts',(1.47018674401621E-11,-16.6530191071451,
8.16439679232146));
#18220=CARTESIAN_POINT('Ctrl Pts',(4.71371668583241,-16.4780191071451,8.16439679231297));
#18221=CARTESIAN_POINT('Ctrl Pts',(7.07057502873392,-16.3030191071451,4.082198396148));
#18222=CARTESIAN_POINT('Ctrl Pts',(9.42743337163542,-16.1280191071451,-1.69756769845304E-11));
#18223=CARTESIAN_POINT('Ctrl Pts',(7.07057502871922,-15.9530191071451,-4.08219839617346));
#18224=CARTESIAN_POINT('Ctrl Pts',(4.71371668580301,-15.7780191071451,-8.16439679232994));
#18225=CARTESIAN_POINT('Ctrl Pts',(-1.4702867290402E-11,-15.6030191071451,
-8.16439679232146));
#18226=CARTESIAN_POINT('Ctrl Pts',(-4.71371668583241,-15.4280191071451,
-8.16439679231297));
#18227=CARTESIAN_POINT('Ctrl Pts',(-7.07057502873392,-15.2530191071451,
-4.082198396148));
#18228=CARTESIAN_POINT('Ctrl Pts',(-9.42743337163542,-15.0780191071451,
1.69768315121407E-11));
#18229=CARTESIAN_POINT('Ctrl Pts',(-7.07057502871922,-14.9030191071451,
4.08219839617346));
#18230=CARTESIAN_POINT('Ctrl Pts',(-4.71371668580301,-14.7280191071451,
8.16439679232994));
#18231=CARTESIAN_POINT('Ctrl Pts',(1.47018674401621E-11,-14.5530191071451,
8.16439679232146));
#18232=CARTESIAN_POINT('Ctrl Pts',(4.71371668583241,-14.3780191071451,8.16439679231297));
#18233=CARTESIAN_POINT('Ctrl Pts',(7.07057502873392,-14.2030191071451,4.082198396148));
#18234=CARTESIAN_POINT('Ctrl Pts',(9.42743337163542,-14.0280191071451,-1.69756769845304E-11));
#18235=CARTESIAN_POINT('Ctrl Pts',(7.07057502871922,-13.8530191071451,-4.08219839617346));
#18236=CARTESIAN_POINT('Ctrl Pts',(4.71371668580301,-13.6780191071451,-8.16439679232994));
#18237=CARTESIAN_POINT('Ctrl Pts',(-1.4702867290402E-11,-13.5030191071451,
-8.16439679232146));
#18238=CARTESIAN_POINT('Ctrl Pts',(-4.71371668583241,-13.3280191071452,
-8.16439679231297));
#18239=CARTESIAN_POINT('Ctrl Pts',(-7.07057502873392,-13.1530191071451,
-4.082198396148));
#18240=CARTESIAN_POINT('Ctrl Pts',(-9.42743337163542,-12.9780191071451,
1.69768315121407E-11));
#18241=CARTESIAN_POINT('Ctrl Pts',(-7.07057502871922,-12.8030191071452,
4.08219839617346));
#18242=CARTESIAN_POINT('Ctrl Pts',(-4.71371668580301,-12.6280191071451,
8.16439679232994));
#18243=CARTESIAN_POINT('Ctrl Pts',(1.47018674401621E-11,-12.4530191071451,
8.16439679232146));
#18244=CARTESIAN_POINT('Ctrl Pts',(4.71371668583241,-12.2780191071452,8.16439679231297));
#18245=CARTESIAN_POINT('Ctrl Pts',(7.07057502873392,-12.1030191071451,4.082198396148));
#18246=CARTESIAN_POINT('Ctrl Pts',(9.42743337163542,-11.9280191071451,-1.69756769845304E-11));
#18247=CARTESIAN_POINT('Ctrl Pts',(7.07057502871922,-11.7530191071452,-4.08219839617346));
#18248=CARTESIAN_POINT('Ctrl Pts',(4.71371668580301,-11.5780191071452,-8.16439679232994));
#18249=CARTESIAN_POINT('Ctrl Pts',(-1.4702867290402E-11,-11.4030191071451,
-8.16439679232146));
#18250=CARTESIAN_POINT('Ctrl Pts',(-4.71371668583241,-11.2280191071451,
-8.16439679231297));
#18251=CARTESIAN_POINT('Ctrl Pts',(-7.07057502873392,-11.0530191071452,
-4.082198396148));
#18252=CARTESIAN_POINT('Ctrl Pts',(-9.42743337163542,-10.8780191071451,
1.69768315121407E-11));
#18253=CARTESIAN_POINT('Ctrl Pts',(-7.07057502871922,-10.7030191071451,
4.08219839617346));
#18254=CARTESIAN_POINT('Ctrl Pts',(-4.71371668580301,-10.5280191071452,
8.16439679232994));
#18255=CARTESIAN_POINT('Ctrl Pts',(1.47018674401621E-11,-10.3530191071451,
8.16439679232146));
#18256=CARTESIAN_POINT('Ctrl Pts',(4.71371668583241,-10.1780191071451,8.16439679231297));
#18257=CARTESIAN_POINT('Ctrl Pts',(7.07057502873392,-10.0030191071452,4.082198396148));
#18258=CARTESIAN_POINT('Ctrl Pts',(9.42743337163542,-9.82801910714514,-1.69756769845304E-11));
#18259=CARTESIAN_POINT('Ctrl Pts',(7.07057502871922,-9.65301910714514,-4.08219839617346));
#18260=CARTESIAN_POINT('Ctrl Pts',(4.71371668580301,-9.47801910714516,-8.16439679232994));
#18261=CARTESIAN_POINT('Ctrl Pts',(-1.4702867290402E-11,-9.30301910714514,
-8.16439679232146));
#18262=CARTESIAN_POINT('Ctrl Pts',(-4.71371668583241,-9.12801910714515,
-8.16439679231297));
#18263=CARTESIAN_POINT('Ctrl Pts',(-7.07057502873392,-8.95301910714516,
-4.082198396148));
#18264=CARTESIAN_POINT('Ctrl Pts',(-9.42743337163542,-8.77801910714516,
1.69768315121407E-11));
#18265=CARTESIAN_POINT('Ctrl Pts',(-7.07057502871922,-8.60301910714514,
4.08219839617346));
#18266=CARTESIAN_POINT('Ctrl Pts',(-4.71371668580301,-8.42801910714516,
8.16439679232994));
#18267=CARTESIAN_POINT('Ctrl Pts',(1.47018674401621E-11,-8.25301910714516,
8.16439679232146));
#18268=CARTESIAN_POINT('Ctrl Pts',(4.71371668583241,-8.07801910714515,8.16439679231297));
#18269=CARTESIAN_POINT('Ctrl Pts',(7.07057502873392,-7.90301910714516,4.082198396148));
#18270=CARTESIAN_POINT('Ctrl Pts',(9.42743337163542,-7.72801910714516,-1.69756769845304E-11));
#18271=CARTESIAN_POINT('Ctrl Pts',(7.07057502871922,-7.55301910714514,-4.08219839617346));
#18272=CARTESIAN_POINT('Ctrl Pts',(4.71371668580301,-7.37801910714516,-8.16439679232994));
#18273=CARTESIAN_POINT('Ctrl Pts',(-1.4702867290402E-11,-7.20301910714516,
-8.16439679232146));
#18274=CARTESIAN_POINT('Ctrl Pts',(-4.71371668583241,-7.02801910714516,
-8.16439679231297));
#18275=CARTESIAN_POINT('Ctrl Pts',(-7.07057502873392,-6.85301910714514,
-4.082198396148));
#18276=CARTESIAN_POINT('Ctrl Pts',(-9.42743337163542,-6.67801910714516,
1.69768315121407E-11));
#18277=CARTESIAN_POINT('Ctrl Pts',(-7.07057502871922,-6.50301910714514,
4.08219839617346));
#18278=CARTESIAN_POINT('Ctrl Pts',(-4.71371668580301,-6.32801910714515,
8.16439679232994));
#18279=CARTESIAN_POINT('Ctrl Pts',(1.47018674401621E-11,-6.15301910714516,
8.16439679232146));
#18280=CARTESIAN_POINT('Ctrl Pts',(4.71371668583241,-5.97801910714516,8.16439679231297));
#18281=CARTESIAN_POINT('Ctrl Pts',(7.07057502873392,-5.80301910714515,4.082198396148));
#18282=CARTESIAN_POINT('Ctrl Pts',(9.42743337163542,-5.62801910714516,-1.69756769845304E-11));
#18283=CARTESIAN_POINT('Ctrl Pts',(7.07057502871922,-5.45301910714515,-4.08219839617346));
#18284=CARTESIAN_POINT('Ctrl Pts',(4.71371668580301,-5.27801910714516,-8.16439679232994));
#18285=CARTESIAN_POINT('Ctrl Pts',(-1.4702867290402E-11,-5.10301910714516,
-8.16439679232146));
#18286=CARTESIAN_POINT('Ctrl Pts',(-4.71371668583241,-4.92801910714516,
-8.16439679231297));
#18287=CARTESIAN_POINT('Ctrl Pts',(-7.07057502873392,-4.75301910714515,
-4.082198396148));
#18288=CARTESIAN_POINT('Ctrl Pts',(-9.42743337163542,-4.57801910714517,
1.69768315121407E-11));
#18289=CARTESIAN_POINT('Ctrl Pts',(-7.07057502871922,-4.40301910714516,
4.08219839617346));
#18290=CARTESIAN_POINT('Ctrl Pts',(-4.71371668580301,-4.22801910714516,
8.16439679232994));
#18291=CARTESIAN_POINT('Ctrl Pts',(1.47018674401621E-11,-4.05301910714517,
8.16439679232146));
#18292=CARTESIAN_POINT('Ctrl Pts',(4.71371668583241,-3.87801910714518,8.16439679231297));
#18293=CARTESIAN_POINT('Ctrl Pts',(7.07057502873392,-3.70301910714515,4.082198396148));
#18294=CARTESIAN_POINT('Ctrl Pts',(9.42743337163542,-3.52801910714518,-1.69756769845304E-11));
#18295=CARTESIAN_POINT('Ctrl Pts',(7.07057502871922,-3.35301910714517,-4.08219839617346));
#18296=CARTESIAN_POINT('Ctrl Pts',(4.71371668580301,-3.17801910714516,-8.16439679232994));
#18297=CARTESIAN_POINT('Ctrl Pts',(-1.4702867290402E-11,-3.00301910714517,
-8.16439679232146));
#18298=CARTESIAN_POINT('Ctrl Pts',(-4.71371668583241,-2.82801910714518,
-8.16439679231297));
#18299=CARTESIAN_POINT('Ctrl Pts',(-7.07057502873392,-2.65301910714515,
-4.082198396148));
#18300=CARTESIAN_POINT('Ctrl Pts',(-9.42743337163542,-2.47801910714516,
1.69768315121407E-11));
#18301=CARTESIAN_POINT('Ctrl Pts',(-7.07057502871922,-2.30301910714517,
4.08219839617346));
#18302=CARTESIAN_POINT('Ctrl Pts',(-4.71371668580301,-2.12801910714516,
8.16439679232994));
#18303=CARTESIAN_POINT('Ctrl Pts',(1.47018674401621E-11,-1.95301910714515,
8.16439679232146));
#18304=CARTESIAN_POINT('Ctrl Pts',(4.71371668583241,-1.77801910714518,8.16439679231297));
#18305=CARTESIAN_POINT('Ctrl Pts',(7.07057502873392,-1.60301910714516,4.082198396148));
#18306=CARTESIAN_POINT('Ctrl Pts',(9.42743337163542,-1.42801910714516,-1.69756769845304E-11));
#18307=CARTESIAN_POINT('Ctrl Pts',(7.07057502871922,-1.25301910714517,-4.08219839617346));
#18308=CARTESIAN_POINT('Ctrl Pts',(4.71371668580301,-1.07801910714517,-8.16439679232994));
#18309=CARTESIAN_POINT('Ctrl Pts',(-1.4702867290402E-11,-0.903019107145155,
-8.16439679232146));
#18310=CARTESIAN_POINT('Ctrl Pts',(-4.71371668583241,-0.728019107145183,
-8.16439679231297));
#18311=CARTESIAN_POINT('Ctrl Pts',(-7.07057502873392,-0.553019107145171,
-4.082198396148));
#18312=CARTESIAN_POINT('Ctrl Pts',(-9.42743337163542,-0.378019107145163,
1.69768315121407E-11));
#18313=CARTESIAN_POINT('Ctrl Pts',(-7.07057502871922,-0.203019107145175,
4.08219839617346));
#18314=CARTESIAN_POINT('Ctrl Pts',(-4.71371668580301,-0.0280191071451809,
8.16439679232994));
#18315=CARTESIAN_POINT('Ctrl Pts',(1.47018674401621E-11,0.146980892854842,
8.16439679232146));
#18316=CARTESIAN_POINT('Ctrl Pts',(4.71371668583241,0.321980892854814,8.16439679231297));
#18317=CARTESIAN_POINT('Ctrl Pts',(7.07057502873392,0.496980892854826,4.082198396148));
#18318=CARTESIAN_POINT('Ctrl Pts',(9.42743337163542,0.671980892854834,-1.69756769845304E-11));
#18319=CARTESIAN_POINT('Ctrl Pts',(7.07057502871922,0.846980892854822,-4.08219839617346));
#18320=CARTESIAN_POINT('Ctrl Pts',(4.71371668580301,1.02198089285482,-8.16439679232994));
#18321=CARTESIAN_POINT('Ctrl Pts',(-1.4702867290402E-11,1.19698089285484,
-8.16439679232146));
#18322=CARTESIAN_POINT('Ctrl Pts',(-4.71371668583241,1.37198089285481,-8.16439679231297));
#18323=CARTESIAN_POINT('Ctrl Pts',(-7.07057502873392,1.54698089285482,-4.082198396148));
#18324=CARTESIAN_POINT('Ctrl Pts',(-9.42743337163542,1.72198089285483,1.69768315121407E-11));
#18325=CARTESIAN_POINT('Ctrl Pts',(-7.07057502871922,1.89698089285484,4.08219839617346));
#18326=CARTESIAN_POINT('Ctrl Pts',(-4.71371668580301,2.07198089285481,8.16439679232994));
#18327=CARTESIAN_POINT('Ctrl Pts',(1.47018674401621E-11,2.24698089285484,
8.16439679232146));
#18328=CARTESIAN_POINT('Ctrl Pts',(4.71371668583241,2.42198089285483,8.16439679231297));
#18329=CARTESIAN_POINT('Ctrl Pts',(7.07057502873392,2.59698089285482,4.082198396148));
#18330=CARTESIAN_POINT('Ctrl Pts',(9.42743337163542,2.77198089285483,-1.69756769845304E-11));
#18331=CARTESIAN_POINT('Ctrl Pts',(7.07057502871922,2.94698089285484,-4.08219839617346));
#18332=CARTESIAN_POINT('Ctrl Pts',(4.71371668580301,3.12198089285481,-8.16439679232994));
#18333=CARTESIAN_POINT('Ctrl Pts',(-1.4702867290402E-11,3.29698089285482,
-8.16439679232146));
#18334=CARTESIAN_POINT('Ctrl Pts',(-4.71371668583241,3.47198089285483,-8.16439679231297));
#18335=CARTESIAN_POINT('Ctrl Pts',(-7.07057502873392,3.64698089285482,-4.082198396148));
#18336=CARTESIAN_POINT('Ctrl Pts',(-9.42743337163542,3.82198089285481,1.69768315121407E-11));
#18337=CARTESIAN_POINT('Ctrl Pts',(-7.07057502871922,3.99698089285483,4.08219839617346));
#18338=CARTESIAN_POINT('Ctrl Pts',(-4.71371668580301,4.17198089285481,8.16439679232994));
#18339=CARTESIAN_POINT('Ctrl Pts',(1.47018674401621E-11,4.34698089285482,
8.16439679232146));
#18340=CARTESIAN_POINT('Ctrl Pts',(4.71371668583241,4.52198089285483,8.16439679231297));
#18341=CARTESIAN_POINT('Ctrl Pts',(7.07057502873392,4.69698089285481,4.082198396148));
#18342=CARTESIAN_POINT('Ctrl Pts',(9.42743337163542,4.87198089285481,-1.69756769845304E-11));
#18343=CARTESIAN_POINT('Ctrl Pts',(7.07057502871922,5.04698089285483,-4.08219839617346));
#18344=CARTESIAN_POINT('Ctrl Pts',(4.71371668580301,5.22198089285481,-8.16439679232994));
#18345=CARTESIAN_POINT('Ctrl Pts',(-1.4702867290402E-11,5.39698089285482,
-8.16439679232146));
#18346=CARTESIAN_POINT('Ctrl Pts',(-4.71371668583241,5.57198089285483,-8.16439679231297));
#18347=CARTESIAN_POINT('Ctrl Pts',(-7.07057502873392,5.74698089285481,-4.082198396148));
#18348=CARTESIAN_POINT('Ctrl Pts',(-9.42743337163542,5.92198089285481,1.69768315121407E-11));
#18349=CARTESIAN_POINT('Ctrl Pts',(-7.07057502871922,6.09698089285483,4.08219839617346));
#18350=CARTESIAN_POINT('Ctrl Pts',(-4.71371668580301,6.2719808928548,8.16439679232994));
#18351=CARTESIAN_POINT('Ctrl Pts',(1.47018674401621E-11,6.44698089285481,
8.16439679232146));
#18352=CARTESIAN_POINT('Ctrl Pts',(4.71371668583241,6.62198089285482,8.16439679231297));
#18353=CARTESIAN_POINT('Ctrl Pts',(7.07057502873392,6.79698089285483,4.082198396148));
#18354=CARTESIAN_POINT('Ctrl Pts',(9.42743337163542,6.97198089285481,-1.69756769845304E-11));
#18355=CARTESIAN_POINT('Ctrl Pts',(7.07057502871922,7.14698089285482,-4.08219839617346));
#18356=CARTESIAN_POINT('Ctrl Pts',(4.71371668580301,7.32198089285482,-8.16439679232994));
#18357=CARTESIAN_POINT('Ctrl Pts',(-1.4702867290402E-11,7.49698089285481,
-8.16439679232146));
#18358=CARTESIAN_POINT('Ctrl Pts',(-4.71371668583241,7.67198089285481,-8.16439679231297));
#18359=CARTESIAN_POINT('Ctrl Pts',(-7.07057502873392,7.84698089285483,-4.082198396148));
#18360=CARTESIAN_POINT('Ctrl Pts',(-9.42743337163542,8.0219808928548,1.69768315121407E-11));
#18361=CARTESIAN_POINT('Ctrl Pts',(-7.07057502871922,8.19698089285481,4.08219839617346));
#18362=CARTESIAN_POINT('Ctrl Pts',(-4.71371668580301,8.37198089285483,8.16439679232994));
#18363=CARTESIAN_POINT('Ctrl Pts',(1.47018674401621E-11,8.54698089285481,
8.16439679232146));
#18364=CARTESIAN_POINT('Ctrl Pts',(4.71371668583241,8.72198089285481,8.16439679231297));
#18365=CARTESIAN_POINT('Ctrl Pts',(7.07057502873392,8.89698089285482,4.082198396148));
#18366=CARTESIAN_POINT('Ctrl Pts',(9.42743337163542,9.0719808928548,-1.69756769845304E-11));
#18367=CARTESIAN_POINT('Ctrl Pts',(7.07057502871922,9.24698089285481,-4.08219839617346));
#18368=CARTESIAN_POINT('Ctrl Pts',(4.71371668580301,9.42198089285482,-8.16439679232994));
#18369=CARTESIAN_POINT('Ctrl Pts',(-1.4702867290402E-11,9.5969808928548,
-8.16439679232146));
#18370=CARTESIAN_POINT('Ctrl Pts',(-4.71371668583241,9.7719808928548,-8.16439679231297));
#18371=CARTESIAN_POINT('Ctrl Pts',(-7.07057502873392,9.94698089285482,-4.082198396148));
#18372=CARTESIAN_POINT('Ctrl Pts',(-9.42743337163542,10.1219808928548,1.69768315121407E-11));
#18373=CARTESIAN_POINT('Ctrl Pts',(-7.07057502871922,10.2969808928548,4.08219839617346));
#18374=CARTESIAN_POINT('Ctrl Pts',(-4.71371668580301,10.4719808928548,8.16439679232994));
#18375=CARTESIAN_POINT('Ctrl Pts',(1.47018674401621E-11,10.6469808928548,
8.16439679232146));
#18376=CARTESIAN_POINT('Ctrl Pts',(4.71371668583241,10.8219808928548,8.16439679231297));
#18377=CARTESIAN_POINT('Ctrl Pts',(7.07057502873392,10.9969808928548,4.082198396148));
#18378=CARTESIAN_POINT('Ctrl Pts',(9.42743337163542,11.1719808928548,-1.69756769845304E-11));
#18379=CARTESIAN_POINT('Ctrl Pts',(7.07057502871922,11.3469808928548,-4.08219839617346));
#18380=CARTESIAN_POINT('Ctrl Pts',(4.71371668580301,11.5219808928548,-8.16439679232994));
#18381=CARTESIAN_POINT('Ctrl Pts',(-1.4702867290402E-11,11.6969808928548,
-8.16439679232146));
#18382=CARTESIAN_POINT('Ctrl Pts',(-4.71371668583241,11.8719808928548,-8.16439679231297));
#18383=CARTESIAN_POINT('Ctrl Pts',(-7.07057502873392,12.0469808928548,-4.082198396148));
#18384=CARTESIAN_POINT('Ctrl Pts',(-9.42743337163542,12.2219808928548,1.69768315121407E-11));
#18385=CARTESIAN_POINT('Ctrl Pts',(-7.07057502871922,12.3969808928548,4.08219839617346));
#18386=CARTESIAN_POINT('Ctrl Pts',(-4.71371668580301,12.5719808928548,8.16439679232994));
#18387=CARTESIAN_POINT('Ctrl Pts',(1.47018674401621E-11,12.7469808928548,
8.16439679232146));
#18388=CARTESIAN_POINT('Ctrl Pts',(4.71371668583241,12.9219808928548,8.16439679231297));
#18389=CARTESIAN_POINT('Ctrl Pts',(7.07057502873392,13.0969808928548,4.082198396148));
#18390=CARTESIAN_POINT('Ctrl Pts',(9.42743337163542,13.2719808928548,-1.69756769845304E-11));
#18391=CARTESIAN_POINT('Ctrl Pts',(7.07057502871922,13.4469808928548,-4.08219839617346));
#18392=CARTESIAN_POINT('Ctrl Pts',(4.71371668580301,13.6219808928548,-8.16439679232994));
#18393=CARTESIAN_POINT('Ctrl Pts',(-1.4702867290402E-11,13.7969808928548,
-8.16439679232146));
#18394=CARTESIAN_POINT('Ctrl Pts',(-4.71371668583241,13.9719808928548,-8.16439679231297));
#18395=CARTESIAN_POINT('Ctrl Pts',(-7.07057502873392,14.1469808928548,-4.082198396148));
#18396=CARTESIAN_POINT('Ctrl Pts',(-9.42743337163542,14.3219808928548,1.69768315121407E-11));
#18397=CARTESIAN_POINT('Ctrl Pts',(-7.07057502871922,14.4969808928548,4.08219839617346));
#18398=CARTESIAN_POINT('Ctrl Pts',(-4.71371668580301,14.6719808928548,8.16439679232994));
#18399=CARTESIAN_POINT('Ctrl Pts',(1.47018674401621E-11,14.8469808928548,
8.16439679232146));
#18400=CARTESIAN_POINT('Ctrl Pts',(4.71371668583241,15.0219808928548,8.16439679231297));
#18401=CARTESIAN_POINT('Ctrl Pts',(7.07057502873392,15.1969808928548,4.082198396148));
#18402=CARTESIAN_POINT('Ctrl Pts',(9.42743337163542,15.3719808928548,-1.69756769845304E-11));
#18403=CARTESIAN_POINT('Ctrl Pts',(7.07057502871922,15.5469808928548,-4.08219839617346));
#18404=CARTESIAN_POINT('Ctrl Pts',(4.71371668580301,15.7219808928548,-8.16439679232994));
#18405=CARTESIAN_POINT('Ctrl Pts',(-1.4702867290402E-11,15.8969808928548,
-8.16439679232146));
#18406=CARTESIAN_POINT('Ctrl Pts',(-4.71371668583241,16.0719808928548,-8.16439679231297));
#18407=CARTESIAN_POINT('Ctrl Pts',(-7.07057502873392,16.2469808928548,-4.082198396148));
#18408=CARTESIAN_POINT('Ctrl Pts',(-9.42743337163542,16.4219808928548,1.69768315121407E-11));
#18409=CARTESIAN_POINT('Ctrl Pts',(-7.07057502871922,16.5969808928548,4.08219839617346));
#18410=CARTESIAN_POINT('Ctrl Pts',(-4.71371668580301,16.7719808928548,8.16439679232994));
#18411=CARTESIAN_POINT('Ctrl Pts',(1.47018674401621E-11,16.9469808928548,
8.16439679232146));
#18412=CARTESIAN_POINT('Ctrl Pts',(4.71371668583241,17.1219808928548,8.16439679231297));
#18413=CARTESIAN_POINT('Ctrl Pts',(7.07057502873392,17.2969808928548,4.082198396148));
#18414=CARTESIAN_POINT('Ctrl Pts',(9.42743337163542,17.4719808928548,-1.69756769845304E-11));
#18415=CARTESIAN_POINT('Ctrl Pts',(7.07057502871922,17.6469808928548,-4.08219839617346));
#18416=CARTESIAN_POINT('Ctrl Pts',(4.71371668580301,17.8219808928548,-8.16439679232994));
#18417=CARTESIAN_POINT('Ctrl Pts',(-1.4702867290402E-11,17.9969808928548,
-8.16439679232146));
#18418=CARTESIAN_POINT('Ctrl Pts',(-4.71371668583241,18.1719808928548,-8.16439679231297));
#18419=CARTESIAN_POINT('Ctrl Pts',(-7.07057502873392,18.3469808928548,-4.082198396148));
#18420=CARTESIAN_POINT('Ctrl Pts',(-9.42743337163542,18.5219808928548,1.69768315121407E-11));
#18421=CARTESIAN_POINT('Ctrl Pts',(-7.07057502871922,18.6969808928548,4.08219839617346));
#18422=CARTESIAN_POINT('Ctrl Pts',(-4.71371668580301,18.8719808928548,8.16439679232994));
#18423=CARTESIAN_POINT('Ctrl Pts',(1.47018674401621E-11,19.0469808928548,
8.16439679232146));
#18424=CARTESIAN_POINT('Ctrl Pts',(4.71371668583241,19.2219808928548,8.16439679231297));
#18425=CARTESIAN_POINT('Ctrl Pts',(7.07057502873392,19.3969808928548,4.082198396148));
#18426=CARTESIAN_POINT('Ctrl Pts',(9.42743337163542,19.5719808928548,-1.69756769845304E-11));
#18427=CARTESIAN_POINT('Ctrl Pts',(7.07057502871922,19.7469808928548,-4.08219839617346));
#18428=CARTESIAN_POINT('Ctrl Pts',(4.71371668580301,19.9219808928548,-8.16439679232994));
#18429=CARTESIAN_POINT('Ctrl Pts',(-1.4702867290402E-11,20.0969808928548,
-8.16439679232146));
#18430=CARTESIAN_POINT('Ctrl Pts',(-4.71371668583241,20.2719808928548,-8.16439679231297));
#18431=CARTESIAN_POINT('Ctrl Pts',(-7.07057502873392,20.4469808928548,-4.082198396148));
#18432=CARTESIAN_POINT('Ctrl Pts',(-9.42743337163542,20.6219808928548,1.69768315121407E-11));
#18433=CARTESIAN_POINT('Ctrl Pts',(-7.07057502871922,20.7969808928548,4.08219839617346));
#18434=CARTESIAN_POINT('Ctrl Pts',(-4.71371668580301,20.9719808928548,8.16439679232994));
#18435=CARTESIAN_POINT('Ctrl Pts',(1.47018674401621E-11,21.1469808928548,
8.16439679232146));
#18436=CARTESIAN_POINT('Ctrl Pts',(4.71371668583241,21.3219808928548,8.16439679231297));
#18437=CARTESIAN_POINT('Ctrl Pts',(7.07057502873392,21.4969808928548,4.082198396148));
#18438=CARTESIAN_POINT('Ctrl Pts',(9.42743337163542,21.6719808928548,-1.69756769845304E-11));
#18439=CARTESIAN_POINT('Ctrl Pts',(7.07057502871922,21.8469808928548,-4.08219839617346));
#18440=CARTESIAN_POINT('Ctrl Pts',(4.71371668580301,22.0219808928548,-8.16439679232994));
#18441=CARTESIAN_POINT('Ctrl Pts',(-1.4702867290402E-11,22.1969808928548,
-8.16439679232146));
#18442=CARTESIAN_POINT('Ctrl Pts',(-4.71371668583241,22.3719808928548,-8.16439679231297));
#18443=CARTESIAN_POINT('Ctrl Pts',(-7.07057502873392,22.5469808928548,-4.082198396148));
#18444=CARTESIAN_POINT('Ctrl Pts',(-9.42743337163542,22.7219808928548,1.69768315121407E-11));
#18445=CARTESIAN_POINT('Ctrl Pts',(-7.07057502871922,22.8969808928548,4.08219839617346));
#18446=CARTESIAN_POINT('Ctrl Pts',(-4.71371668580301,23.0719808928548,8.16439679232994));
#18447=CARTESIAN_POINT('Ctrl Pts',(1.47018674401621E-11,23.2469808928548,
8.16439679232146));
#18448=CARTESIAN_POINT('Ctrl Pts',(4.71371668583241,23.4219808928548,8.16439679231297));
#18449=CARTESIAN_POINT('Ctrl Pts',(7.07057502873392,23.5969808928548,4.082198396148));
#18450=CARTESIAN_POINT('Ctrl Pts',(9.42743337163542,23.7719808928548,-1.69756769845304E-11));
#18451=CARTESIAN_POINT('Ctrl Pts',(7.07057502871922,23.9469808928548,-4.08219839617346));
#18452=CARTESIAN_POINT('Ctrl Pts',(4.71371668580301,24.1219808928548,-8.16439679232994));
#18453=CARTESIAN_POINT('Ctrl Pts',(-1.4702867290402E-11,24.2969808928548,
-8.16439679232146));
#18454=CARTESIAN_POINT('Ctrl Pts',(-4.71371668583241,24.4719808928548,-8.16439679231297));
#18455=CARTESIAN_POINT('Ctrl Pts',(-7.07057502873392,24.6469808928548,-4.082198396148));
#18456=CARTESIAN_POINT('Ctrl Pts',(-9.42743337163542,24.8219808928548,1.69768315121407E-11));
#18457=CARTESIAN_POINT('Ctrl Pts',(-7.07057502871922,24.9969808928548,4.08219839617346));
#18458=CARTESIAN_POINT('Ctrl Pts',(-4.71371668580301,25.1719808928548,8.16439679232994));
#18459=CARTESIAN_POINT('Ctrl Pts',(1.47018674401621E-11,25.3469808928548,
8.16439679232146));
#18460=CARTESIAN_POINT('Ctrl Pts',(4.71371668583241,25.5219808928548,8.16439679231297));
#18461=CARTESIAN_POINT('Ctrl Pts',(7.07057502873392,25.6969808928548,4.082198396148));
#18462=CARTESIAN_POINT('Ctrl Pts',(9.42743337163542,25.8719808928548,-1.69756769845304E-11));
#18463=CARTESIAN_POINT('Ctrl Pts',(7.07057502871922,26.0469808928548,-4.08219839617346));
#18464=CARTESIAN_POINT('Ctrl Pts',(4.71371668580301,26.2219808928548,-8.16439679232994));
#18465=CARTESIAN_POINT('Ctrl Pts',(-1.4702867290402E-11,26.3969808928548,
-8.16439679232146));
#18466=CARTESIAN_POINT('Ctrl Pts',(-1.51301075899711E-11,-143.579517970998,
-8.40164026751963));
#18467=CARTESIAN_POINT('Ctrl Pts',(-4.85068927010199,-143.404517970998,
-8.4016402675109));
#18468=CARTESIAN_POINT('Ctrl Pts',(-7.27603390513785,-143.229517970998,
-4.20082013374671));
#18469=CARTESIAN_POINT('Ctrl Pts',(-9.70137854017372,-143.054517970998,
1.74701493417668E-11));
#18470=CARTESIAN_POINT('Ctrl Pts',(-7.27603390512272,-142.879517970998,
4.20082013377292));
#18471=CARTESIAN_POINT('Ctrl Pts',(-4.85068927007173,-142.704517970998,
8.40164026752836));
#18472=CARTESIAN_POINT('Ctrl Pts',(1.5129078685785E-11,-142.529517970998,
8.40164026751963));
#18473=CARTESIAN_POINT('Ctrl Pts',(4.85068927010198,-142.354517970998,8.4016402675109));
#18474=CARTESIAN_POINT('Ctrl Pts',(7.27603390513785,-142.179517970998,4.20082013374672));
#18475=CARTESIAN_POINT('Ctrl Pts',(9.70137854017372,-142.004517970998,-1.74689612655491E-11));
#18476=CARTESIAN_POINT('Ctrl Pts',(7.27603390512273,-141.829517970998,-4.20082013377291));
#18477=CARTESIAN_POINT('Ctrl Pts',(4.85068927007173,-141.654517970998,-8.40164026752836));
#18478=CARTESIAN_POINT('Ctrl Pts',(-1.51301075899711E-11,-141.479517970998,
-8.40164026751963));
#18479=CARTESIAN_POINT('Ctrl Pts',(-4.85068927010199,-141.304517970998,
-8.4016402675109));
#18480=CARTESIAN_POINT('Ctrl Pts',(-7.27603390513785,-141.129517970998,
-4.20082013374671));
#18481=CARTESIAN_POINT('Ctrl Pts',(-9.70137854017372,-140.954517970998,
1.74701493417668E-11));
#18482=CARTESIAN_POINT('Ctrl Pts',(-7.27603390512272,-140.779517970998,
4.20082013377292));
#18483=CARTESIAN_POINT('Ctrl Pts',(-4.85068927007173,-140.604517970998,
8.40164026752836));
#18484=CARTESIAN_POINT('Ctrl Pts',(1.5129078685785E-11,-140.429517970998,
8.40164026751963));
#18485=CARTESIAN_POINT('Ctrl Pts',(4.85068927010198,-140.254517970998,8.4016402675109));
#18486=CARTESIAN_POINT('Ctrl Pts',(7.27603390513785,-140.079517970998,4.20082013374672));
#18487=CARTESIAN_POINT('Ctrl Pts',(9.70137854017372,-139.904517970998,-1.74689612655491E-11));
#18488=CARTESIAN_POINT('Ctrl Pts',(7.27603390512273,-139.729517970998,-4.20082013377291));
#18489=CARTESIAN_POINT('Ctrl Pts',(4.85068927007173,-139.554517970998,-8.40164026752836));
#18490=CARTESIAN_POINT('Ctrl Pts',(-1.51301075899711E-11,-139.379517970998,
-8.40164026751963));
#18491=CARTESIAN_POINT('Ctrl Pts',(-4.85068927010199,-139.204517970998,
-8.4016402675109));
#18492=CARTESIAN_POINT('Ctrl Pts',(-7.27603390513785,-139.029517970998,
-4.20082013374671));
#18493=CARTESIAN_POINT('Ctrl Pts',(-9.70137854017372,-138.854517970998,
1.74701493417668E-11));
#18494=CARTESIAN_POINT('Ctrl Pts',(-7.27603390512272,-138.679517970998,
4.20082013377292));
#18495=CARTESIAN_POINT('Ctrl Pts',(-4.85068927007173,-138.504517970998,
8.40164026752836));
#18496=CARTESIAN_POINT('Ctrl Pts',(1.5129078685785E-11,-138.329517970998,
8.40164026751963));
#18497=CARTESIAN_POINT('Ctrl Pts',(4.85068927010198,-138.154517970998,8.4016402675109));
#18498=CARTESIAN_POINT('Ctrl Pts',(7.27603390513785,-137.979517970998,4.20082013374672));
#18499=CARTESIAN_POINT('Ctrl Pts',(9.70137854017372,-137.804517970998,-1.74689612655491E-11));
#18500=CARTESIAN_POINT('Ctrl Pts',(7.27603390512273,-137.629517970998,-4.20082013377291));
#18501=CARTESIAN_POINT('Ctrl Pts',(4.85068927007173,-137.454517970998,-8.40164026752836));
#18502=CARTESIAN_POINT('Ctrl Pts',(-1.51301075899711E-11,-137.279517970998,
-8.40164026751963));
#18503=CARTESIAN_POINT('Ctrl Pts',(-4.85068927010199,-137.104517970998,
-8.4016402675109));
#18504=CARTESIAN_POINT('Ctrl Pts',(-7.27603390513785,-136.929517970998,
-4.20082013374671));
#18505=CARTESIAN_POINT('Ctrl Pts',(-9.70137854017372,-136.754517970998,
1.74701493417668E-11));
#18506=CARTESIAN_POINT('Ctrl Pts',(-7.27603390512272,-136.579517970998,
4.20082013377292));
#18507=CARTESIAN_POINT('Ctrl Pts',(-4.85068927007173,-136.404517970998,
8.40164026752836));
#18508=CARTESIAN_POINT('Ctrl Pts',(1.5129078685785E-11,-136.229517970998,
8.40164026751963));
#18509=CARTESIAN_POINT('Ctrl Pts',(4.85068927010198,-136.054517970998,8.4016402675109));
#18510=CARTESIAN_POINT('Ctrl Pts',(7.27603390513785,-135.879517970998,4.20082013374672));
#18511=CARTESIAN_POINT('Ctrl Pts',(9.70137854017372,-135.704517970998,-1.74689612655491E-11));
#18512=CARTESIAN_POINT('Ctrl Pts',(7.27603390512273,-135.529517970998,-4.20082013377291));
#18513=CARTESIAN_POINT('Ctrl Pts',(4.85068927007173,-135.354517970998,-8.40164026752836));
#18514=CARTESIAN_POINT('Ctrl Pts',(-1.51301075899711E-11,-135.179517970998,
-8.40164026751963));
#18515=CARTESIAN_POINT('Ctrl Pts',(-4.85068927010199,-135.004517970998,
-8.4016402675109));
#18516=CARTESIAN_POINT('Ctrl Pts',(-7.27603390513785,-134.829517970998,
-4.20082013374671));
#18517=CARTESIAN_POINT('Ctrl Pts',(-9.70137854017372,-134.654517970998,
1.74701493417668E-11));
#18518=CARTESIAN_POINT('Ctrl Pts',(-7.27603390512272,-134.479517970998,
4.20082013377292));
#18519=CARTESIAN_POINT('Ctrl Pts',(-4.85068927007173,-134.304517970998,
8.40164026752836));
#18520=CARTESIAN_POINT('Ctrl Pts',(1.5129078685785E-11,-134.129517970998,
8.40164026751963));
#18521=CARTESIAN_POINT('Ctrl Pts',(4.85068927010198,-133.954517970998,8.4016402675109));
#18522=CARTESIAN_POINT('Ctrl Pts',(7.27603390513785,-133.779517970998,4.20082013374672));
#18523=CARTESIAN_POINT('Ctrl Pts',(9.70137854017372,-133.604517970998,-1.74689612655491E-11));
#18524=CARTESIAN_POINT('Ctrl Pts',(7.27603390512273,-133.429517970998,-4.20082013377291));
#18525=CARTESIAN_POINT('Ctrl Pts',(4.85068927007173,-133.254517970998,-8.40164026752836));
#18526=CARTESIAN_POINT('Ctrl Pts',(-1.51301075899711E-11,-133.079517970998,
-8.40164026751963));
#18527=CARTESIAN_POINT('Ctrl Pts',(-4.85068927010199,-132.904517970998,
-8.4016402675109));
#18528=CARTESIAN_POINT('Ctrl Pts',(-7.27603390513785,-132.729517970998,
-4.20082013374671));
#18529=CARTESIAN_POINT('Ctrl Pts',(-9.70137854017372,-132.554517970998,
1.74701493417668E-11));
#18530=CARTESIAN_POINT('Ctrl Pts',(-7.27603390512272,-132.379517970998,
4.20082013377292));
#18531=CARTESIAN_POINT('Ctrl Pts',(-4.85068927007173,-132.204517970998,
8.40164026752836));
#18532=CARTESIAN_POINT('Ctrl Pts',(1.5129078685785E-11,-132.029517970998,
8.40164026751963));
#18533=CARTESIAN_POINT('Ctrl Pts',(4.85068927010198,-131.854517970998,8.4016402675109));
#18534=CARTESIAN_POINT('Ctrl Pts',(7.27603390513785,-131.679517970998,4.20082013374672));
#18535=CARTESIAN_POINT('Ctrl Pts',(9.70137854017372,-131.504517970998,-1.74689612655491E-11));
#18536=CARTESIAN_POINT('Ctrl Pts',(7.27603390512273,-131.329517970998,-4.20082013377291));
#18537=CARTESIAN_POINT('Ctrl Pts',(4.85068927007173,-131.154517970998,-8.40164026752836));
#18538=CARTESIAN_POINT('Ctrl Pts',(-1.51301075899711E-11,-130.979517970998,
-8.40164026751963));
#18539=CARTESIAN_POINT('Ctrl Pts',(-4.85068927010199,-130.804517970998,
-8.4016402675109));
#18540=CARTESIAN_POINT('Ctrl Pts',(-7.27603390513785,-130.629517970998,
-4.20082013374671));
#18541=CARTESIAN_POINT('Ctrl Pts',(-9.70137854017372,-130.454517970998,
1.74701493417668E-11));
#18542=CARTESIAN_POINT('Ctrl Pts',(-7.27603390512272,-130.279517970998,
4.20082013377292));
#18543=CARTESIAN_POINT('Ctrl Pts',(-4.85068927007173,-130.104517970998,
8.40164026752836));
#18544=CARTESIAN_POINT('Ctrl Pts',(1.5129078685785E-11,-129.929517970998,
8.40164026751963));
#18545=CARTESIAN_POINT('Ctrl Pts',(4.85068927010198,-129.754517970998,8.4016402675109));
#18546=CARTESIAN_POINT('Ctrl Pts',(7.27603390513785,-129.579517970998,4.20082013374672));
#18547=CARTESIAN_POINT('Ctrl Pts',(9.70137854017372,-129.404517970998,-1.74689612655491E-11));
#18548=CARTESIAN_POINT('Ctrl Pts',(7.27603390512273,-129.229517970998,-4.20082013377291));
#18549=CARTESIAN_POINT('Ctrl Pts',(4.85068927007173,-129.054517970998,-8.40164026752836));
#18550=CARTESIAN_POINT('Ctrl Pts',(-1.51301075899711E-11,-128.879517970998,
-8.40164026751963));
#18551=CARTESIAN_POINT('Ctrl Pts',(-4.85068927010199,-128.704517970998,
-8.4016402675109));
#18552=CARTESIAN_POINT('Ctrl Pts',(-7.27603390513785,-128.529517970998,
-4.20082013374671));
#18553=CARTESIAN_POINT('Ctrl Pts',(-9.70137854017372,-128.354517970998,
1.74701493417668E-11));
#18554=CARTESIAN_POINT('Ctrl Pts',(-7.27603390512272,-128.179517970998,
4.20082013377292));
#18555=CARTESIAN_POINT('Ctrl Pts',(-4.85068927007173,-128.004517970998,
8.40164026752836));
#18556=CARTESIAN_POINT('Ctrl Pts',(1.5129078685785E-11,-127.829517970998,
8.40164026751963));
#18557=CARTESIAN_POINT('Ctrl Pts',(4.85068927010198,-127.654517970998,8.4016402675109));
#18558=CARTESIAN_POINT('Ctrl Pts',(7.27603390513785,-127.479517970998,4.20082013374672));
#18559=CARTESIAN_POINT('Ctrl Pts',(9.70137854017372,-127.304517970998,-1.74689612655491E-11));
#18560=CARTESIAN_POINT('Ctrl Pts',(7.27603390512273,-127.129517970998,-4.20082013377291));
#18561=CARTESIAN_POINT('Ctrl Pts',(4.85068927007173,-126.954517970998,-8.40164026752836));
#18562=CARTESIAN_POINT('Ctrl Pts',(-1.51301075899711E-11,-126.779517970998,
-8.40164026751963));
#18563=CARTESIAN_POINT('Ctrl Pts',(-4.85068927010199,-126.604517970998,
-8.4016402675109));
#18564=CARTESIAN_POINT('Ctrl Pts',(-7.27603390513785,-126.429517970998,
-4.20082013374671));
#18565=CARTESIAN_POINT('Ctrl Pts',(-9.70137854017372,-126.254517970998,
1.74701493417668E-11));
#18566=CARTESIAN_POINT('Ctrl Pts',(-7.27603390512272,-126.079517970998,
4.20082013377292));
#18567=CARTESIAN_POINT('Ctrl Pts',(-4.85068927007173,-125.904517970998,
8.40164026752836));
#18568=CARTESIAN_POINT('Ctrl Pts',(1.5129078685785E-11,-125.729517970998,
8.40164026751963));
#18569=CARTESIAN_POINT('Ctrl Pts',(4.85068927010198,-125.554517970998,8.4016402675109));
#18570=CARTESIAN_POINT('Ctrl Pts',(7.27603390513785,-125.379517970998,4.20082013374672));
#18571=CARTESIAN_POINT('Ctrl Pts',(9.70137854017372,-125.204517970998,-1.74689612655491E-11));
#18572=CARTESIAN_POINT('Ctrl Pts',(7.27603390512273,-125.029517970998,-4.20082013377291));
#18573=CARTESIAN_POINT('Ctrl Pts',(4.85068927007173,-124.854517970998,-8.40164026752836));
#18574=CARTESIAN_POINT('Ctrl Pts',(-1.51301075899711E-11,-124.679517970998,
-8.40164026751963));
#18575=CARTESIAN_POINT('Ctrl Pts',(-4.85068927010199,-124.504517970998,
-8.4016402675109));
#18576=CARTESIAN_POINT('Ctrl Pts',(-7.27603390513785,-124.329517970998,
-4.20082013374671));
#18577=CARTESIAN_POINT('Ctrl Pts',(-9.70137854017372,-124.154517970998,
1.74701493417668E-11));
#18578=CARTESIAN_POINT('Ctrl Pts',(-7.27603390512272,-123.979517970998,
4.20082013377292));
#18579=CARTESIAN_POINT('Ctrl Pts',(-4.85068927007173,-123.804517970998,
8.40164026752836));
#18580=CARTESIAN_POINT('Ctrl Pts',(1.5129078685785E-11,-123.629517970998,
8.40164026751963));
#18581=CARTESIAN_POINT('Ctrl Pts',(4.85068927010198,-123.454517970998,8.4016402675109));
#18582=CARTESIAN_POINT('Ctrl Pts',(7.27603390513785,-123.279517970998,4.20082013374672));
#18583=CARTESIAN_POINT('Ctrl Pts',(9.70137854017372,-123.104517970998,-1.74689612655491E-11));
#18584=CARTESIAN_POINT('Ctrl Pts',(7.27603390512273,-122.929517970998,-4.20082013377291));
#18585=CARTESIAN_POINT('Ctrl Pts',(4.85068927007173,-122.754517970998,-8.40164026752836));
#18586=CARTESIAN_POINT('Ctrl Pts',(-1.51301075899711E-11,-122.579517970998,
-8.40164026751963));
#18587=CARTESIAN_POINT('Ctrl Pts',(-4.85068927010199,-122.404517970998,
-8.4016402675109));
#18588=CARTESIAN_POINT('Ctrl Pts',(-7.27603390513785,-122.229517970998,
-4.20082013374671));
#18589=CARTESIAN_POINT('Ctrl Pts',(-9.70137854017372,-122.054517970998,
1.74701493417668E-11));
#18590=CARTESIAN_POINT('Ctrl Pts',(-7.27603390512272,-121.879517970998,
4.20082013377292));
#18591=CARTESIAN_POINT('Ctrl Pts',(-4.85068927007173,-121.704517970998,
8.40164026752836));
#18592=CARTESIAN_POINT('Ctrl Pts',(1.5129078685785E-11,-121.529517970998,
8.40164026751963));
#18593=CARTESIAN_POINT('Ctrl Pts',(4.85068927010198,-121.354517970998,8.4016402675109));
#18594=CARTESIAN_POINT('Ctrl Pts',(7.27603390513785,-121.179517970998,4.20082013374672));
#18595=CARTESIAN_POINT('Ctrl Pts',(9.70137854017372,-121.004517970998,-1.74689612655491E-11));
#18596=CARTESIAN_POINT('Ctrl Pts',(7.27603390512273,-120.829517970998,-4.20082013377291));
#18597=CARTESIAN_POINT('Ctrl Pts',(4.85068927007173,-120.654517970998,-8.40164026752836));
#18598=CARTESIAN_POINT('Ctrl Pts',(-1.51301075899711E-11,-120.479517970998,
-8.40164026751963));
#18599=CARTESIAN_POINT('Ctrl Pts',(-4.85068927010199,-120.304517970998,
-8.4016402675109));
#18600=CARTESIAN_POINT('Ctrl Pts',(-7.27603390513785,-120.129517970998,
-4.20082013374671));
#18601=CARTESIAN_POINT('Ctrl Pts',(-9.70137854017372,-119.954517970998,
1.74701493417668E-11));
#18602=CARTESIAN_POINT('Ctrl Pts',(-7.27603390512272,-119.779517970998,
4.20082013377292));
#18603=CARTESIAN_POINT('Ctrl Pts',(-4.85068927007173,-119.604517970998,
8.40164026752836));
#18604=CARTESIAN_POINT('Ctrl Pts',(1.5129078685785E-11,-119.429517970998,
8.40164026751963));
#18605=CARTESIAN_POINT('Ctrl Pts',(4.85068927010198,-119.254517970998,8.4016402675109));
#18606=CARTESIAN_POINT('Ctrl Pts',(7.27603390513785,-119.079517970998,4.20082013374672));
#18607=CARTESIAN_POINT('Ctrl Pts',(9.70137854017372,-118.904517970998,-1.74689612655491E-11));
#18608=CARTESIAN_POINT('Ctrl Pts',(7.27603390512273,-118.729517970998,-4.20082013377291));
#18609=CARTESIAN_POINT('Ctrl Pts',(4.85068927007173,-118.554517970998,-8.40164026752836));
#18610=CARTESIAN_POINT('Ctrl Pts',(-1.51301075899711E-11,-118.379517970998,
-8.40164026751963));
#18611=CARTESIAN_POINT('Ctrl Pts',(-4.85068927010199,-118.204517970998,
-8.4016402675109));
#18612=CARTESIAN_POINT('Ctrl Pts',(-7.27603390513785,-118.029517970998,
-4.20082013374671));
#18613=CARTESIAN_POINT('Ctrl Pts',(-9.70137854017372,-117.854517970998,
1.74701493417668E-11));
#18614=CARTESIAN_POINT('Ctrl Pts',(-7.27603390512272,-117.679517970998,
4.20082013377292));
#18615=CARTESIAN_POINT('Ctrl Pts',(-4.85068927007173,-117.504517970998,
8.40164026752836));
#18616=CARTESIAN_POINT('Ctrl Pts',(1.5129078685785E-11,-117.329517970998,
8.40164026751963));
#18617=CARTESIAN_POINT('Ctrl Pts',(4.85068927010198,-117.154517970998,8.4016402675109));
#18618=CARTESIAN_POINT('Ctrl Pts',(7.27603390513785,-116.979517970998,4.20082013374672));
#18619=CARTESIAN_POINT('Ctrl Pts',(9.70137854017372,-116.804517970998,-1.74689612655491E-11));
#18620=CARTESIAN_POINT('Ctrl Pts',(7.27603390512273,-116.629517970998,-4.20082013377291));
#18621=CARTESIAN_POINT('Ctrl Pts',(4.85068927007173,-116.454517970998,-8.40164026752836));
#18622=CARTESIAN_POINT('Ctrl Pts',(-1.51301075899711E-11,-116.279517970998,
-8.40164026751963));
#18623=CARTESIAN_POINT('Ctrl Pts',(-4.85068927010199,-116.104517970998,
-8.4016402675109));
#18624=CARTESIAN_POINT('Ctrl Pts',(-7.27603390513785,-115.929517970998,
-4.20082013374671));
#18625=CARTESIAN_POINT('Ctrl Pts',(-9.70137854017372,-115.754517970998,
1.74701493417668E-11));
#18626=CARTESIAN_POINT('Ctrl Pts',(-7.27603390512272,-115.579517970998,
4.20082013377292));
#18627=CARTESIAN_POINT('Ctrl Pts',(-4.85068927007173,-115.404517970998,
8.40164026752836));
#18628=CARTESIAN_POINT('Ctrl Pts',(1.5129078685785E-11,-115.229517970998,
8.40164026751963));
#18629=CARTESIAN_POINT('Ctrl Pts',(4.85068927010198,-115.054517970998,8.4016402675109));
#18630=CARTESIAN_POINT('Ctrl Pts',(7.27603390513785,-114.879517970998,4.20082013374672));
#18631=CARTESIAN_POINT('Ctrl Pts',(9.70137854017372,-114.704517970998,-1.74689612655491E-11));
#18632=CARTESIAN_POINT('Ctrl Pts',(7.27603390512273,-114.529517970998,-4.20082013377291));
#18633=CARTESIAN_POINT('Ctrl Pts',(4.85068927007173,-114.354517970998,-8.40164026752836));
#18634=CARTESIAN_POINT('Ctrl Pts',(-1.51301075899711E-11,-114.179517970998,
-8.40164026751963));
#18635=CARTESIAN_POINT('Ctrl Pts',(-4.85068927010199,-114.004517970998,
-8.4016402675109));
#18636=CARTESIAN_POINT('Ctrl Pts',(-7.27603390513785,-113.829517970998,
-4.20082013374671));
#18637=CARTESIAN_POINT('Ctrl Pts',(-9.70137854017372,-113.654517970998,
1.74701493417668E-11));
#18638=CARTESIAN_POINT('Ctrl Pts',(-7.27603390512272,-113.479517970998,
4.20082013377292));
#18639=CARTESIAN_POINT('Ctrl Pts',(-4.85068927007173,-113.304517970998,
8.40164026752836));
#18640=CARTESIAN_POINT('Ctrl Pts',(1.5129078685785E-11,-113.129517970998,
8.40164026751963));
#18641=CARTESIAN_POINT('Ctrl Pts',(4.85068927010198,-112.954517970998,8.4016402675109));
#18642=CARTESIAN_POINT('Ctrl Pts',(7.27603390513785,-112.779517970998,4.20082013374672));
#18643=CARTESIAN_POINT('Ctrl Pts',(9.70137854017372,-112.604517970998,-1.74689612655491E-11));
#18644=CARTESIAN_POINT('Ctrl Pts',(7.27603390512273,-112.429517970998,-4.20082013377291));
#18645=CARTESIAN_POINT('Ctrl Pts',(4.85068927007173,-112.254517970998,-8.40164026752836));
#18646=CARTESIAN_POINT('Ctrl Pts',(-1.51301075899711E-11,-112.079517970998,
-8.40164026751963));
#18647=CARTESIAN_POINT('Ctrl Pts',(-4.85068927010199,-111.904517970998,
-8.4016402675109));
#18648=CARTESIAN_POINT('Ctrl Pts',(-7.27603390513785,-111.729517970998,
-4.20082013374671));
#18649=CARTESIAN_POINT('Ctrl Pts',(-9.70137854017372,-111.554517970998,
1.74701493417668E-11));
#18650=CARTESIAN_POINT('Ctrl Pts',(-7.27603390512272,-111.379517970998,
4.20082013377292));
#18651=CARTESIAN_POINT('Ctrl Pts',(-4.85068927007173,-111.204517970998,
8.40164026752836));
#18652=CARTESIAN_POINT('Ctrl Pts',(1.5129078685785E-11,-111.029517970998,
8.40164026751963));
#18653=CARTESIAN_POINT('Ctrl Pts',(4.85068927010198,-110.854517970998,8.4016402675109));
#18654=CARTESIAN_POINT('Ctrl Pts',(7.27603390513785,-110.679517970998,4.20082013374672));
#18655=CARTESIAN_POINT('Ctrl Pts',(9.70137854017372,-110.504517970998,-1.74689612655491E-11));
#18656=CARTESIAN_POINT('Ctrl Pts',(7.27603390512273,-110.329517970998,-4.20082013377291));
#18657=CARTESIAN_POINT('Ctrl Pts',(4.85068927007173,-110.154517970998,-8.40164026752836));
#18658=CARTESIAN_POINT('Ctrl Pts',(-1.51301075899711E-11,-109.979517970998,
-8.40164026751963));
#18659=CARTESIAN_POINT('Ctrl Pts',(-4.85068927010199,-109.804517970998,
-8.4016402675109));
#18660=CARTESIAN_POINT('Ctrl Pts',(-7.27603390513785,-109.629517970998,
-4.20082013374671));
#18661=CARTESIAN_POINT('Ctrl Pts',(-9.70137854017372,-109.454517970998,
1.74701493417668E-11));
#18662=CARTESIAN_POINT('Ctrl Pts',(-7.27603390512272,-109.279517970998,
4.20082013377292));
#18663=CARTESIAN_POINT('Ctrl Pts',(-4.85068927007173,-109.104517970998,
8.40164026752836));
#18664=CARTESIAN_POINT('Ctrl Pts',(1.5129078685785E-11,-108.929517970998,
8.40164026751963));
#18665=CARTESIAN_POINT('Ctrl Pts',(4.85068927010198,-108.754517970998,8.4016402675109));
#18666=CARTESIAN_POINT('Ctrl Pts',(7.27603390513785,-108.579517970998,4.20082013374672));
#18667=CARTESIAN_POINT('Ctrl Pts',(9.70137854017372,-108.404517970998,-1.74689612655491E-11));
#18668=CARTESIAN_POINT('Ctrl Pts',(7.27603390512273,-108.229517970998,-4.20082013377291));
#18669=CARTESIAN_POINT('Ctrl Pts',(4.85068927007173,-108.054517970998,-8.40164026752836));
#18670=CARTESIAN_POINT('Ctrl Pts',(-1.51301075899711E-11,-107.879517970998,
-8.40164026751963));
#18671=CARTESIAN_POINT('Ctrl Pts',(-4.85068927010199,-107.704517970998,
-8.4016402675109));
#18672=CARTESIAN_POINT('Ctrl Pts',(-7.27603390513785,-107.529517970998,
-4.20082013374671));
#18673=CARTESIAN_POINT('Ctrl Pts',(-9.70137854017372,-107.354517970998,
1.74701493417668E-11));
#18674=CARTESIAN_POINT('Ctrl Pts',(-7.27603390512272,-107.179517970998,
4.20082013377292));
#18675=CARTESIAN_POINT('Ctrl Pts',(-4.85068927007173,-107.004517970998,
8.40164026752836));
#18676=CARTESIAN_POINT('Ctrl Pts',(1.5129078685785E-11,-106.829517970998,
8.40164026751963));
#18677=CARTESIAN_POINT('Ctrl Pts',(4.85068927010198,-106.654517970998,8.4016402675109));
#18678=CARTESIAN_POINT('Ctrl Pts',(7.27603390513785,-106.479517970998,4.20082013374672));
#18679=CARTESIAN_POINT('Ctrl Pts',(9.70137854017372,-106.304517970998,-1.74689612655491E-11));
#18680=CARTESIAN_POINT('Ctrl Pts',(7.27603390512273,-106.129517970998,-4.20082013377291));
#18681=CARTESIAN_POINT('Ctrl Pts',(4.85068927007173,-105.954517970998,-8.40164026752836));
#18682=CARTESIAN_POINT('Ctrl Pts',(-1.51301075899711E-11,-105.779517970998,
-8.40164026751963));
#18683=CARTESIAN_POINT('Ctrl Pts',(-4.85068927010199,-105.604517970998,
-8.4016402675109));
#18684=CARTESIAN_POINT('Ctrl Pts',(-7.27603390513785,-105.429517970998,
-4.20082013374671));
#18685=CARTESIAN_POINT('Ctrl Pts',(-9.70137854017372,-105.254517970998,
1.74701493417668E-11));
#18686=CARTESIAN_POINT('Ctrl Pts',(-7.27603390512272,-105.079517970998,
4.20082013377292));
#18687=CARTESIAN_POINT('Ctrl Pts',(-4.85068927007173,-104.904517970998,
8.40164026752836));
#18688=CARTESIAN_POINT('Ctrl Pts',(1.5129078685785E-11,-104.729517970998,
8.40164026751963));
#18689=CARTESIAN_POINT('Ctrl Pts',(4.85068927010198,-104.554517970998,8.4016402675109));
#18690=CARTESIAN_POINT('Ctrl Pts',(7.27603390513785,-104.379517970998,4.20082013374672));
#18691=CARTESIAN_POINT('Ctrl Pts',(9.70137854017372,-104.204517970998,-1.74689612655491E-11));
#18692=CARTESIAN_POINT('Ctrl Pts',(7.27603390512273,-104.029517970998,-4.20082013377291));
#18693=CARTESIAN_POINT('Ctrl Pts',(4.85068927007173,-103.854517970998,-8.40164026752836));
#18694=CARTESIAN_POINT('Ctrl Pts',(-1.51301075899711E-11,-103.679517970998,
-8.40164026751963));
#18695=CARTESIAN_POINT('Ctrl Pts',(-4.85068927010199,-103.504517970998,
-8.4016402675109));
#18696=CARTESIAN_POINT('Ctrl Pts',(-7.27603390513785,-103.329517970998,
-4.20082013374671));
#18697=CARTESIAN_POINT('Ctrl Pts',(-9.70137854017372,-103.154517970998,
1.74701493417668E-11));
#18698=CARTESIAN_POINT('Ctrl Pts',(-7.27603390512272,-102.979517970998,
4.20082013377292));
#18699=CARTESIAN_POINT('Ctrl Pts',(-4.85068927007173,-102.804517970998,
8.40164026752836));
#18700=CARTESIAN_POINT('Ctrl Pts',(1.5129078685785E-11,-102.629517970998,
8.40164026751963));
#18701=CARTESIAN_POINT('Ctrl Pts',(4.85068927010198,-102.454517970998,8.4016402675109));
#18702=CARTESIAN_POINT('Ctrl Pts',(7.27603390513785,-102.279517970998,4.20082013374672));
#18703=CARTESIAN_POINT('Ctrl Pts',(9.70137854017372,-102.104517970998,-1.74689612655491E-11));
#18704=CARTESIAN_POINT('Ctrl Pts',(7.27603390512273,-101.929517970998,-4.20082013377291));
#18705=CARTESIAN_POINT('Ctrl Pts',(4.85068927007173,-101.754517970998,-8.40164026752836));
#18706=CARTESIAN_POINT('Ctrl Pts',(-1.51301075899711E-11,-101.579517970998,
-8.40164026751963));
#18707=CARTESIAN_POINT('Ctrl Pts',(-4.85068927010199,-101.404517970998,
-8.4016402675109));
#18708=CARTESIAN_POINT('Ctrl Pts',(-7.27603390513785,-101.229517970998,
-4.20082013374671));
#18709=CARTESIAN_POINT('Ctrl Pts',(-9.70137854017372,-101.054517970998,
1.74701493417668E-11));
#18710=CARTESIAN_POINT('Ctrl Pts',(-7.27603390512272,-100.879517970998,
4.20082013377292));
#18711=CARTESIAN_POINT('Ctrl Pts',(-4.85068927007173,-100.704517970998,
8.40164026752836));
#18712=CARTESIAN_POINT('Ctrl Pts',(1.5129078685785E-11,-100.529517970998,
8.40164026751963));
#18713=CARTESIAN_POINT('Ctrl Pts',(4.85068927010198,-100.354517970998,8.4016402675109));
#18714=CARTESIAN_POINT('Ctrl Pts',(7.27603390513785,-100.179517970998,4.20082013374672));
#18715=CARTESIAN_POINT('Ctrl Pts',(9.70137854017372,-100.004517970998,-1.74689612655491E-11));
#18716=CARTESIAN_POINT('Ctrl Pts',(7.27603390512273,-99.8295179709984,-4.20082013377291));
#18717=CARTESIAN_POINT('Ctrl Pts',(4.85068927007173,-99.6545179709984,-8.40164026752836));
#18718=CARTESIAN_POINT('Ctrl Pts',(-1.51301075899711E-11,-99.4795179709984,
-8.40164026751963));
#18719=CARTESIAN_POINT('Ctrl Pts',(-4.85068927010199,-99.3045179709984,
-8.4016402675109));
#18720=CARTESIAN_POINT('Ctrl Pts',(-7.27603390513785,-99.1295179709984,
-4.20082013374671));
#18721=CARTESIAN_POINT('Ctrl Pts',(-9.70137854017372,-98.9545179709984,
1.74701493417668E-11));
#18722=CARTESIAN_POINT('Ctrl Pts',(-7.27603390512272,-98.7795179709984,
4.20082013377292));
#18723=CARTESIAN_POINT('Ctrl Pts',(-4.85068927007173,-98.6045179709984,
8.40164026752836));
#18724=CARTESIAN_POINT('Ctrl Pts',(1.5129078685785E-11,-98.4295179709984,
8.40164026751963));
#18725=CARTESIAN_POINT('Ctrl Pts',(4.85068927010198,-98.2545179709984,8.4016402675109));
#18726=CARTESIAN_POINT('Ctrl Pts',(7.27603390513785,-98.0795179709984,4.20082013374672));
#18727=CARTESIAN_POINT('Ctrl Pts',(9.70137854017372,-97.9045179709984,-1.74689612655491E-11));
#18728=CARTESIAN_POINT('Ctrl Pts',(7.27603390512273,-97.7295179709984,-4.20082013377291));
#18729=CARTESIAN_POINT('Ctrl Pts',(4.85068927007173,-97.5545179709984,-8.40164026752836));
#18730=CARTESIAN_POINT('Ctrl Pts',(-1.51301075899711E-11,-97.3795179709984,
-8.40164026751963));
#18731=CARTESIAN_POINT('Ctrl Pts',(-4.85068927010199,-97.2045179709984,
-8.4016402675109));
#18732=CARTESIAN_POINT('Ctrl Pts',(-7.27603390513785,-97.0295179709984,
-4.20082013374671));
#18733=CARTESIAN_POINT('Ctrl Pts',(-9.70137854017372,-96.8545179709984,
1.74701493417668E-11));
#18734=CARTESIAN_POINT('Ctrl Pts',(-7.27603390512272,-96.6795179709984,
4.20082013377292));
#18735=CARTESIAN_POINT('Ctrl Pts',(-4.85068927007173,-96.5045179709984,
8.40164026752836));
#18736=CARTESIAN_POINT('Ctrl Pts',(1.5129078685785E-11,-96.3295179709984,
8.40164026751963));
#18737=CARTESIAN_POINT('Ctrl Pts',(4.85068927010198,-96.1545179709984,8.4016402675109));
#18738=CARTESIAN_POINT('Ctrl Pts',(7.27603390513785,-95.9795179709984,4.20082013374672));
#18739=CARTESIAN_POINT('Ctrl Pts',(9.70137854017372,-95.8045179709984,-1.74689612655491E-11));
#18740=CARTESIAN_POINT('Ctrl Pts',(7.27603390512273,-95.6295179709984,-4.20082013377291));
#18741=CARTESIAN_POINT('Ctrl Pts',(4.85068927007173,-95.4545179709984,-8.40164026752836));
#18742=CARTESIAN_POINT('Ctrl Pts',(-1.51301075899711E-11,-95.2795179709984,
-8.40164026751963));
#18743=CARTESIAN_POINT('Ctrl Pts',(-4.85068927010199,-95.1045179709984,
-8.4016402675109));
#18744=CARTESIAN_POINT('Ctrl Pts',(-7.27603390513785,-94.9295179709984,
-4.20082013374671));
#18745=CARTESIAN_POINT('Ctrl Pts',(-9.70137854017372,-94.7545179709984,
1.74701493417668E-11));
#18746=CARTESIAN_POINT('Ctrl Pts',(-7.27603390512272,-94.5795179709984,
4.20082013377292));
#18747=CARTESIAN_POINT('Ctrl Pts',(-4.85068927007173,-94.4045179709984,
8.40164026752836));
#18748=CARTESIAN_POINT('Ctrl Pts',(1.5129078685785E-11,-94.2295179709984,
8.40164026751963));
#18749=CARTESIAN_POINT('Ctrl Pts',(4.85068927010198,-94.0545179709984,8.4016402675109));
#18750=CARTESIAN_POINT('Ctrl Pts',(7.27603390513785,-93.8795179709984,4.20082013374672));
#18751=CARTESIAN_POINT('Ctrl Pts',(9.70137854017372,-93.7045179709984,-1.74689612655491E-11));
#18752=CARTESIAN_POINT('Ctrl Pts',(7.27603390512273,-93.5295179709984,-4.20082013377291));
#18753=CARTESIAN_POINT('Ctrl Pts',(4.85068927007173,-93.3545179709984,-8.40164026752836));
#18754=CARTESIAN_POINT('Ctrl Pts',(-1.51301075899711E-11,-93.1795179709984,
-8.40164026751963));
#18755=CARTESIAN_POINT('Ctrl Pts',(-4.85068927010199,-93.0045179709984,
-8.4016402675109));
#18756=CARTESIAN_POINT('Ctrl Pts',(-7.27603390513785,-92.8295179709984,
-4.20082013374671));
#18757=CARTESIAN_POINT('Ctrl Pts',(-9.70137854017372,-92.6545179709984,
1.74701493417668E-11));
#18758=CARTESIAN_POINT('Ctrl Pts',(-7.27603390512272,-92.4795179709984,
4.20082013377292));
#18759=CARTESIAN_POINT('Ctrl Pts',(-4.85068927007173,-92.3045179709984,
8.40164026752836));
#18760=CARTESIAN_POINT('Ctrl Pts',(1.5129078685785E-11,-92.1295179709984,
8.40164026751963));
#18761=CARTESIAN_POINT('Ctrl Pts',(4.85068927010198,-91.9545179709984,8.4016402675109));
#18762=CARTESIAN_POINT('Ctrl Pts',(7.27603390513785,-91.7795179709984,4.20082013374672));
#18763=CARTESIAN_POINT('Ctrl Pts',(9.70137854017372,-91.6045179709984,-1.74689612655491E-11));
#18764=CARTESIAN_POINT('Ctrl Pts',(7.27603390512273,-91.4295179709984,-4.20082013377291));
#18765=CARTESIAN_POINT('Ctrl Pts',(4.85068927007173,-91.2545179709984,-8.40164026752836));
#18766=CARTESIAN_POINT('Ctrl Pts',(-1.51301075899711E-11,-91.0795179709984,
-8.40164026751963));
#18767=CARTESIAN_POINT('Ctrl Pts',(-4.85068927010199,-90.9045179709984,
-8.4016402675109));
#18768=CARTESIAN_POINT('Ctrl Pts',(-7.27603390513785,-90.7295179709984,
-4.20082013374671));
#18769=CARTESIAN_POINT('Ctrl Pts',(-9.70137854017372,-90.5545179709984,
1.74701493417668E-11));
#18770=CARTESIAN_POINT('Ctrl Pts',(-7.27603390512272,-90.3795179709984,
4.20082013377292));
#18771=CARTESIAN_POINT('Ctrl Pts',(-4.85068927007173,-90.2045179709984,
8.40164026752836));
#18772=CARTESIAN_POINT('Ctrl Pts',(1.5129078685785E-11,-90.0295179709984,
8.40164026751963));
#18773=CARTESIAN_POINT('Ctrl Pts',(4.85068927010198,-89.8545179709984,8.4016402675109));
#18774=CARTESIAN_POINT('Ctrl Pts',(7.27603390513785,-89.6795179709984,4.20082013374672));
#18775=CARTESIAN_POINT('Ctrl Pts',(9.70137854017372,-89.5045179709984,-1.74689612655491E-11));
#18776=CARTESIAN_POINT('Ctrl Pts',(7.27603390512273,-89.3295179709984,-4.20082013377291));
#18777=CARTESIAN_POINT('Ctrl Pts',(4.85068927007173,-89.1545179709984,-8.40164026752836));
#18778=CARTESIAN_POINT('Ctrl Pts',(-1.51301075899711E-11,-88.9795179709984,
-8.40164026751963));
#18779=CARTESIAN_POINT('Ctrl Pts',(-4.85068927010199,-88.8045179709984,
-8.4016402675109));
#18780=CARTESIAN_POINT('Ctrl Pts',(-7.27603390513785,-88.6295179709984,
-4.20082013374671));
#18781=CARTESIAN_POINT('Ctrl Pts',(-9.70137854017372,-88.4545179709984,
1.74701493417668E-11));
#18782=CARTESIAN_POINT('Ctrl Pts',(-7.27603390512272,-88.2795179709984,
4.20082013377292));
#18783=CARTESIAN_POINT('Ctrl Pts',(-4.85068927007173,-88.1045179709984,
8.40164026752836));
#18784=CARTESIAN_POINT('Ctrl Pts',(1.5129078685785E-11,-87.9295179709984,
8.40164026751963));
#18785=CARTESIAN_POINT('Ctrl Pts',(4.85068927010198,-87.7545179709984,8.4016402675109));
#18786=CARTESIAN_POINT('Ctrl Pts',(7.27603390513785,-87.5795179709984,4.20082013374672));
#18787=CARTESIAN_POINT('Ctrl Pts',(9.70137854017372,-87.4045179709984,-1.74689612655491E-11));
#18788=CARTESIAN_POINT('Ctrl Pts',(7.27603390512273,-87.2295179709984,-4.20082013377291));
#18789=CARTESIAN_POINT('Ctrl Pts',(4.85068927007173,-87.0545179709984,-8.40164026752836));
#18790=CARTESIAN_POINT('Ctrl Pts',(-1.51301075899711E-11,-86.8795179709984,
-8.40164026751963));
#18791=CARTESIAN_POINT('Ctrl Pts',(-4.85068927010199,-86.7045179709984,
-8.4016402675109));
#18792=CARTESIAN_POINT('Ctrl Pts',(-7.27603390513785,-86.5295179709984,
-4.20082013374671));
#18793=CARTESIAN_POINT('Ctrl Pts',(-9.70137854017372,-86.3545179709984,
1.74701493417668E-11));
#18794=CARTESIAN_POINT('Ctrl Pts',(-7.27603390512272,-86.1795179709984,
4.20082013377292));
#18795=CARTESIAN_POINT('Ctrl Pts',(-4.85068927007173,-86.0045179709984,
8.40164026752836));
#18796=CARTESIAN_POINT('Ctrl Pts',(1.5129078685785E-11,-85.8295179709984,
8.40164026751963));
#18797=CARTESIAN_POINT('Ctrl Pts',(4.85068927010198,-85.6545179709984,8.4016402675109));
#18798=CARTESIAN_POINT('Ctrl Pts',(7.27603390513785,-85.4795179709984,4.20082013374672));
#18799=CARTESIAN_POINT('Ctrl Pts',(9.70137854017372,-85.3045179709984,-1.74689612655491E-11));
#18800=CARTESIAN_POINT('Ctrl Pts',(7.27603390512273,-85.1295179709984,-4.20082013377291));
#18801=CARTESIAN_POINT('Ctrl Pts',(4.85068927007173,-84.9545179709984,-8.40164026752836));
#18802=CARTESIAN_POINT('Ctrl Pts',(-1.51301075899711E-11,-84.7795179709984,
-8.40164026751963));
#18803=CARTESIAN_POINT('Ctrl Pts',(-4.85068927010199,-84.6045179709984,
-8.4016402675109));
#18804=CARTESIAN_POINT('Ctrl Pts',(-7.27603390513785,-84.4295179709984,
-4.20082013374671));
#18805=CARTESIAN_POINT('Ctrl Pts',(-9.70137854017372,-84.2545179709984,
1.74701493417668E-11));
#18806=CARTESIAN_POINT('Ctrl Pts',(-7.27603390512272,-84.0795179709984,
4.20082013377292));
#18807=CARTESIAN_POINT('Ctrl Pts',(-4.85068927007173,-83.9045179709984,
8.40164026752836));
#18808=CARTESIAN_POINT('Ctrl Pts',(1.5129078685785E-11,-83.7295179709984,
8.40164026751963));
#18809=CARTESIAN_POINT('Ctrl Pts',(4.85068927010198,-83.5545179709984,8.4016402675109));
#18810=CARTESIAN_POINT('Ctrl Pts',(7.27603390513785,-83.3795179709984,4.20082013374672));
#18811=CARTESIAN_POINT('Ctrl Pts',(9.70137854017372,-83.2045179709984,-1.74689612655491E-11));
#18812=CARTESIAN_POINT('Ctrl Pts',(7.27603390512273,-83.0295179709984,-4.20082013377291));
#18813=CARTESIAN_POINT('Ctrl Pts',(4.85068927007173,-82.8545179709984,-8.40164026752836));
#18814=CARTESIAN_POINT('Ctrl Pts',(-1.51301075899711E-11,-82.6795179709984,
-8.40164026751963));
#18815=CARTESIAN_POINT('Ctrl Pts',(-4.85068927010199,-82.5045179709984,
-8.4016402675109));
#18816=CARTESIAN_POINT('Ctrl Pts',(-7.27603390513785,-82.3295179709984,
-4.20082013374671));
#18817=CARTESIAN_POINT('Ctrl Pts',(-9.70137854017372,-82.1545179709984,
1.74701493417668E-11));
#18818=CARTESIAN_POINT('Ctrl Pts',(-7.27603390512272,-81.9795179709984,
4.20082013377292));
#18819=CARTESIAN_POINT('Ctrl Pts',(-4.85068927007173,-81.8045179709984,
8.40164026752836));
#18820=CARTESIAN_POINT('Ctrl Pts',(1.5129078685785E-11,-81.6295179709984,
8.40164026751963));
#18821=CARTESIAN_POINT('Ctrl Pts',(4.85068927010198,-81.4545179709984,8.4016402675109));
#18822=CARTESIAN_POINT('Ctrl Pts',(7.27603390513785,-81.2795179709984,4.20082013374672));
#18823=CARTESIAN_POINT('Ctrl Pts',(9.70137854017372,-81.1045179709984,-1.74689612655491E-11));
#18824=CARTESIAN_POINT('Ctrl Pts',(7.27603390512273,-80.9295179709984,-4.20082013377291));
#18825=CARTESIAN_POINT('Ctrl Pts',(4.85068927007173,-80.7545179709984,-8.40164026752836));
#18826=CARTESIAN_POINT('Ctrl Pts',(-1.51301075899711E-11,-80.5795179709984,
-8.40164026751963));
#18827=CARTESIAN_POINT('Ctrl Pts',(-4.85068927010199,-80.4045179709985,
-8.4016402675109));
#18828=CARTESIAN_POINT('Ctrl Pts',(-7.27603390513785,-80.2295179709984,
-4.20082013374671));
#18829=CARTESIAN_POINT('Ctrl Pts',(-9.70137854017372,-80.0545179709984,
1.74701493417668E-11));
#18830=CARTESIAN_POINT('Ctrl Pts',(-7.27603390512272,-79.8795179709984,
4.20082013377292));
#18831=CARTESIAN_POINT('Ctrl Pts',(-4.85068927007173,-79.7045179709984,
8.40164026752836));
#18832=CARTESIAN_POINT('Ctrl Pts',(1.5129078685785E-11,-79.5295179709984,
8.40164026751963));
#18833=CARTESIAN_POINT('Ctrl Pts',(4.85068927010198,-79.3545179709984,8.4016402675109));
#18834=CARTESIAN_POINT('Ctrl Pts',(7.27603390513785,-79.1795179709984,4.20082013374672));
#18835=CARTESIAN_POINT('Ctrl Pts',(9.70137854017372,-79.0045179709984,-1.74689612655491E-11));
#18836=CARTESIAN_POINT('Ctrl Pts',(7.27603390512273,-78.8295179709984,-4.20082013377291));
#18837=CARTESIAN_POINT('Ctrl Pts',(4.85068927007173,-78.6545179709984,-8.40164026752836));
#18838=CARTESIAN_POINT('Ctrl Pts',(-1.51301075899711E-11,-78.4795179709984,
-8.40164026751963));
#18839=CARTESIAN_POINT('Ctrl Pts',(-4.85068927010199,-78.3045179709985,
-8.4016402675109));
#18840=CARTESIAN_POINT('Ctrl Pts',(-7.27603390513785,-78.1295179709984,
-4.20082013374671));
#18841=CARTESIAN_POINT('Ctrl Pts',(-9.70137854017372,-77.9545179709984,
1.74701493417668E-11));
#18842=CARTESIAN_POINT('Ctrl Pts',(-7.27603390512272,-77.7795179709984,
4.20082013377292));
#18843=CARTESIAN_POINT('Ctrl Pts',(-4.85068927007173,-77.6045179709984,
8.40164026752836));
#18844=CARTESIAN_POINT('Ctrl Pts',(1.5129078685785E-11,-77.4295179709984,
8.40164026751963));
#18845=CARTESIAN_POINT('Ctrl Pts',(4.85068927010198,-77.2545179709984,8.4016402675109));
#18846=CARTESIAN_POINT('Ctrl Pts',(7.27603390513785,-77.0795179709984,4.20082013374672));
#18847=CARTESIAN_POINT('Ctrl Pts',(9.70137854017372,-76.9045179709984,-1.74689612655491E-11));
#18848=CARTESIAN_POINT('Ctrl Pts',(7.27603390512273,-76.7295179709984,-4.20082013377291));
#18849=CARTESIAN_POINT('Ctrl Pts',(4.85068927007173,-76.5545179709984,-8.40164026752836));
#18850=CARTESIAN_POINT('Ctrl Pts',(-1.51301075899711E-11,-76.3795179709984,
-8.40164026751963));
#18851=CARTESIAN_POINT('Ctrl Pts',(-4.85068927010199,-76.2045179709985,
-8.4016402675109));
#18852=CARTESIAN_POINT('Ctrl Pts',(-7.27603390513785,-76.0295179709984,
-4.20082013374671));
#18853=CARTESIAN_POINT('Ctrl Pts',(-9.70137854017372,-75.8545179709985,
1.74701493417668E-11));
#18854=CARTESIAN_POINT('Ctrl Pts',(-7.27603390512272,-75.6795179709984,
4.20082013377292));
#18855=CARTESIAN_POINT('Ctrl Pts',(-4.85068927007173,-75.5045179709984,
8.40164026752836));
#18856=CARTESIAN_POINT('Ctrl Pts',(1.5129078685785E-11,-75.3295179709984,
8.40164026751963));
#18857=CARTESIAN_POINT('Ctrl Pts',(4.85068927010198,-75.1545179709984,8.4016402675109));
#18858=CARTESIAN_POINT('Ctrl Pts',(7.27603390513785,-74.9795179709984,4.20082013374672));
#18859=CARTESIAN_POINT('Ctrl Pts',(9.70137854017372,-74.8045179709984,-1.74689612655491E-11));
#18860=CARTESIAN_POINT('Ctrl Pts',(7.27603390512273,-74.6295179709984,-4.20082013377291));
#18861=CARTESIAN_POINT('Ctrl Pts',(4.85068927007173,-74.4545179709984,-8.40164026752836));
#18862=CARTESIAN_POINT('Ctrl Pts',(-1.51301075899711E-11,-74.2795179709984,
-8.40164026751963));
#18863=CARTESIAN_POINT('Ctrl Pts',(-4.85068927010199,-74.1045179709984,
-8.4016402675109));
#18864=CARTESIAN_POINT('Ctrl Pts',(-7.27603390513785,-73.9295179709984,
-4.20082013374671));
#18865=CARTESIAN_POINT('Ctrl Pts',(-9.70137854017372,-73.7545179709984,
1.74701493417668E-11));
#18866=CARTESIAN_POINT('Ctrl Pts',(-7.27603390512272,-73.5795179709984,
4.20082013377292));
#18867=CARTESIAN_POINT('Ctrl Pts',(-4.85068927007173,-73.4045179709984,
8.40164026752836));
#18868=CARTESIAN_POINT('Ctrl Pts',(1.5129078685785E-11,-73.2295179709984,
8.40164026751963));
#18869=CARTESIAN_POINT('Ctrl Pts',(4.85068927010198,-73.0545179709984,8.4016402675109));
#18870=CARTESIAN_POINT('Ctrl Pts',(7.27603390513785,-72.8795179709984,4.20082013374672));
#18871=CARTESIAN_POINT('Ctrl Pts',(9.70137854017372,-72.7045179709984,-1.74689612655491E-11));
#18872=CARTESIAN_POINT('Ctrl Pts',(7.27603390512273,-72.5295179709984,-4.20082013377291));
#18873=CARTESIAN_POINT('Ctrl Pts',(4.85068927007173,-72.3545179709984,-8.40164026752836));
#18874=CARTESIAN_POINT('Ctrl Pts',(-1.51301075899711E-11,-72.1795179709984,
-8.40164026751963));
#18875=CARTESIAN_POINT('Ctrl Pts',(-4.85068927010199,-72.0045179709984,
-8.4016402675109));
#18876=CARTESIAN_POINT('Ctrl Pts',(-7.27603390513785,-71.8295179709984,
-4.20082013374671));
#18877=CARTESIAN_POINT('Ctrl Pts',(-9.70137854017372,-71.6545179709985,
1.74701493417668E-11));
#18878=CARTESIAN_POINT('Ctrl Pts',(-7.27603390512272,-71.4795179709984,
4.20082013377292));
#18879=CARTESIAN_POINT('Ctrl Pts',(-4.85068927007173,-71.3045179709984,
8.40164026752836));
#18880=CARTESIAN_POINT('Ctrl Pts',(1.5129078685785E-11,-71.1295179709984,
8.40164026751963));
#18881=CARTESIAN_POINT('Ctrl Pts',(4.85068927010198,-70.9545179709984,8.4016402675109));
#18882=CARTESIAN_POINT('Ctrl Pts',(7.27603390513785,-70.7795179709984,4.20082013374672));
#18883=CARTESIAN_POINT('Ctrl Pts',(9.70137854017372,-70.6045179709985,-1.74689612655491E-11));
#18884=CARTESIAN_POINT('Ctrl Pts',(7.27603390512273,-70.4295179709984,-4.20082013377291));
#18885=CARTESIAN_POINT('Ctrl Pts',(4.85068927007173,-70.2545179709984,-8.40164026752836));
#18886=CARTESIAN_POINT('Ctrl Pts',(-1.51301075899711E-11,-70.0795179709985,
-8.40164026751963));
#18887=CARTESIAN_POINT('Ctrl Pts',(-4.85068927010199,-69.9045179709984,
-8.4016402675109));
#18888=CARTESIAN_POINT('Ctrl Pts',(-7.27603390513785,-69.7295179709984,
-4.20082013374671));
#18889=CARTESIAN_POINT('Ctrl Pts',(-9.70137854017372,-69.5545179709985,
1.74701493417668E-11));
#18890=CARTESIAN_POINT('Ctrl Pts',(-7.27603390512272,-69.3795179709984,
4.20082013377292));
#18891=CARTESIAN_POINT('Ctrl Pts',(-4.85068927007173,-69.2045179709985,
8.40164026752836));
#18892=CARTESIAN_POINT('Ctrl Pts',(1.5129078685785E-11,-69.0295179709985,
8.40164026751963));
#18893=CARTESIAN_POINT('Ctrl Pts',(4.85068927010198,-68.8545179709984,8.4016402675109));
#18894=CARTESIAN_POINT('Ctrl Pts',(7.27603390513785,-68.6795179709985,4.20082013374672));
#18895=CARTESIAN_POINT('Ctrl Pts',(9.70137854017372,-68.5045179709985,-1.74689612655491E-11));
#18896=CARTESIAN_POINT('Ctrl Pts',(7.27603390512273,-68.3295179709984,-4.20082013377291));
#18897=CARTESIAN_POINT('Ctrl Pts',(4.85068927007173,-68.1545179709985,-8.40164026752836));
#18898=CARTESIAN_POINT('Ctrl Pts',(-1.51301075899711E-11,-67.9795179709985,
-8.40164026751963));
#18899=CARTESIAN_POINT('Ctrl Pts',(-4.85068927010199,-67.8045179709984,
-8.4016402675109));
#18900=CARTESIAN_POINT('Ctrl Pts',(-7.27603390513785,-67.6295179709984,
-4.20082013374671));
#18901=CARTESIAN_POINT('Ctrl Pts',(-9.70137854017372,-67.4545179709985,
1.74701493417668E-11));
#18902=CARTESIAN_POINT('Ctrl Pts',(-7.27603390512272,-67.2795179709984,
4.20082013377292));
#18903=CARTESIAN_POINT('Ctrl Pts',(-4.85068927007173,-67.1045179709985,
8.40164026752836));
#18904=CARTESIAN_POINT('Ctrl Pts',(1.5129078685785E-11,-66.9295179709985,
8.40164026751963));
#18905=CARTESIAN_POINT('Ctrl Pts',(4.85068927010198,-66.7545179709984,8.4016402675109));
#18906=CARTESIAN_POINT('Ctrl Pts',(7.27603390513785,-66.5795179709985,4.20082013374672));
#18907=CARTESIAN_POINT('Ctrl Pts',(9.70137854017372,-66.4045179709985,-1.74689612655491E-11));
#18908=CARTESIAN_POINT('Ctrl Pts',(7.27603390512273,-66.2295179709984,-4.20082013377291));
#18909=CARTESIAN_POINT('Ctrl Pts',(4.85068927007173,-66.0545179709985,-8.40164026752836));
#18910=CARTESIAN_POINT('Ctrl Pts',(-1.51301075899711E-11,-65.8795179709984,
-8.40164026751963));
#18911=CARTESIAN_POINT('Ctrl Pts',(-4.85068927010199,-65.7045179709985,
-8.4016402675109));
#18912=CARTESIAN_POINT('Ctrl Pts',(-7.27603390513785,-65.5295179709985,
-4.20082013374671));
#18913=CARTESIAN_POINT('Ctrl Pts',(-9.70137854017372,-65.3545179709984,
1.74701493417668E-11));
#18914=CARTESIAN_POINT('Ctrl Pts',(-7.27603390512272,-65.1795179709984,
4.20082013377292));
#18915=CARTESIAN_POINT('Ctrl Pts',(-4.85068927007173,-65.0045179709985,
8.40164026752836));
#18916=CARTESIAN_POINT('Ctrl Pts',(1.5129078685785E-11,-64.8295179709985,
8.40164026751963));
#18917=CARTESIAN_POINT('Ctrl Pts',(4.85068927010198,-64.6545179709985,8.4016402675109));
#18918=CARTESIAN_POINT('Ctrl Pts',(7.27603390513785,-64.4795179709985,4.20082013374672));
#18919=CARTESIAN_POINT('Ctrl Pts',(9.70137854017372,-64.3045179709985,-1.74689612655491E-11));
#18920=CARTESIAN_POINT('Ctrl Pts',(7.27603390512273,-64.1295179709984,-4.20082013377291));
#18921=CARTESIAN_POINT('Ctrl Pts',(4.85068927007173,-63.9545179709985,-8.40164026752836));
#18922=CARTESIAN_POINT('Ctrl Pts',(-1.51301075899711E-11,-63.7795179709985,
-8.40164026751963));
#18923=CARTESIAN_POINT('Ctrl Pts',(-4.85068927010199,-63.6045179709985,
-8.4016402675109));
#18924=CARTESIAN_POINT('Ctrl Pts',(-7.27603390513785,-63.4295179709985,
-4.20082013374671));
#18925=CARTESIAN_POINT('Ctrl Pts',(-9.70137854017372,-63.2545179709985,
1.74701493417668E-11));
#18926=CARTESIAN_POINT('Ctrl Pts',(-7.27603390512272,-63.0795179709985,
4.20082013377292));
#18927=CARTESIAN_POINT('Ctrl Pts',(-4.85068927007173,-62.9045179709985,
8.40164026752836));
#18928=CARTESIAN_POINT('Ctrl Pts',(1.5129078685785E-11,-62.7295179709985,
8.40164026751963));
#18929=CARTESIAN_POINT('Ctrl Pts',(4.85068927010198,-62.5545179709985,8.4016402675109));
#18930=CARTESIAN_POINT('Ctrl Pts',(7.27603390513785,-62.3795179709985,4.20082013374672));
#18931=CARTESIAN_POINT('Ctrl Pts',(9.70137854017372,-62.2045179709985,-1.74689612655491E-11));
#18932=CARTESIAN_POINT('Ctrl Pts',(7.27603390512273,-62.0295179709985,-4.20082013377291));
#18933=CARTESIAN_POINT('Ctrl Pts',(4.85068927007173,-61.8545179709985,-8.40164026752836));
#18934=CARTESIAN_POINT('Ctrl Pts',(-1.51301075899711E-11,-61.6795179709985,
-8.40164026751963));
#18935=CARTESIAN_POINT('Ctrl Pts',(-4.85068927010199,-61.5045179709985,
-8.4016402675109));
#18936=CARTESIAN_POINT('Ctrl Pts',(-7.27603390513785,-61.3295179709985,
-4.20082013374671));
#18937=CARTESIAN_POINT('Ctrl Pts',(-9.70137854017372,-61.1545179709985,
1.74701493417668E-11));
#18938=CARTESIAN_POINT('Ctrl Pts',(-7.27603390512272,-60.9795179709985,
4.20082013377292));
#18939=CARTESIAN_POINT('Ctrl Pts',(-4.85068927007173,-60.8045179709985,
8.40164026752836));
#18940=CARTESIAN_POINT('Ctrl Pts',(1.5129078685785E-11,-60.6295179709985,
8.40164026751963));
#18941=CARTESIAN_POINT('Ctrl Pts',(4.85068927010198,-60.4545179709985,8.4016402675109));
#18942=CARTESIAN_POINT('Ctrl Pts',(7.27603390513785,-60.2795179709985,4.20082013374672));
#18943=CARTESIAN_POINT('Ctrl Pts',(9.70137854017372,-60.1045179709985,-1.74689612655491E-11));
#18944=CARTESIAN_POINT('Ctrl Pts',(7.27603390512273,-59.9295179709985,-4.20082013377291));
#18945=CARTESIAN_POINT('Ctrl Pts',(4.85068927007173,-59.7545179709985,-8.40164026752836));
#18946=CARTESIAN_POINT('Ctrl Pts',(-1.51301075899711E-11,-59.5795179709985,
-8.40164026751963));
#18947=CARTESIAN_POINT('Ctrl Pts',(-4.85068927010199,-59.4045179709985,
-8.4016402675109));
#18948=CARTESIAN_POINT('Ctrl Pts',(-7.27603390513785,-59.2295179709985,
-4.20082013374671));
#18949=CARTESIAN_POINT('Ctrl Pts',(-9.70137854017372,-59.0545179709985,
1.74701493417668E-11));
#18950=CARTESIAN_POINT('Ctrl Pts',(-7.27603390512272,-58.8795179709985,
4.20082013377292));
#18951=CARTESIAN_POINT('Ctrl Pts',(-4.85068927007173,-58.7045179709985,
8.40164026752836));
#18952=CARTESIAN_POINT('Ctrl Pts',(1.5129078685785E-11,-58.5295179709984,
8.40164026751963));
#18953=CARTESIAN_POINT('Ctrl Pts',(4.85068927010198,-58.3545179709985,8.4016402675109));
#18954=CARTESIAN_POINT('Ctrl Pts',(7.27603390513785,-58.1795179709985,4.20082013374672));
#18955=CARTESIAN_POINT('Ctrl Pts',(9.70137854017372,-58.0045179709985,-1.74689612655491E-11));
#18956=CARTESIAN_POINT('Ctrl Pts',(7.27603390512273,-57.8295179709985,-4.20082013377291));
#18957=CARTESIAN_POINT('Ctrl Pts',(4.85068927007173,-57.6545179709985,-8.40164026752836));
#18958=CARTESIAN_POINT('Ctrl Pts',(-1.51301075899711E-11,-57.4795179709985,
-8.40164026751963));
#18959=CARTESIAN_POINT('Ctrl Pts',(-4.85068927010199,-57.3045179709985,
-8.4016402675109));
#18960=CARTESIAN_POINT('Ctrl Pts',(-7.27603390513785,-57.1295179709985,
-4.20082013374671));
#18961=CARTESIAN_POINT('Ctrl Pts',(-9.70137854017372,-56.9545179709985,
1.74701493417668E-11));
#18962=CARTESIAN_POINT('Ctrl Pts',(-7.27603390512272,-56.7795179709985,
4.20082013377292));
#18963=CARTESIAN_POINT('Ctrl Pts',(-4.85068927007173,-56.6045179709985,
8.40164026752836));
#18964=CARTESIAN_POINT('Ctrl Pts',(1.5129078685785E-11,-56.4295179709985,
8.40164026751963));
#18965=CARTESIAN_POINT('Ctrl Pts',(4.85068927010198,-56.2545179709985,8.4016402675109));
#18966=CARTESIAN_POINT('Ctrl Pts',(7.27603390513785,-56.0795179709985,4.20082013374672));
#18967=CARTESIAN_POINT('Ctrl Pts',(9.70137854017372,-55.9045179709985,-1.74689612655491E-11));
#18968=CARTESIAN_POINT('Ctrl Pts',(7.27603390512273,-55.7295179709985,-4.20082013377291));
#18969=CARTESIAN_POINT('Ctrl Pts',(4.85068927007173,-55.5545179709985,-8.40164026752836));
#18970=CARTESIAN_POINT('Ctrl Pts',(-1.51301075899711E-11,-55.3795179709985,
-8.40164026751963));
#18971=CARTESIAN_POINT('Ctrl Pts',(-4.85068927010199,-55.2045179709985,
-8.4016402675109));
#18972=CARTESIAN_POINT('Ctrl Pts',(-7.27603390513785,-55.0295179709985,
-4.20082013374671));
#18973=CARTESIAN_POINT('Ctrl Pts',(-9.70137854017372,-54.8545179709985,
1.74701493417668E-11));
#18974=CARTESIAN_POINT('Ctrl Pts',(-7.27603390512272,-54.6795179709985,
4.20082013377292));
#18975=CARTESIAN_POINT('Ctrl Pts',(-4.85068927007173,-54.5045179709985,
8.40164026752836));
#18976=CARTESIAN_POINT('Ctrl Pts',(1.5129078685785E-11,-54.3295179709985,
8.40164026751963));
#18977=CARTESIAN_POINT('Ctrl Pts',(4.85068927010198,-54.1545179709985,8.4016402675109));
#18978=CARTESIAN_POINT('Ctrl Pts',(7.27603390513785,-53.9795179709985,4.20082013374672));
#18979=CARTESIAN_POINT('Ctrl Pts',(9.70137854017372,-53.8045179709985,-1.74689612655491E-11));
#18980=CARTESIAN_POINT('Ctrl Pts',(7.27603390512273,-53.6295179709985,-4.20082013377291));
#18981=CARTESIAN_POINT('Ctrl Pts',(4.85068927007173,-53.4545179709985,-8.40164026752836));
#18982=CARTESIAN_POINT('Ctrl Pts',(-1.51301075899711E-11,-53.2795179709985,
-8.40164026751963));
#18983=CARTESIAN_POINT('Ctrl Pts',(-4.85068927010199,-53.1045179709985,
-8.4016402675109));
#18984=CARTESIAN_POINT('Ctrl Pts',(-7.27603390513785,-52.9295179709985,
-4.20082013374671));
#18985=CARTESIAN_POINT('Ctrl Pts',(-9.70137854017372,-52.7545179709985,
1.74701493417668E-11));
#18986=CARTESIAN_POINT('Ctrl Pts',(-7.27603390512272,-52.5795179709985,
4.20082013377292));
#18987=CARTESIAN_POINT('Ctrl Pts',(-4.85068927007173,-52.4045179709985,
8.40164026752836));
#18988=CARTESIAN_POINT('Ctrl Pts',(1.5129078685785E-11,-52.2295179709985,
8.40164026751963));
#18989=CARTESIAN_POINT('Ctrl Pts',(4.85068927010198,-52.0545179709985,8.4016402675109));
#18990=CARTESIAN_POINT('Ctrl Pts',(7.27603390513785,-51.8795179709985,4.20082013374672));
#18991=CARTESIAN_POINT('Ctrl Pts',(9.70137854017372,-51.7045179709985,-1.74689612655491E-11));
#18992=CARTESIAN_POINT('Ctrl Pts',(7.27603390512273,-51.5295179709985,-4.20082013377291));
#18993=CARTESIAN_POINT('Ctrl Pts',(4.85068927007173,-51.3545179709985,-8.40164026752836));
#18994=CARTESIAN_POINT('Ctrl Pts',(-1.51301075899711E-11,-51.1795179709985,
-8.40164026751963));
#18995=CARTESIAN_POINT('Ctrl Pts',(-4.85068927010199,-51.0045179709985,
-8.4016402675109));
#18996=CARTESIAN_POINT('Ctrl Pts',(-7.27603390513785,-50.8295179709985,
-4.20082013374671));
#18997=CARTESIAN_POINT('Ctrl Pts',(-9.70137854017372,-50.6545179709985,
1.74701493417668E-11));
#18998=CARTESIAN_POINT('Ctrl Pts',(-7.27603390512272,-50.4795179709985,
4.20082013377292));
#18999=CARTESIAN_POINT('Ctrl Pts',(-4.85068927007173,-50.3045179709985,
8.40164026752836));
#19000=CARTESIAN_POINT('Ctrl Pts',(1.5129078685785E-11,-50.1295179709985,
8.40164026751963));
#19001=CARTESIAN_POINT('Ctrl Pts',(4.85068927010198,-49.9545179709985,8.4016402675109));
#19002=CARTESIAN_POINT('Ctrl Pts',(7.27603390513785,-49.7795179709985,4.20082013374672));
#19003=CARTESIAN_POINT('Ctrl Pts',(9.70137854017372,-49.6045179709985,-1.74689612655491E-11));
#19004=CARTESIAN_POINT('Ctrl Pts',(7.27603390512273,-49.4295179709985,-4.20082013377291));
#19005=CARTESIAN_POINT('Ctrl Pts',(4.85068927007173,-49.2545179709985,-8.40164026752836));
#19006=CARTESIAN_POINT('Ctrl Pts',(-1.51301075899711E-11,-49.0795179709985,
-8.40164026751963));
#19007=CARTESIAN_POINT('Ctrl Pts',(-4.85068927010199,-48.9045179709985,
-8.4016402675109));
#19008=CARTESIAN_POINT('Ctrl Pts',(-7.27603390513785,-48.7295179709985,
-4.20082013374671));
#19009=CARTESIAN_POINT('Ctrl Pts',(-9.70137854017372,-48.5545179709985,
1.74701493417668E-11));
#19010=CARTESIAN_POINT('Ctrl Pts',(-7.27603390512272,-48.3795179709985,
4.20082013377292));
#19011=CARTESIAN_POINT('Ctrl Pts',(-4.85068927007173,-48.2045179709985,
8.40164026752836));
#19012=CARTESIAN_POINT('Ctrl Pts',(1.5129078685785E-11,-48.0295179709985,
8.40164026751963));
#19013=CARTESIAN_POINT('Ctrl Pts',(4.85068927010198,-47.8545179709985,8.4016402675109));
#19014=CARTESIAN_POINT('Ctrl Pts',(7.27603390513785,-47.6795179709985,4.20082013374672));
#19015=CARTESIAN_POINT('Ctrl Pts',(9.70137854017372,-47.5045179709985,-1.74689612655491E-11));
#19016=CARTESIAN_POINT('Ctrl Pts',(7.27603390512273,-47.3295179709985,-4.20082013377291));
#19017=CARTESIAN_POINT('Ctrl Pts',(4.85068927007173,-47.1545179709985,-8.40164026752836));
#19018=CARTESIAN_POINT('Ctrl Pts',(-1.51301075899711E-11,-46.9795179709985,
-8.40164026751963));
#19019=CARTESIAN_POINT('Ctrl Pts',(-4.85068927010199,-46.8045179709985,
-8.4016402675109));
#19020=CARTESIAN_POINT('Ctrl Pts',(-7.27603390513785,-46.6295179709985,
-4.20082013374671));
#19021=CARTESIAN_POINT('Ctrl Pts',(-9.70137854017372,-46.4545179709985,
1.74701493417668E-11));
#19022=CARTESIAN_POINT('Ctrl Pts',(-7.27603390512272,-46.2795179709985,
4.20082013377292));
#19023=CARTESIAN_POINT('Ctrl Pts',(-4.85068927007173,-46.1045179709985,
8.40164026752836));
#19024=CARTESIAN_POINT('Ctrl Pts',(1.5129078685785E-11,-45.9295179709985,
8.40164026751963));
#19025=CARTESIAN_POINT('Ctrl Pts',(4.85068927010198,-45.7545179709985,8.4016402675109));
#19026=CARTESIAN_POINT('Ctrl Pts',(7.27603390513785,-45.5795179709985,4.20082013374672));
#19027=CARTESIAN_POINT('Ctrl Pts',(9.70137854017372,-45.4045179709985,-1.74689612655491E-11));
#19028=CARTESIAN_POINT('Ctrl Pts',(7.27603390512273,-45.2295179709985,-4.20082013377291));
#19029=CARTESIAN_POINT('Ctrl Pts',(4.85068927007173,-45.0545179709985,-8.40164026752836));
#19030=CARTESIAN_POINT('Ctrl Pts',(-1.51301075899711E-11,-44.8795179709985,
-8.40164026751963));
#19031=CARTESIAN_POINT('Ctrl Pts',(-4.85068927010199,-44.7045179709985,
-8.4016402675109));
#19032=CARTESIAN_POINT('Ctrl Pts',(-7.27603390513785,-44.5295179709985,
-4.20082013374671));
#19033=CARTESIAN_POINT('Ctrl Pts',(-9.70137854017372,-44.3545179709985,
1.74701493417668E-11));
#19034=CARTESIAN_POINT('Ctrl Pts',(-7.27603390512272,-44.1795179709985,
4.20082013377292));
#19035=CARTESIAN_POINT('Ctrl Pts',(-4.85068927007173,-44.0045179709985,
8.40164026752836));
#19036=CARTESIAN_POINT('Ctrl Pts',(1.5129078685785E-11,-43.8295179709985,
8.40164026751963));
#19037=CARTESIAN_POINT('Ctrl Pts',(4.85068927010198,-43.6545179709985,8.4016402675109));
#19038=CARTESIAN_POINT('Ctrl Pts',(7.27603390513785,-43.4795179709985,4.20082013374672));
#19039=CARTESIAN_POINT('Ctrl Pts',(9.70137854017372,-43.3045179709985,-1.74689612655491E-11));
#19040=CARTESIAN_POINT('Ctrl Pts',(7.27603390512273,-43.1295179709985,-4.20082013377291));
#19041=CARTESIAN_POINT('Ctrl Pts',(4.85068927007173,-42.9545179709985,-8.40164026752836));
#19042=CARTESIAN_POINT('Ctrl Pts',(-1.51301075899711E-11,-42.7795179709985,
-8.40164026751963));
#19043=CARTESIAN_POINT('Ctrl Pts',(-4.85068927010199,-42.6045179709985,
-8.4016402675109));
#19044=CARTESIAN_POINT('Ctrl Pts',(-7.27603390513785,-42.4295179709985,
-4.20082013374671));
#19045=CARTESIAN_POINT('Ctrl Pts',(-9.70137854017372,-42.2545179709985,
1.74701493417668E-11));
#19046=CARTESIAN_POINT('Ctrl Pts',(-7.27603390512272,-42.0795179709985,
4.20082013377292));
#19047=CARTESIAN_POINT('Ctrl Pts',(-4.85068927007173,-41.9045179709985,
8.40164026752836));
#19048=CARTESIAN_POINT('Ctrl Pts',(1.5129078685785E-11,-41.7295179709985,
8.40164026751963));
#19049=CARTESIAN_POINT('Ctrl Pts',(4.85068927010198,-41.5545179709985,8.4016402675109));
#19050=CARTESIAN_POINT('Ctrl Pts',(7.27603390513785,-41.3795179709985,4.20082013374672));
#19051=CARTESIAN_POINT('Ctrl Pts',(9.70137854017372,-41.2045179709985,-1.74689612655491E-11));
#19052=CARTESIAN_POINT('Ctrl Pts',(7.27603390512273,-41.0295179709985,-4.20082013377291));
#19053=CARTESIAN_POINT('Ctrl Pts',(4.85068927007173,-40.8545179709985,-8.40164026752836));
#19054=CARTESIAN_POINT('Ctrl Pts',(-1.51301075899711E-11,-40.6795179709985,
-8.40164026751963));
#19055=CARTESIAN_POINT('Ctrl Pts',(-4.85068927010199,-40.5045179709985,
-8.4016402675109));
#19056=CARTESIAN_POINT('Ctrl Pts',(-7.27603390513785,-40.3295179709985,
-4.20082013374671));
#19057=CARTESIAN_POINT('Ctrl Pts',(-9.70137854017372,-40.1545179709985,
1.74701493417668E-11));
#19058=CARTESIAN_POINT('Ctrl Pts',(-7.27603390512272,-39.9795179709985,
4.20082013377292));
#19059=CARTESIAN_POINT('Ctrl Pts',(-4.85068927007173,-39.8045179709985,
8.40164026752836));
#19060=CARTESIAN_POINT('Ctrl Pts',(1.5129078685785E-11,-39.6295179709985,
8.40164026751963));
#19061=CARTESIAN_POINT('Ctrl Pts',(4.85068927010198,-39.4545179709985,8.4016402675109));
#19062=CARTESIAN_POINT('Ctrl Pts',(7.27603390513785,-39.2795179709985,4.20082013374672));
#19063=CARTESIAN_POINT('Ctrl Pts',(9.70137854017372,-39.1045179709985,-1.74689612655491E-11));
#19064=CARTESIAN_POINT('Ctrl Pts',(7.27603390512273,-38.9295179709985,-4.20082013377291));
#19065=CARTESIAN_POINT('Ctrl Pts',(4.85068927007173,-38.7545179709985,-8.40164026752836));
#19066=CARTESIAN_POINT('Ctrl Pts',(-1.51301075899711E-11,-38.5795179709985,
-8.40164026751963));
#19067=CARTESIAN_POINT('Ctrl Pts',(-4.85068927010199,-38.4045179709985,
-8.4016402675109));
#19068=CARTESIAN_POINT('Ctrl Pts',(-7.27603390513785,-38.2295179709985,
-4.20082013374671));
#19069=CARTESIAN_POINT('Ctrl Pts',(-9.70137854017372,-38.0545179709985,
1.74701493417668E-11));
#19070=CARTESIAN_POINT('Ctrl Pts',(-7.27603390512272,-37.8795179709985,
4.20082013377292));
#19071=CARTESIAN_POINT('Ctrl Pts',(-4.85068927007173,-37.7045179709985,
8.40164026752836));
#19072=CARTESIAN_POINT('Ctrl Pts',(1.5129078685785E-11,-37.5295179709985,
8.40164026751963));
#19073=CARTESIAN_POINT('Ctrl Pts',(4.85068927010198,-37.3545179709985,8.4016402675109));
#19074=CARTESIAN_POINT('Ctrl Pts',(7.27603390513785,-37.1795179709985,4.20082013374672));
#19075=CARTESIAN_POINT('Ctrl Pts',(9.70137854017372,-37.0045179709985,-1.74689612655491E-11));
#19076=CARTESIAN_POINT('Ctrl Pts',(7.27603390512273,-36.8295179709985,-4.20082013377291));
#19077=CARTESIAN_POINT('Ctrl Pts',(4.85068927007173,-36.6545179709985,-8.40164026752836));
#19078=CARTESIAN_POINT('Ctrl Pts',(-1.51301075899711E-11,-36.4795179709985,
-8.40164026751963));
#19079=CARTESIAN_POINT('Ctrl Pts',(-4.85068927010199,-36.3045179709985,
-8.4016402675109));
#19080=CARTESIAN_POINT('Ctrl Pts',(-7.27603390513785,-36.1295179709985,
-4.20082013374671));
#19081=CARTESIAN_POINT('Ctrl Pts',(-9.70137854017372,-35.9545179709985,
1.74701493417668E-11));
#19082=CARTESIAN_POINT('Ctrl Pts',(-7.27603390512272,-35.7795179709985,
4.20082013377292));
#19083=CARTESIAN_POINT('Ctrl Pts',(-4.85068927007173,-35.6045179709985,
8.40164026752836));
#19084=CARTESIAN_POINT('Ctrl Pts',(1.5129078685785E-11,-35.4295179709985,
8.40164026751963));
#19085=CARTESIAN_POINT('Ctrl Pts',(4.85068927010198,-35.2545179709985,8.4016402675109));
#19086=CARTESIAN_POINT('Ctrl Pts',(7.27603390513785,-35.0795179709985,4.20082013374672));
#19087=CARTESIAN_POINT('Ctrl Pts',(9.70137854017372,-34.9045179709985,-1.74689612655491E-11));
#19088=CARTESIAN_POINT('Ctrl Pts',(7.27603390512273,-34.7295179709985,-4.20082013377291));
#19089=CARTESIAN_POINT('Ctrl Pts',(4.85068927007173,-34.5545179709985,-8.40164026752836));
#19090=CARTESIAN_POINT('Ctrl Pts',(-1.51301075899711E-11,-34.3795179709985,
-8.40164026751963));
#19091=CARTESIAN_POINT('Ctrl Pts',(-4.85068927010199,-34.2045179709985,
-8.4016402675109));
#19092=CARTESIAN_POINT('Ctrl Pts',(-7.27603390513785,-34.0295179709985,
-4.20082013374671));
#19093=CARTESIAN_POINT('Ctrl Pts',(-9.70137854017372,-33.8545179709985,
1.74701493417668E-11));
#19094=CARTESIAN_POINT('Ctrl Pts',(-7.27603390512272,-33.6795179709985,
4.20082013377292));
#19095=CARTESIAN_POINT('Ctrl Pts',(-4.85068927007173,-33.5045179709985,
8.40164026752836));
#19096=CARTESIAN_POINT('Ctrl Pts',(1.5129078685785E-11,-33.3295179709985,
8.40164026751963));
#19097=CARTESIAN_POINT('Ctrl Pts',(4.85068927010198,-33.1545179709985,8.4016402675109));
#19098=CARTESIAN_POINT('Ctrl Pts',(7.27603390513785,-32.9795179709985,4.20082013374672));
#19099=CARTESIAN_POINT('Ctrl Pts',(9.70137854017372,-32.8045179709985,-1.74689612655491E-11));
#19100=CARTESIAN_POINT('Ctrl Pts',(7.27603390512273,-32.6295179709985,-4.20082013377291));
#19101=CARTESIAN_POINT('Ctrl Pts',(4.85068927007173,-32.4545179709985,-8.40164026752836));
#19102=CARTESIAN_POINT('Ctrl Pts',(-1.51301075899711E-11,-32.2795179709985,
-8.40164026751963));
#19103=CARTESIAN_POINT('Ctrl Pts',(-4.85068927010199,-32.1045179709985,
-8.4016402675109));
#19104=CARTESIAN_POINT('Ctrl Pts',(-7.27603390513785,-31.9295179709985,
-4.20082013374671));
#19105=CARTESIAN_POINT('Ctrl Pts',(-9.70137854017372,-31.7545179709985,
1.74701493417668E-11));
#19106=CARTESIAN_POINT('Ctrl Pts',(-7.27603390512272,-31.5795179709985,
4.20082013377292));
#19107=CARTESIAN_POINT('Ctrl Pts',(-4.85068927007173,-31.4045179709985,
8.40164026752836));
#19108=CARTESIAN_POINT('Ctrl Pts',(1.5129078685785E-11,-31.2295179709985,
8.40164026751963));
#19109=CARTESIAN_POINT('Ctrl Pts',(4.85068927010198,-31.0545179709985,8.4016402675109));
#19110=CARTESIAN_POINT('Ctrl Pts',(7.27603390513785,-30.8795179709985,4.20082013374672));
#19111=CARTESIAN_POINT('Ctrl Pts',(9.70137854017372,-30.7045179709985,-1.74689612655491E-11));
#19112=CARTESIAN_POINT('Ctrl Pts',(7.27603390512273,-30.5295179709985,-4.20082013377291));
#19113=CARTESIAN_POINT('Ctrl Pts',(4.85068927007173,-30.3545179709985,-8.40164026752836));
#19114=CARTESIAN_POINT('Ctrl Pts',(-1.51301075899711E-11,-30.1795179709985,
-8.40164026751963));
#19115=CARTESIAN_POINT('Ctrl Pts',(-4.85068927010199,-30.0045179709985,
-8.4016402675109));
#19116=CARTESIAN_POINT('Ctrl Pts',(-7.27603390513785,-29.8295179709985,
-4.20082013374671));
#19117=CARTESIAN_POINT('Ctrl Pts',(-9.70137854017372,-29.6545179709985,
1.74701493417668E-11));
#19118=CARTESIAN_POINT('Ctrl Pts',(-7.27603390512272,-29.4795179709985,
4.20082013377292));
#19119=CARTESIAN_POINT('Ctrl Pts',(-4.85068927007173,-29.3045179709985,
8.40164026752836));
#19120=CARTESIAN_POINT('Ctrl Pts',(1.5129078685785E-11,-29.1295179709985,
8.40164026751963));
#19121=CARTESIAN_POINT('Ctrl Pts',(4.85068927010198,-28.9545179709986,8.4016402675109));
#19122=CARTESIAN_POINT('Ctrl Pts',(7.27603390513785,-28.7795179709985,4.20082013374672));
#19123=CARTESIAN_POINT('Ctrl Pts',(9.70137854017372,-28.6045179709986,-1.74689612655491E-11));
#19124=CARTESIAN_POINT('Ctrl Pts',(7.27603390512273,-28.4295179709985,-4.20082013377291));
#19125=CARTESIAN_POINT('Ctrl Pts',(4.85068927007173,-28.2545179709985,-8.40164026752836));
#19126=CARTESIAN_POINT('Ctrl Pts',(-1.51301075899711E-11,-28.0795179709985,
-8.40164026751963));
#19127=CARTESIAN_POINT('Ctrl Pts',(-4.85068927010199,-27.9045179709985,
-8.4016402675109));
#19128=CARTESIAN_POINT('Ctrl Pts',(-7.27603390513785,-27.7295179709985,
-4.20082013374671));
#19129=CARTESIAN_POINT('Ctrl Pts',(-9.70137854017372,-27.5545179709986,
1.74701493417668E-11));
#19130=CARTESIAN_POINT('Ctrl Pts',(-7.27603390512272,-27.3795179709985,
4.20082013377292));
#19131=CARTESIAN_POINT('Ctrl Pts',(-4.85068927007173,-27.2045179709986,
8.40164026752836));
#19132=CARTESIAN_POINT('Ctrl Pts',(1.5129078685785E-11,-27.0295179709986,
8.40164026751963));
#19133=CARTESIAN_POINT('Ctrl Pts',(4.85068927010198,-26.8545179709985,8.4016402675109));
#19134=CARTESIAN_POINT('Ctrl Pts',(7.27603390513785,-26.6795179709985,4.20082013374672));
#19135=CARTESIAN_POINT('Ctrl Pts',(9.70137854017372,-26.5045179709986,-1.74689612655491E-11));
#19136=CARTESIAN_POINT('Ctrl Pts',(7.27603390512273,-26.3295179709985,-4.20082013377291));
#19137=CARTESIAN_POINT('Ctrl Pts',(4.85068927007173,-26.1545179709986,-8.40164026752836));
#19138=CARTESIAN_POINT('Ctrl Pts',(-1.51301075899711E-11,-25.9795179709985,
-8.40164026751963));
#19139=CARTESIAN_POINT('Ctrl Pts',(-4.85068927010199,-25.8045179709985,
-8.4016402675109));
#19140=CARTESIAN_POINT('Ctrl Pts',(-7.27603390513785,-25.6295179709985,
-4.20082013374671));
#19141=CARTESIAN_POINT('Ctrl Pts',(-9.70137854017372,-25.4545179709985,
1.74701493417668E-11));
#19142=CARTESIAN_POINT('Ctrl Pts',(-7.27603390512272,-25.2795179709985,
4.20082013377292));
#19143=CARTESIAN_POINT('Ctrl Pts',(-4.85068927007173,-25.1045179709986,
8.40164026752836));
#19144=CARTESIAN_POINT('Ctrl Pts',(1.5129078685785E-11,-24.9295179709985,
8.40164026751963));
#19145=CARTESIAN_POINT('Ctrl Pts',(4.85068927010198,-24.7545179709985,8.4016402675109));
#19146=CARTESIAN_POINT('Ctrl Pts',(7.27603390513785,-24.5795179709986,4.20082013374672));
#19147=CARTESIAN_POINT('Ctrl Pts',(9.70137854017372,-24.4045179709986,-1.74689612655491E-11));
#19148=CARTESIAN_POINT('Ctrl Pts',(7.27603390512273,-24.2295179709986,-4.20082013377291));
#19149=CARTESIAN_POINT('Ctrl Pts',(4.85068927007173,-24.0545179709986,-8.40164026752836));
#19150=CARTESIAN_POINT('Ctrl Pts',(-1.51301075899711E-11,-23.8795179709986,
-8.40164026751963));
#19151=CARTESIAN_POINT('Ctrl Pts',(-4.85068927010199,-23.7045179709986,
-8.4016402675109));
#19152=CARTESIAN_POINT('Ctrl Pts',(-7.27603390513785,-23.5295179709985,
-4.20082013374671));
#19153=CARTESIAN_POINT('Ctrl Pts',(-9.70137854017372,-23.3545179709986,
1.74701493417668E-11));
#19154=CARTESIAN_POINT('Ctrl Pts',(-7.27603390512272,-23.1795179709986,
4.20082013377292));
#19155=CARTESIAN_POINT('Ctrl Pts',(-4.85068927007173,-23.0045179709986,
8.40164026752836));
#19156=CARTESIAN_POINT('Ctrl Pts',(1.5129078685785E-11,-22.8295179709986,
8.40164026751963));
#19157=CARTESIAN_POINT('Ctrl Pts',(4.85068927010198,-22.6545179709986,8.4016402675109));
#19158=CARTESIAN_POINT('Ctrl Pts',(7.27603390513785,-22.4795179709986,4.20082013374672));
#19159=CARTESIAN_POINT('Ctrl Pts',(9.70137854017372,-22.3045179709986,-1.74689612655491E-11));
#19160=CARTESIAN_POINT('Ctrl Pts',(7.27603390512273,-22.1295179709986,-4.20082013377291));
#19161=CARTESIAN_POINT('Ctrl Pts',(4.85068927007173,-21.9545179709986,-8.40164026752836));
#19162=CARTESIAN_POINT('Ctrl Pts',(-1.51301075899711E-11,-21.7795179709986,
-8.40164026751963));
#19163=CARTESIAN_POINT('Ctrl Pts',(-4.85068927010199,-21.6045179709986,
-8.4016402675109));
#19164=CARTESIAN_POINT('Ctrl Pts',(-7.27603390513785,-21.4295179709986,
-4.20082013374671));
#19165=CARTESIAN_POINT('Ctrl Pts',(-9.70137854017372,-21.2545179709986,
1.74701493417668E-11));
#19166=CARTESIAN_POINT('Ctrl Pts',(-7.27603390512272,-21.0795179709986,
4.20082013377292));
#19167=CARTESIAN_POINT('Ctrl Pts',(-4.85068927007173,-20.9045179709986,
8.40164026752836));
#19168=CARTESIAN_POINT('Ctrl Pts',(1.5129078685785E-11,-20.7295179709986,
8.40164026751963));
#19169=CARTESIAN_POINT('Ctrl Pts',(4.85068927010198,-20.5545179709986,8.4016402675109));
#19170=CARTESIAN_POINT('Ctrl Pts',(7.27603390513785,-20.3795179709986,4.20082013374672));
#19171=CARTESIAN_POINT('Ctrl Pts',(9.70137854017372,-20.2045179709986,-1.74689612655491E-11));
#19172=CARTESIAN_POINT('Ctrl Pts',(7.27603390512273,-20.0295179709986,-4.20082013377291));
#19173=CARTESIAN_POINT('Ctrl Pts',(4.85068927007173,-19.8545179709986,-8.40164026752836));
#19174=CARTESIAN_POINT('Ctrl Pts',(-1.51301075899711E-11,-19.6795179709986,
-8.40164026751963));
#19175=CARTESIAN_POINT('Ctrl Pts',(-4.85068927010199,-19.5045179709986,
-8.4016402675109));
#19176=CARTESIAN_POINT('Ctrl Pts',(-7.27603390513785,-19.3295179709986,
-4.20082013374671));
#19177=CARTESIAN_POINT('Ctrl Pts',(-9.70137854017372,-19.1545179709986,
1.74701493417668E-11));
#19178=CARTESIAN_POINT('Ctrl Pts',(-7.27603390512272,-18.9795179709986,
4.20082013377292));
#19179=CARTESIAN_POINT('Ctrl Pts',(-4.85068927007173,-18.8045179709986,
8.40164026752836));
#19180=CARTESIAN_POINT('Ctrl Pts',(1.5129078685785E-11,-18.6295179709986,
8.40164026751963));
#19181=CARTESIAN_POINT('Ctrl Pts',(4.85068927010198,-18.4545179709986,8.4016402675109));
#19182=CARTESIAN_POINT('Ctrl Pts',(7.27603390513785,-18.2795179709986,4.20082013374672));
#19183=CARTESIAN_POINT('Ctrl Pts',(9.70137854017372,-18.1045179709986,-1.74689612655491E-11));
#19184=CARTESIAN_POINT('Ctrl Pts',(7.27603390512273,-17.9295179709986,-4.20082013377291));
#19185=CARTESIAN_POINT('Ctrl Pts',(4.85068927007173,-17.7545179709986,-8.40164026752836));
#19186=CARTESIAN_POINT('Ctrl Pts',(-1.51301075899711E-11,-17.5795179709986,
-8.40164026751963));
#19187=CARTESIAN_POINT('Ctrl Pts',(-4.85068927010199,-17.4045179709986,
-8.4016402675109));
#19188=CARTESIAN_POINT('Ctrl Pts',(-7.27603390513785,-17.2295179709986,
-4.20082013374671));
#19189=CARTESIAN_POINT('Ctrl Pts',(-9.70137854017372,-17.0545179709986,
1.74701493417668E-11));
#19190=CARTESIAN_POINT('Ctrl Pts',(-7.27603390512272,-16.8795179709986,
4.20082013377292));
#19191=CARTESIAN_POINT('Ctrl Pts',(-4.85068927007173,-16.7045179709986,
8.40164026752836));
#19192=CARTESIAN_POINT('Ctrl Pts',(1.5129078685785E-11,-16.5295179709986,
8.40164026751963));
#19193=CARTESIAN_POINT('Ctrl Pts',(4.85068927010198,-16.3545179709986,8.4016402675109));
#19194=CARTESIAN_POINT('Ctrl Pts',(7.27603390513785,-16.1795179709986,4.20082013374672));
#19195=CARTESIAN_POINT('Ctrl Pts',(9.70137854017372,-16.0045179709986,-1.74689612655491E-11));
#19196=CARTESIAN_POINT('Ctrl Pts',(7.27603390512273,-15.8295179709986,-4.20082013377291));
#19197=CARTESIAN_POINT('Ctrl Pts',(4.85068927007173,-15.6545179709986,-8.40164026752836));
#19198=CARTESIAN_POINT('Ctrl Pts',(-1.51301075899711E-11,-15.4795179709986,
-8.40164026751963));
#19199=CARTESIAN_POINT('Ctrl Pts',(-4.85068927010199,-15.3045179709986,
-8.4016402675109));
#19200=CARTESIAN_POINT('Ctrl Pts',(-7.27603390513785,-15.1295179709986,
-4.20082013374671));
#19201=CARTESIAN_POINT('Ctrl Pts',(-9.70137854017372,-14.9545179709986,
1.74701493417668E-11));
#19202=CARTESIAN_POINT('Ctrl Pts',(-7.27603390512272,-14.7795179709986,
4.20082013377292));
#19203=CARTESIAN_POINT('Ctrl Pts',(-4.85068927007173,-14.6045179709986,
8.40164026752836));
#19204=CARTESIAN_POINT('Ctrl Pts',(1.5129078685785E-11,-14.4295179709986,
8.40164026751963));
#19205=CARTESIAN_POINT('Ctrl Pts',(4.85068927010198,-14.2545179709986,8.4016402675109));
#19206=CARTESIAN_POINT('Ctrl Pts',(7.27603390513785,-14.0795179709986,4.20082013374672));
#19207=CARTESIAN_POINT('Ctrl Pts',(9.70137854017372,-13.9045179709986,-1.74689612655491E-11));
#19208=CARTESIAN_POINT('Ctrl Pts',(7.27603390512273,-13.7295179709986,-4.20082013377291));
#19209=CARTESIAN_POINT('Ctrl Pts',(4.85068927007173,-13.5545179709986,-8.40164026752836));
#19210=CARTESIAN_POINT('Ctrl Pts',(-1.51301075899711E-11,-13.3795179709986,
-8.40164026751963));
#19211=CARTESIAN_POINT('Ctrl Pts',(-4.85068927010199,-13.2045179709986,
-8.4016402675109));
#19212=CARTESIAN_POINT('Ctrl Pts',(-7.27603390513785,-13.0295179709986,
-4.20082013374671));
#19213=CARTESIAN_POINT('Ctrl Pts',(-9.70137854017372,-12.8545179709986,
1.74701493417668E-11));
#19214=CARTESIAN_POINT('Ctrl Pts',(-7.27603390512272,-12.6795179709986,
4.20082013377292));
#19215=CARTESIAN_POINT('Ctrl Pts',(-4.85068927007173,-12.5045179709986,
8.40164026752836));
#19216=CARTESIAN_POINT('Ctrl Pts',(1.5129078685785E-11,-12.3295179709986,
8.40164026751963));
#19217=CARTESIAN_POINT('Ctrl Pts',(4.85068927010198,-12.1545179709986,8.4016402675109));
#19218=CARTESIAN_POINT('Ctrl Pts',(7.27603390513785,-11.9795179709986,4.20082013374672));
#19219=CARTESIAN_POINT('Ctrl Pts',(9.70137854017372,-11.8045179709986,-1.74689612655491E-11));
#19220=CARTESIAN_POINT('Ctrl Pts',(7.27603390512273,-11.6295179709986,-4.20082013377291));
#19221=CARTESIAN_POINT('Ctrl Pts',(4.85068927007173,-11.4545179709986,-8.40164026752836));
#19222=CARTESIAN_POINT('Ctrl Pts',(-1.51301075899711E-11,-11.2795179709986,
-8.40164026751963));
#19223=CARTESIAN_POINT('Ctrl Pts',(-4.85068927010199,-11.1045179709986,
-8.4016402675109));
#19224=CARTESIAN_POINT('Ctrl Pts',(-7.27603390513785,-10.9295179709986,
-4.20082013374671));
#19225=CARTESIAN_POINT('Ctrl Pts',(-9.70137854017372,-10.7545179709986,
1.74701493417668E-11));
#19226=CARTESIAN_POINT('Ctrl Pts',(-7.27603390512272,-10.5795179709986,
4.20082013377292));
#19227=CARTESIAN_POINT('Ctrl Pts',(-4.85068927007173,-10.4045179709986,
8.40164026752836));
#19228=CARTESIAN_POINT('Ctrl Pts',(1.5129078685785E-11,-10.2295179709986,
8.40164026751963));
#19229=CARTESIAN_POINT('Ctrl Pts',(4.85068927010198,-10.0545179709986,8.4016402675109));
#19230=CARTESIAN_POINT('Ctrl Pts',(7.27603390513785,-9.87951797099859,4.20082013374672));
#19231=CARTESIAN_POINT('Ctrl Pts',(9.70137854017372,-9.70451797099858,-1.74689612655491E-11));
#19232=CARTESIAN_POINT('Ctrl Pts',(7.27603390512273,-9.52951797099857,-4.20082013377291));
#19233=CARTESIAN_POINT('Ctrl Pts',(4.85068927007173,-9.3545179709986,-8.40164026752836));
#19234=CARTESIAN_POINT('Ctrl Pts',(-1.51301075899711E-11,-9.17951797099859,
-8.40164026751963));
#19235=CARTESIAN_POINT('Ctrl Pts',(-4.85068927010199,-9.00451797099858,
-8.4016402675109));
#19236=CARTESIAN_POINT('Ctrl Pts',(-7.27603390513785,-8.8295179709986,-4.20082013374671));
#19237=CARTESIAN_POINT('Ctrl Pts',(-9.70137854017372,-8.65451797099859,
1.74701493417668E-11));
#19238=CARTESIAN_POINT('Ctrl Pts',(-7.27603390512272,-8.47951797099858,
4.20082013377292));
#19239=CARTESIAN_POINT('Ctrl Pts',(-4.85068927007173,-8.3045179709986,8.40164026752836));
#19240=CARTESIAN_POINT('Ctrl Pts',(1.5129078685785E-11,-8.12951797099859,
8.40164026751963));
#19241=CARTESIAN_POINT('Ctrl Pts',(4.85068927010198,-7.95451797099859,8.4016402675109));
#19242=CARTESIAN_POINT('Ctrl Pts',(7.27603390513785,-7.7795179709986,4.20082013374672));
#19243=CARTESIAN_POINT('Ctrl Pts',(9.70137854017372,-7.60451797099859,-1.74689612655491E-11));
#19244=CARTESIAN_POINT('Ctrl Pts',(7.27603390512273,-7.42951797099858,-4.20082013377291));
#19245=CARTESIAN_POINT('Ctrl Pts',(4.85068927007173,-7.25451797099861,-8.40164026752836));
#19246=CARTESIAN_POINT('Ctrl Pts',(-1.51301075899711E-11,-7.07951797099859,
-8.40164026751963));
#19247=CARTESIAN_POINT('Ctrl Pts',(-4.85068927010199,-6.90451797099859,
-8.4016402675109));
#19248=CARTESIAN_POINT('Ctrl Pts',(-7.27603390513785,-6.72951797099858,
-4.20082013374671));
#19249=CARTESIAN_POINT('Ctrl Pts',(-9.70137854017372,-6.5545179709986,1.74701493417668E-11));
#19250=CARTESIAN_POINT('Ctrl Pts',(-7.27603390512272,-6.37951797099859,
4.20082013377292));
#19251=CARTESIAN_POINT('Ctrl Pts',(-4.85068927007173,-6.20451797099858,
8.40164026752836));
#19252=CARTESIAN_POINT('Ctrl Pts',(1.5129078685785E-11,-6.0295179709986,
8.40164026751963));
#19253=CARTESIAN_POINT('Ctrl Pts',(4.85068927010198,-5.8545179709986,8.4016402675109));
#19254=CARTESIAN_POINT('Ctrl Pts',(7.27603390513785,-5.67951797099858,4.20082013374672));
#19255=CARTESIAN_POINT('Ctrl Pts',(9.70137854017372,-5.5045179709986,-1.74689612655491E-11));
#19256=CARTESIAN_POINT('Ctrl Pts',(7.27603390512273,-5.32951797099859,-4.20082013377291));
#19257=CARTESIAN_POINT('Ctrl Pts',(4.85068927007173,-5.15451797099859,-8.40164026752836));
#19258=CARTESIAN_POINT('Ctrl Pts',(-1.51301075899711E-11,-4.9795179709986,
-8.40164026751963));
#19259=CARTESIAN_POINT('Ctrl Pts',(-4.85068927010199,-4.8045179709986,-8.4016402675109));
#19260=CARTESIAN_POINT('Ctrl Pts',(-7.27603390513785,-4.62951797099859,
-4.20082013374671));
#19261=CARTESIAN_POINT('Ctrl Pts',(-9.70137854017372,-4.45451797099861,
1.74701493417668E-11));
#19262=CARTESIAN_POINT('Ctrl Pts',(-7.27603390512272,-4.2795179709986,4.20082013377292));
#19263=CARTESIAN_POINT('Ctrl Pts',(-4.85068927007173,-4.10451797099859,
8.40164026752836));
#19264=CARTESIAN_POINT('Ctrl Pts',(1.5129078685785E-11,-3.92951797099861,
8.40164026751963));
#19265=CARTESIAN_POINT('Ctrl Pts',(4.85068927010198,-3.75451797099861,8.4016402675109));
#19266=CARTESIAN_POINT('Ctrl Pts',(7.27603390513785,-3.57951797099859,4.20082013374672));
#19267=CARTESIAN_POINT('Ctrl Pts',(9.70137854017372,-3.40451797099861,-1.74689612655491E-11));
#19268=CARTESIAN_POINT('Ctrl Pts',(7.27603390512273,-3.2295179709986,-4.20082013377291));
#19269=CARTESIAN_POINT('Ctrl Pts',(4.85068927007173,-3.0545179709986,-8.40164026752836));
#19270=CARTESIAN_POINT('Ctrl Pts',(-1.51301075899711E-11,-2.87951797099861,
-8.40164026751963));
#19271=CARTESIAN_POINT('Ctrl Pts',(-4.85068927010199,-2.70451797099861,
-8.4016402675109));
#19272=CARTESIAN_POINT('Ctrl Pts',(-7.27603390513785,-2.5295179709986,-4.20082013374671));
#19273=CARTESIAN_POINT('Ctrl Pts',(-9.70137854017372,-2.3545179709986,1.74701493417668E-11));
#19274=CARTESIAN_POINT('Ctrl Pts',(-7.27603390512272,-2.17951797099861,
4.20082013377292));
#19275=CARTESIAN_POINT('Ctrl Pts',(-4.85068927007173,-2.0045179709986,8.40164026752836));
#19276=CARTESIAN_POINT('Ctrl Pts',(1.5129078685785E-11,-1.82951797099859,
8.40164026751963));
#19277=CARTESIAN_POINT('Ctrl Pts',(4.85068927010198,-1.65451797099861,8.4016402675109));
#19278=CARTESIAN_POINT('Ctrl Pts',(7.27603390513785,-1.4795179709986,4.20082013374672));
#19279=CARTESIAN_POINT('Ctrl Pts',(9.70137854017372,-1.3045179709986,-1.74689612655491E-11));
#19280=CARTESIAN_POINT('Ctrl Pts',(7.27603390512273,-1.12951797099861,-4.20082013377291));
#19281=CARTESIAN_POINT('Ctrl Pts',(4.85068927007173,-0.954517970998605,
-8.40164026752836));
#19282=CARTESIAN_POINT('Ctrl Pts',(-1.51301075899711E-11,-0.779517970998594,
-8.40164026751963));
#19283=CARTESIAN_POINT('Ctrl Pts',(-4.85068927010199,-0.604517970998614,
-8.4016402675109));
#19284=CARTESIAN_POINT('Ctrl Pts',(-7.27603390513785,-0.429517970998605,
-4.20082013374671));
#19285=CARTESIAN_POINT('Ctrl Pts',(-9.70137854017372,-0.2545179709986,1.74701493417668E-11));
#19286=CARTESIAN_POINT('Ctrl Pts',(-7.27603390512272,-0.079517970998616,
4.20082013377292));
#19287=CARTESIAN_POINT('Ctrl Pts',(-4.85068927007173,0.0954820290013905,
8.40164026752836));
#19288=CARTESIAN_POINT('Ctrl Pts',(1.5129078685785E-11,0.270482029001401,
8.40164026751963));
#19289=CARTESIAN_POINT('Ctrl Pts',(4.85068927010198,0.445482029001381,8.4016402675109));
#19290=CARTESIAN_POINT('Ctrl Pts',(7.27603390513785,0.62048202900139,4.20082013374672));
#19291=CARTESIAN_POINT('Ctrl Pts',(9.70137854017372,0.795482029001395,-1.74689612655491E-11));
#19292=CARTESIAN_POINT('Ctrl Pts',(7.27603390512273,0.970482029001379,-4.20082013377291));
#19293=CARTESIAN_POINT('Ctrl Pts',(4.85068927007173,1.14548202900139,-8.40164026752836));
#19294=CARTESIAN_POINT('Ctrl Pts',(-1.51301075899711E-11,1.3204820290014,
-8.40164026751963));
#19295=CARTESIAN_POINT('Ctrl Pts',(-4.85068927010199,1.49548202900138,-8.4016402675109));
#19296=CARTESIAN_POINT('Ctrl Pts',(-7.27603390513785,1.67048202900139,-4.20082013374671));
#19297=CARTESIAN_POINT('Ctrl Pts',(-9.70137854017372,1.84548202900139,1.74701493417668E-11));
#19298=CARTESIAN_POINT('Ctrl Pts',(-7.27603390512272,2.0204820290014,4.20082013377292));
#19299=CARTESIAN_POINT('Ctrl Pts',(-4.85068927007173,2.19548202900138,8.40164026752836));
#19300=CARTESIAN_POINT('Ctrl Pts',(1.5129078685785E-11,2.37048202900139,
8.40164026751963));
#19301=CARTESIAN_POINT('Ctrl Pts',(4.85068927010198,2.5454820290014,8.4016402675109));
#19302=CARTESIAN_POINT('Ctrl Pts',(7.27603390513785,2.72048202900138,4.20082013374672));
#19303=CARTESIAN_POINT('Ctrl Pts',(9.70137854017372,2.89548202900139,-1.74689612655491E-11));
#19304=CARTESIAN_POINT('Ctrl Pts',(7.27603390512273,3.0704820290014,-4.20082013377291));
#19305=CARTESIAN_POINT('Ctrl Pts',(4.85068927007173,3.24548202900138,-8.40164026752836));
#19306=CARTESIAN_POINT('Ctrl Pts',(-1.51301075899711E-11,3.42048202900139,
-8.40164026751963));
#19307=CARTESIAN_POINT('Ctrl Pts',(-4.85068927010199,3.59548202900139,-8.4016402675109));
#19308=CARTESIAN_POINT('Ctrl Pts',(-7.27603390513785,3.77048202900138,-4.20082013374671));
#19309=CARTESIAN_POINT('Ctrl Pts',(-9.70137854017372,3.94548202900138,1.74701493417668E-11));
#19310=CARTESIAN_POINT('Ctrl Pts',(-7.27603390512272,4.12048202900139,4.20082013377292));
#19311=CARTESIAN_POINT('Ctrl Pts',(-4.85068927007173,4.29548202900137,8.40164026752836));
#19312=CARTESIAN_POINT('Ctrl Pts',(1.5129078685785E-11,4.47048202900138,
8.40164026751963));
#19313=CARTESIAN_POINT('Ctrl Pts',(4.85068927010198,4.64548202900139,8.4016402675109));
#19314=CARTESIAN_POINT('Ctrl Pts',(7.27603390513785,4.82048202900137,4.20082013374672));
#19315=CARTESIAN_POINT('Ctrl Pts',(9.70137854017372,4.99548202900138,-1.74689612655491E-11));
#19316=CARTESIAN_POINT('Ctrl Pts',(7.27603390512273,5.17048202900139,-4.20082013377291));
#19317=CARTESIAN_POINT('Ctrl Pts',(4.85068927007173,5.34548202900137,-8.40164026752836));
#19318=CARTESIAN_POINT('Ctrl Pts',(-1.51301075899711E-11,5.52048202900138,
-8.40164026751963));
#19319=CARTESIAN_POINT('Ctrl Pts',(-4.85068927010199,5.69548202900138,-8.4016402675109));
#19320=CARTESIAN_POINT('Ctrl Pts',(-7.27603390513785,5.87048202900137,-4.20082013374671));
#19321=CARTESIAN_POINT('Ctrl Pts',(-9.70137854017372,6.04548202900137,1.74701493417668E-11));
#19322=CARTESIAN_POINT('Ctrl Pts',(-7.27603390512272,6.22048202900138,4.20082013377292));
#19323=CARTESIAN_POINT('Ctrl Pts',(-4.85068927007173,6.39548202900136,8.40164026752836));
#19324=CARTESIAN_POINT('Ctrl Pts',(1.5129078685785E-11,6.57048202900137,
8.40164026751963));
#19325=CARTESIAN_POINT('Ctrl Pts',(4.85068927010198,6.74548202900138,8.4016402675109));
#19326=CARTESIAN_POINT('Ctrl Pts',(7.27603390513785,6.92048202900139,4.20082013374672));
#19327=CARTESIAN_POINT('Ctrl Pts',(9.70137854017372,7.09548202900137,-1.74689612655491E-11));
#19328=CARTESIAN_POINT('Ctrl Pts',(7.27603390512273,7.27048202900138,-4.20082013377291));
#19329=CARTESIAN_POINT('Ctrl Pts',(4.85068927007173,7.44548202900138,-8.40164026752836));
#19330=CARTESIAN_POINT('Ctrl Pts',(-1.51301075899711E-11,7.62048202900137,
-8.40164026751963));
#19331=CARTESIAN_POINT('Ctrl Pts',(-4.85068927010199,7.79548202900137,-8.4016402675109));
#19332=CARTESIAN_POINT('Ctrl Pts',(-7.27603390513785,7.97048202900139,-4.20082013374671));
#19333=CARTESIAN_POINT('Ctrl Pts',(-9.70137854017372,8.14548202900136,1.74701493417668E-11));
#19334=CARTESIAN_POINT('Ctrl Pts',(-7.27603390512272,8.32048202900138,4.20082013377292));
#19335=CARTESIAN_POINT('Ctrl Pts',(-4.85068927007173,8.49548202900138,8.40164026752836));
#19336=CARTESIAN_POINT('Ctrl Pts',(1.5129078685785E-11,8.67048202900136,
8.40164026751963));
#19337=CARTESIAN_POINT('Ctrl Pts',(4.85068927010198,8.84548202900137,8.4016402675109));
#19338=CARTESIAN_POINT('Ctrl Pts',(7.27603390513785,9.02048202900138,4.20082013374672));
#19339=CARTESIAN_POINT('Ctrl Pts',(9.70137854017372,9.19548202900136,-1.74689612655491E-11));
#19340=CARTESIAN_POINT('Ctrl Pts',(7.27603390512273,9.37048202900137,-4.20082013377291));
#19341=CARTESIAN_POINT('Ctrl Pts',(4.85068927007173,9.54548202900137,-8.40164026752836));
#19342=CARTESIAN_POINT('Ctrl Pts',(-1.51301075899711E-11,9.72048202900136,
-8.40164026751963));
#19343=CARTESIAN_POINT('Ctrl Pts',(-4.85068927010199,9.89548202900136,-8.4016402675109));
#19344=CARTESIAN_POINT('Ctrl Pts',(-7.27603390513785,10.0704820290014,-4.20082013374671));
#19345=CARTESIAN_POINT('Ctrl Pts',(-9.70137854017372,10.2454820290014,1.74701493417668E-11));
#19346=CARTESIAN_POINT('Ctrl Pts',(-7.27603390512272,10.4204820290014,4.20082013377292));
#19347=CARTESIAN_POINT('Ctrl Pts',(-4.85068927007173,10.5954820290014,8.40164026752836));
#19348=CARTESIAN_POINT('Ctrl Pts',(1.5129078685785E-11,10.7704820290014,
8.40164026751963));
#19349=CARTESIAN_POINT('Ctrl Pts',(4.85068927010198,10.9454820290014,8.4016402675109));
#19350=CARTESIAN_POINT('Ctrl Pts',(7.27603390513785,11.1204820290014,4.20082013374672));
#19351=CARTESIAN_POINT('Ctrl Pts',(9.70137854017372,11.2954820290014,-1.74689612655491E-11));
#19352=CARTESIAN_POINT('Ctrl Pts',(7.27603390512273,11.4704820290014,-4.20082013377291));
#19353=CARTESIAN_POINT('Ctrl Pts',(4.85068927007173,11.6454820290014,-8.40164026752836));
#19354=CARTESIAN_POINT('Ctrl Pts',(-1.51301075899711E-11,11.8204820290014,
-8.40164026751963));
#19355=CARTESIAN_POINT('Ctrl Pts',(-4.85068927010199,11.9954820290014,-8.4016402675109));
#19356=CARTESIAN_POINT('Ctrl Pts',(-7.27603390513785,12.1704820290014,-4.20082013374671));
#19357=CARTESIAN_POINT('Ctrl Pts',(-9.70137854017372,12.3454820290014,1.74701493417668E-11));
#19358=CARTESIAN_POINT('Ctrl Pts',(-7.27603390512272,12.5204820290014,4.20082013377292));
#19359=CARTESIAN_POINT('Ctrl Pts',(-4.85068927007173,12.6954820290014,8.40164026752836));
#19360=CARTESIAN_POINT('Ctrl Pts',(1.5129078685785E-11,12.8704820290014,
8.40164026751963));
#19361=CARTESIAN_POINT('Ctrl Pts',(4.85068927010198,13.0454820290013,8.4016402675109));
#19362=CARTESIAN_POINT('Ctrl Pts',(7.27603390513785,13.2204820290014,4.20082013374672));
#19363=CARTESIAN_POINT('Ctrl Pts',(9.70137854017372,13.3954820290014,-1.74689612655491E-11));
#19364=CARTESIAN_POINT('Ctrl Pts',(7.27603390512273,13.5704820290014,-4.20082013377291));
#19365=CARTESIAN_POINT('Ctrl Pts',(4.85068927007173,13.7454820290014,-8.40164026752836));
#19366=CARTESIAN_POINT('Ctrl Pts',(-1.51301075899711E-11,13.9204820290014,
-8.40164026751963));
#19367=CARTESIAN_POINT('Ctrl Pts',(-4.85068927010199,14.0954820290013,-8.4016402675109));
#19368=CARTESIAN_POINT('Ctrl Pts',(-7.27603390513785,14.2704820290014,-4.20082013374671));
#19369=CARTESIAN_POINT('Ctrl Pts',(-9.70137854017372,14.4454820290014,1.74701493417668E-11));
#19370=CARTESIAN_POINT('Ctrl Pts',(-7.27603390512272,14.6204820290013,4.20082013377292));
#19371=CARTESIAN_POINT('Ctrl Pts',(-4.85068927007173,14.7954820290014,8.40164026752836));
#19372=CARTESIAN_POINT('Ctrl Pts',(1.5129078685785E-11,14.9704820290014,
8.40164026751963));
#19373=CARTESIAN_POINT('Ctrl Pts',(4.85068927010198,15.1454820290013,8.4016402675109));
#19374=CARTESIAN_POINT('Ctrl Pts',(7.27603390513785,15.3204820290014,4.20082013374672));
#19375=CARTESIAN_POINT('Ctrl Pts',(9.70137854017372,15.4954820290014,-1.74689612655491E-11));
#19376=CARTESIAN_POINT('Ctrl Pts',(7.27603390512273,15.6704820290014,-4.20082013377291));
#19377=CARTESIAN_POINT('Ctrl Pts',(4.85068927007173,15.8454820290013,-8.40164026752836));
#19378=CARTESIAN_POINT('Ctrl Pts',(-1.51301075899711E-11,16.0204820290014,
-8.40164026751963));
#19379=CARTESIAN_POINT('Ctrl Pts',(-4.85068927010199,16.1954820290014,-8.4016402675109));
#19380=CARTESIAN_POINT('Ctrl Pts',(-7.27603390513785,16.3704820290014,-4.20082013374671));
#19381=CARTESIAN_POINT('Ctrl Pts',(-9.70137854017372,16.5454820290013,1.74701493417668E-11));
#19382=CARTESIAN_POINT('Ctrl Pts',(-7.27603390512272,16.7204820290014,4.20082013377292));
#19383=CARTESIAN_POINT('Ctrl Pts',(-4.85068927007173,16.8954820290013,8.40164026752836));
#19384=CARTESIAN_POINT('Ctrl Pts',(1.5129078685785E-11,17.0704820290014,
8.40164026751963));
#19385=CARTESIAN_POINT('Ctrl Pts',(4.85068927010198,17.2454820290014,8.4016402675109));
#19386=CARTESIAN_POINT('Ctrl Pts',(7.27603390513785,17.4204820290013,4.20082013374672));
#19387=CARTESIAN_POINT('Ctrl Pts',(9.70137854017372,17.5954820290013,-1.74689612655491E-11));
#19388=CARTESIAN_POINT('Ctrl Pts',(7.27603390512273,17.7704820290014,-4.20082013377291));
#19389=CARTESIAN_POINT('Ctrl Pts',(4.85068927007173,17.9454820290013,-8.40164026752836));
#19390=CARTESIAN_POINT('Ctrl Pts',(-1.51301075899711E-11,18.1204820290014,
-8.40164026751963));
#19391=CARTESIAN_POINT('Ctrl Pts',(-4.85068927010199,18.2954820290014,-8.4016402675109));
#19392=CARTESIAN_POINT('Ctrl Pts',(-7.27603390513785,18.4704820290013,-4.20082013374671));
#19393=CARTESIAN_POINT('Ctrl Pts',(-9.70137854017372,18.6454820290013,1.74701493417668E-11));
#19394=CARTESIAN_POINT('Ctrl Pts',(-7.27603390512272,18.8204820290014,4.20082013377292));
#19395=CARTESIAN_POINT('Ctrl Pts',(-4.85068927007173,18.9954820290013,8.40164026752836));
#19396=CARTESIAN_POINT('Ctrl Pts',(1.5129078685785E-11,19.1704820290013,
8.40164026751963));
#19397=CARTESIAN_POINT('Ctrl Pts',(4.85068927010198,19.3454820290014,8.4016402675109));
#19398=CARTESIAN_POINT('Ctrl Pts',(7.27603390513785,19.5204820290013,4.20082013374672));
#19399=CARTESIAN_POINT('Ctrl Pts',(9.70137854017372,19.6954820290013,-1.74689612655491E-11));
#19400=CARTESIAN_POINT('Ctrl Pts',(7.27603390512273,19.8704820290014,-4.20082013377291));
#19401=CARTESIAN_POINT('Ctrl Pts',(4.85068927007173,20.0454820290014,-8.40164026752836));
#19402=CARTESIAN_POINT('Ctrl Pts',(-1.51301075899711E-11,20.2204820290013,
-8.40164026751963));
#19403=CARTESIAN_POINT('Ctrl Pts',(-4.85068927010199,20.3954820290014,-8.4016402675109));
#19404=CARTESIAN_POINT('Ctrl Pts',(-7.27603390513785,20.5704820290014,-4.20082013374671));
#19405=CARTESIAN_POINT('Ctrl Pts',(-9.70137854017372,20.7454820290013,1.74701493417668E-11));
#19406=CARTESIAN_POINT('Ctrl Pts',(-7.27603390512272,20.9204820290013,4.20082013377292));
#19407=CARTESIAN_POINT('Ctrl Pts',(-4.85068927007173,21.0954820290014,8.40164026752836));
#19408=CARTESIAN_POINT('Ctrl Pts',(1.5129078685785E-11,21.2704820290013,
8.40164026751963));
#19409=CARTESIAN_POINT('Ctrl Pts',(4.85068927010198,21.4454820290013,8.4016402675109));
#19410=CARTESIAN_POINT('Ctrl Pts',(7.27603390513785,21.6204820290014,4.20082013374672));
#19411=CARTESIAN_POINT('Ctrl Pts',(9.70137854017372,21.7954820290013,-1.74689612655491E-11));
#19412=CARTESIAN_POINT('Ctrl Pts',(7.27603390512273,21.9704820290013,-4.20082013377291));
#19413=CARTESIAN_POINT('Ctrl Pts',(4.85068927007173,22.1454820290013,-8.40164026752836));
#19414=CARTESIAN_POINT('Ctrl Pts',(-1.51301075899711E-11,22.3204820290013,
-8.40164026751963));
#19415=CARTESIAN_POINT('Ctrl Pts',(-4.85068927010199,22.4954820290013,-8.4016402675109));
#19416=CARTESIAN_POINT('Ctrl Pts',(-7.27603390513785,22.6704820290013,-4.20082013374671));
#19417=CARTESIAN_POINT('Ctrl Pts',(-9.70137854017372,22.8454820290013,1.74701493417668E-11));
#19418=CARTESIAN_POINT('Ctrl Pts',(-7.27603390512272,23.0204820290013,4.20082013377292));
#19419=CARTESIAN_POINT('Ctrl Pts',(-4.85068927007173,23.1954820290013,8.40164026752836));
#19420=CARTESIAN_POINT('Ctrl Pts',(1.5129078685785E-11,23.3704820290013,
8.40164026751963));
#19421=CARTESIAN_POINT('Ctrl Pts',(4.85068927010198,23.5454820290013,8.4016402675109));
#19422=CARTESIAN_POINT('Ctrl Pts',(7.27603390513785,23.7204820290013,4.20082013374672));
#19423=CARTESIAN_POINT('Ctrl Pts',(9.70137854017372,23.8954820290013,-1.74689612655491E-11));
#19424=CARTESIAN_POINT('Ctrl Pts',(7.27603390512273,24.0704820290013,-4.20082013377291));
#19425=CARTESIAN_POINT('Ctrl Pts',(4.85068927007173,24.2454820290013,-8.40164026752836));
#19426=CARTESIAN_POINT('Ctrl Pts',(-1.51301075899711E-11,24.4204820290013,
-8.40164026751963));
#19427=CARTESIAN_POINT('Ctrl Pts',(-4.85068927010199,24.5954820290013,-8.4016402675109));
#19428=CARTESIAN_POINT('Ctrl Pts',(-7.27603390513785,24.7704820290013,-4.20082013374671));
#19429=CARTESIAN_POINT('Ctrl Pts',(-9.70137854017372,24.9454820290013,1.74701493417668E-11));
#19430=CARTESIAN_POINT('Ctrl Pts',(-7.27603390512272,25.1204820290013,4.20082013377292));
#19431=CARTESIAN_POINT('Ctrl Pts',(-4.85068927007173,25.2954820290013,8.40164026752836));
#19432=CARTESIAN_POINT('Ctrl Pts',(1.5129078685785E-11,25.4704820290013,
8.40164026751963));
#19433=CARTESIAN_POINT('Ctrl Pts',(4.85068927010198,25.6454820290013,8.4016402675109));
#19434=CARTESIAN_POINT('Ctrl Pts',(7.27603390513785,25.8204820290013,4.20082013374672));
#19435=CARTESIAN_POINT('Ctrl Pts',(9.70137854017372,25.9954820290013,-1.74689612655491E-11));
#19436=CARTESIAN_POINT('Ctrl Pts',(7.27603390512273,26.1704820290013,-4.20082013377291));
#19437=CARTESIAN_POINT('Ctrl Pts',(4.85068927007173,26.3454820290013,-8.40164026752836));
#19438=CARTESIAN_POINT('Ctrl Pts',(-1.51301075899711E-11,26.5204820290013,
-8.40164026751963));
#19439=CARTESIAN_POINT('Ctrl Pts',(-1.51301029103127E-11,-143.579519323734,
-8.40163766893887));
#19440=CARTESIAN_POINT('Ctrl Pts',(-4.85068776981069,-143.404519323734,
-8.40163766893014));
#19441=CARTESIAN_POINT('Ctrl Pts',(-7.2760316547009,-143.229519323734,-4.20081883445633));
#19442=CARTESIAN_POINT('Ctrl Pts',(-9.70137553959111,-143.054519323734,
1.74701439383464E-11));
#19443=CARTESIAN_POINT('Ctrl Pts',(-7.27603165468577,-142.879519323734,
4.20081883448254));
#19444=CARTESIAN_POINT('Ctrl Pts',(-4.85068776978043,-142.704519323734,
8.40163766894761));
#19445=CARTESIAN_POINT('Ctrl Pts',(1.51290740064448E-11,-142.529519323734,
8.40163766893887));
#19446=CARTESIAN_POINT('Ctrl Pts',(4.85068776981068,-142.354519323734,8.40163766893014));
#19447=CARTESIAN_POINT('Ctrl Pts',(7.2760316547009,-142.179519323734,4.20081883445634));
#19448=CARTESIAN_POINT('Ctrl Pts',(9.70137553959111,-142.004519323734,-1.74689558624962E-11));
#19449=CARTESIAN_POINT('Ctrl Pts',(7.27603165468577,-141.829519323734,-4.20081883448253));
#19450=CARTESIAN_POINT('Ctrl Pts',(4.85068776978043,-141.654519323734,-8.4016376689476));
#19451=CARTESIAN_POINT('Ctrl Pts',(-1.51301029103127E-11,-141.479519323734,
-8.40163766893887));
#19452=CARTESIAN_POINT('Ctrl Pts',(-4.85068776981069,-141.304519323734,
-8.40163766893014));
#19453=CARTESIAN_POINT('Ctrl Pts',(-7.2760316547009,-141.129519323734,-4.20081883445633));
#19454=CARTESIAN_POINT('Ctrl Pts',(-9.70137553959111,-140.954519323734,
1.74701439383464E-11));
#19455=CARTESIAN_POINT('Ctrl Pts',(-7.27603165468577,-140.779519323734,
4.20081883448254));
#19456=CARTESIAN_POINT('Ctrl Pts',(-4.85068776978043,-140.604519323734,
8.40163766894761));
#19457=CARTESIAN_POINT('Ctrl Pts',(1.51290740064448E-11,-140.429519323734,
8.40163766893887));
#19458=CARTESIAN_POINT('Ctrl Pts',(4.85068776981068,-140.254519323734,8.40163766893014));
#19459=CARTESIAN_POINT('Ctrl Pts',(7.2760316547009,-140.079519323734,4.20081883445634));
#19460=CARTESIAN_POINT('Ctrl Pts',(9.70137553959111,-139.904519323734,-1.74689558624962E-11));
#19461=CARTESIAN_POINT('Ctrl Pts',(7.27603165468577,-139.729519323734,-4.20081883448253));
#19462=CARTESIAN_POINT('Ctrl Pts',(4.85068776978043,-139.554519323734,-8.4016376689476));
#19463=CARTESIAN_POINT('Ctrl Pts',(-1.51301029103127E-11,-139.379519323734,
-8.40163766893887));
#19464=CARTESIAN_POINT('Ctrl Pts',(-4.85068776981069,-139.204519323734,
-8.40163766893014));
#19465=CARTESIAN_POINT('Ctrl Pts',(-7.2760316547009,-139.029519323734,-4.20081883445633));
#19466=CARTESIAN_POINT('Ctrl Pts',(-9.70137553959111,-138.854519323734,
1.74701439383464E-11));
#19467=CARTESIAN_POINT('Ctrl Pts',(-7.27603165468577,-138.679519323734,
4.20081883448254));
#19468=CARTESIAN_POINT('Ctrl Pts',(-4.85068776978043,-138.504519323734,
8.40163766894761));
#19469=CARTESIAN_POINT('Ctrl Pts',(1.51290740064448E-11,-138.329519323734,
8.40163766893887));
#19470=CARTESIAN_POINT('Ctrl Pts',(4.85068776981068,-138.154519323734,8.40163766893014));
#19471=CARTESIAN_POINT('Ctrl Pts',(7.2760316547009,-137.979519323734,4.20081883445634));
#19472=CARTESIAN_POINT('Ctrl Pts',(9.70137553959111,-137.804519323734,-1.74689558624962E-11));
#19473=CARTESIAN_POINT('Ctrl Pts',(7.27603165468577,-137.629519323734,-4.20081883448253));
#19474=CARTESIAN_POINT('Ctrl Pts',(4.85068776978043,-137.454519323734,-8.4016376689476));
#19475=CARTESIAN_POINT('Ctrl Pts',(-1.51301029103127E-11,-137.279519323734,
-8.40163766893887));
#19476=CARTESIAN_POINT('Ctrl Pts',(-4.85068776981069,-137.104519323734,
-8.40163766893014));
#19477=CARTESIAN_POINT('Ctrl Pts',(-7.2760316547009,-136.929519323734,-4.20081883445633));
#19478=CARTESIAN_POINT('Ctrl Pts',(-9.70137553959111,-136.754519323734,
1.74701439383464E-11));
#19479=CARTESIAN_POINT('Ctrl Pts',(-7.27603165468577,-136.579519323734,
4.20081883448254));
#19480=CARTESIAN_POINT('Ctrl Pts',(-4.85068776978043,-136.404519323734,
8.40163766894761));
#19481=CARTESIAN_POINT('Ctrl Pts',(1.51290740064448E-11,-136.229519323734,
8.40163766893887));
#19482=CARTESIAN_POINT('Ctrl Pts',(4.85068776981068,-136.054519323734,8.40163766893014));
#19483=CARTESIAN_POINT('Ctrl Pts',(7.2760316547009,-135.879519323734,4.20081883445634));
#19484=CARTESIAN_POINT('Ctrl Pts',(9.70137553959111,-135.704519323734,-1.74689558624962E-11));
#19485=CARTESIAN_POINT('Ctrl Pts',(7.27603165468577,-135.529519323734,-4.20081883448253));
#19486=CARTESIAN_POINT('Ctrl Pts',(4.85068776978043,-135.354519323734,-8.4016376689476));
#19487=CARTESIAN_POINT('Ctrl Pts',(-1.51301029103127E-11,-135.179519323734,
-8.40163766893887));
#19488=CARTESIAN_POINT('Ctrl Pts',(-4.85068776981069,-135.004519323734,
-8.40163766893014));
#19489=CARTESIAN_POINT('Ctrl Pts',(-7.2760316547009,-134.829519323734,-4.20081883445633));
#19490=CARTESIAN_POINT('Ctrl Pts',(-9.70137553959111,-134.654519323734,
1.74701439383464E-11));
#19491=CARTESIAN_POINT('Ctrl Pts',(-7.27603165468577,-134.479519323734,
4.20081883448254));
#19492=CARTESIAN_POINT('Ctrl Pts',(-4.85068776978043,-134.304519323734,
8.40163766894761));
#19493=CARTESIAN_POINT('Ctrl Pts',(1.51290740064448E-11,-134.129519323734,
8.40163766893887));
#19494=CARTESIAN_POINT('Ctrl Pts',(4.85068776981068,-133.954519323734,8.40163766893014));
#19495=CARTESIAN_POINT('Ctrl Pts',(7.2760316547009,-133.779519323734,4.20081883445634));
#19496=CARTESIAN_POINT('Ctrl Pts',(9.70137553959111,-133.604519323734,-1.74689558624962E-11));
#19497=CARTESIAN_POINT('Ctrl Pts',(7.27603165468577,-133.429519323734,-4.20081883448253));
#19498=CARTESIAN_POINT('Ctrl Pts',(4.85068776978043,-133.254519323734,-8.4016376689476));
#19499=CARTESIAN_POINT('Ctrl Pts',(-1.51301029103127E-11,-133.079519323734,
-8.40163766893887));
#19500=CARTESIAN_POINT('Ctrl Pts',(-4.85068776981069,-132.904519323734,
-8.40163766893014));
#19501=CARTESIAN_POINT('Ctrl Pts',(-7.2760316547009,-132.729519323734,-4.20081883445633));
#19502=CARTESIAN_POINT('Ctrl Pts',(-9.70137553959111,-132.554519323734,
1.74701439383464E-11));
#19503=CARTESIAN_POINT('Ctrl Pts',(-7.27603165468577,-132.379519323734,
4.20081883448254));
#19504=CARTESIAN_POINT('Ctrl Pts',(-4.85068776978043,-132.204519323734,
8.40163766894761));
#19505=CARTESIAN_POINT('Ctrl Pts',(1.51290740064448E-11,-132.029519323734,
8.40163766893887));
#19506=CARTESIAN_POINT('Ctrl Pts',(4.85068776981068,-131.854519323734,8.40163766893014));
#19507=CARTESIAN_POINT('Ctrl Pts',(7.2760316547009,-131.679519323734,4.20081883445634));
#19508=CARTESIAN_POINT('Ctrl Pts',(9.70137553959111,-131.504519323734,-1.74689558624962E-11));
#19509=CARTESIAN_POINT('Ctrl Pts',(7.27603165468577,-131.329519323734,-4.20081883448253));
#19510=CARTESIAN_POINT('Ctrl Pts',(4.85068776978043,-131.154519323734,-8.4016376689476));
#19511=CARTESIAN_POINT('Ctrl Pts',(-1.51301029103127E-11,-130.979519323734,
-8.40163766893887));
#19512=CARTESIAN_POINT('Ctrl Pts',(-4.85068776981069,-130.804519323734,
-8.40163766893014));
#19513=CARTESIAN_POINT('Ctrl Pts',(-7.2760316547009,-130.629519323734,-4.20081883445633));
#19514=CARTESIAN_POINT('Ctrl Pts',(-9.70137553959111,-130.454519323734,
1.74701439383464E-11));
#19515=CARTESIAN_POINT('Ctrl Pts',(-7.27603165468577,-130.279519323734,
4.20081883448254));
#19516=CARTESIAN_POINT('Ctrl Pts',(-4.85068776978043,-130.104519323734,
8.40163766894761));
#19517=CARTESIAN_POINT('Ctrl Pts',(1.51290740064448E-11,-129.929519323734,
8.40163766893887));
#19518=CARTESIAN_POINT('Ctrl Pts',(4.85068776981068,-129.754519323734,8.40163766893014));
#19519=CARTESIAN_POINT('Ctrl Pts',(7.2760316547009,-129.579519323734,4.20081883445634));
#19520=CARTESIAN_POINT('Ctrl Pts',(9.70137553959111,-129.404519323734,-1.74689558624962E-11));
#19521=CARTESIAN_POINT('Ctrl Pts',(7.27603165468577,-129.229519323734,-4.20081883448253));
#19522=CARTESIAN_POINT('Ctrl Pts',(4.85068776978043,-129.054519323734,-8.4016376689476));
#19523=CARTESIAN_POINT('Ctrl Pts',(-1.51301029103127E-11,-128.879519323734,
-8.40163766893887));
#19524=CARTESIAN_POINT('Ctrl Pts',(-4.85068776981069,-128.704519323734,
-8.40163766893014));
#19525=CARTESIAN_POINT('Ctrl Pts',(-7.2760316547009,-128.529519323734,-4.20081883445633));
#19526=CARTESIAN_POINT('Ctrl Pts',(-9.70137553959111,-128.354519323734,
1.74701439383464E-11));
#19527=CARTESIAN_POINT('Ctrl Pts',(-7.27603165468577,-128.179519323734,
4.20081883448254));
#19528=CARTESIAN_POINT('Ctrl Pts',(-4.85068776978043,-128.004519323734,
8.40163766894761));
#19529=CARTESIAN_POINT('Ctrl Pts',(1.51290740064448E-11,-127.829519323734,
8.40163766893887));
#19530=CARTESIAN_POINT('Ctrl Pts',(4.85068776981068,-127.654519323734,8.40163766893014));
#19531=CARTESIAN_POINT('Ctrl Pts',(7.2760316547009,-127.479519323734,4.20081883445634));
#19532=CARTESIAN_POINT('Ctrl Pts',(9.70137553959111,-127.304519323734,-1.74689558624962E-11));
#19533=CARTESIAN_POINT('Ctrl Pts',(7.27603165468577,-127.129519323734,-4.20081883448253));
#19534=CARTESIAN_POINT('Ctrl Pts',(4.85068776978043,-126.954519323734,-8.4016376689476));
#19535=CARTESIAN_POINT('Ctrl Pts',(-1.51301029103127E-11,-126.779519323734,
-8.40163766893887));
#19536=CARTESIAN_POINT('Ctrl Pts',(-4.85068776981069,-126.604519323734,
-8.40163766893014));
#19537=CARTESIAN_POINT('Ctrl Pts',(-7.2760316547009,-126.429519323734,-4.20081883445633));
#19538=CARTESIAN_POINT('Ctrl Pts',(-9.70137553959111,-126.254519323734,
1.74701439383464E-11));
#19539=CARTESIAN_POINT('Ctrl Pts',(-7.27603165468577,-126.079519323734,
4.20081883448254));
#19540=CARTESIAN_POINT('Ctrl Pts',(-4.85068776978043,-125.904519323734,
8.40163766894761));
#19541=CARTESIAN_POINT('Ctrl Pts',(1.51290740064448E-11,-125.729519323734,
8.40163766893887));
#19542=CARTESIAN_POINT('Ctrl Pts',(4.85068776981068,-125.554519323734,8.40163766893014));
#19543=CARTESIAN_POINT('Ctrl Pts',(7.2760316547009,-125.379519323734,4.20081883445634));
#19544=CARTESIAN_POINT('Ctrl Pts',(9.70137553959111,-125.204519323734,-1.74689558624962E-11));
#19545=CARTESIAN_POINT('Ctrl Pts',(7.27603165468577,-125.029519323734,-4.20081883448253));
#19546=CARTESIAN_POINT('Ctrl Pts',(4.85068776978043,-124.854519323734,-8.4016376689476));
#19547=CARTESIAN_POINT('Ctrl Pts',(-1.51301029103127E-11,-124.679519323734,
-8.40163766893887));
#19548=CARTESIAN_POINT('Ctrl Pts',(-4.85068776981069,-124.504519323734,
-8.40163766893014));
#19549=CARTESIAN_POINT('Ctrl Pts',(-7.2760316547009,-124.329519323734,-4.20081883445633));
#19550=CARTESIAN_POINT('Ctrl Pts',(-9.70137553959111,-124.154519323734,
1.74701439383464E-11));
#19551=CARTESIAN_POINT('Ctrl Pts',(-7.27603165468577,-123.979519323734,
4.20081883448254));
#19552=CARTESIAN_POINT('Ctrl Pts',(-4.85068776978043,-123.804519323734,
8.40163766894761));
#19553=CARTESIAN_POINT('Ctrl Pts',(1.51290740064448E-11,-123.629519323734,
8.40163766893887));
#19554=CARTESIAN_POINT('Ctrl Pts',(4.85068776981068,-123.454519323734,8.40163766893014));
#19555=CARTESIAN_POINT('Ctrl Pts',(7.2760316547009,-123.279519323734,4.20081883445634));
#19556=CARTESIAN_POINT('Ctrl Pts',(9.70137553959111,-123.104519323734,-1.74689558624962E-11));
#19557=CARTESIAN_POINT('Ctrl Pts',(7.27603165468577,-122.929519323734,-4.20081883448253));
#19558=CARTESIAN_POINT('Ctrl Pts',(4.85068776978043,-122.754519323734,-8.4016376689476));
#19559=CARTESIAN_POINT('Ctrl Pts',(-1.51301029103127E-11,-122.579519323734,
-8.40163766893887));
#19560=CARTESIAN_POINT('Ctrl Pts',(-4.85068776981069,-122.404519323734,
-8.40163766893014));
#19561=CARTESIAN_POINT('Ctrl Pts',(-7.2760316547009,-122.229519323734,-4.20081883445633));
#19562=CARTESIAN_POINT('Ctrl Pts',(-9.70137553959111,-122.054519323734,
1.74701439383464E-11));
#19563=CARTESIAN_POINT('Ctrl Pts',(-7.27603165468577,-121.879519323734,
4.20081883448254));
#19564=CARTESIAN_POINT('Ctrl Pts',(-4.85068776978043,-121.704519323734,
8.40163766894761));
#19565=CARTESIAN_POINT('Ctrl Pts',(1.51290740064448E-11,-121.529519323734,
8.40163766893887));
#19566=CARTESIAN_POINT('Ctrl Pts',(4.85068776981068,-121.354519323734,8.40163766893014));
#19567=CARTESIAN_POINT('Ctrl Pts',(7.2760316547009,-121.179519323734,4.20081883445634));
#19568=CARTESIAN_POINT('Ctrl Pts',(9.70137553959111,-121.004519323734,-1.74689558624962E-11));
#19569=CARTESIAN_POINT('Ctrl Pts',(7.27603165468577,-120.829519323734,-4.20081883448253));
#19570=CARTESIAN_POINT('Ctrl Pts',(4.85068776978043,-120.654519323734,-8.4016376689476));
#19571=CARTESIAN_POINT('Ctrl Pts',(-1.51301029103127E-11,-120.479519323734,
-8.40163766893887));
#19572=CARTESIAN_POINT('Ctrl Pts',(-4.85068776981069,-120.304519323734,
-8.40163766893014));
#19573=CARTESIAN_POINT('Ctrl Pts',(-7.2760316547009,-120.129519323734,-4.20081883445633));
#19574=CARTESIAN_POINT('Ctrl Pts',(-9.70137553959111,-119.954519323734,
1.74701439383464E-11));
#19575=CARTESIAN_POINT('Ctrl Pts',(-7.27603165468577,-119.779519323734,
4.20081883448254));
#19576=CARTESIAN_POINT('Ctrl Pts',(-4.85068776978043,-119.604519323734,
8.40163766894761));
#19577=CARTESIAN_POINT('Ctrl Pts',(1.51290740064448E-11,-119.429519323734,
8.40163766893887));
#19578=CARTESIAN_POINT('Ctrl Pts',(4.85068776981068,-119.254519323734,8.40163766893014));
#19579=CARTESIAN_POINT('Ctrl Pts',(7.2760316547009,-119.079519323734,4.20081883445634));
#19580=CARTESIAN_POINT('Ctrl Pts',(9.70137553959111,-118.904519323734,-1.74689558624962E-11));
#19581=CARTESIAN_POINT('Ctrl Pts',(7.27603165468577,-118.729519323734,-4.20081883448253));
#19582=CARTESIAN_POINT('Ctrl Pts',(4.85068776978043,-118.554519323734,-8.4016376689476));
#19583=CARTESIAN_POINT('Ctrl Pts',(-1.51301029103127E-11,-118.379519323734,
-8.40163766893887));
#19584=CARTESIAN_POINT('Ctrl Pts',(-4.85068776981069,-118.204519323734,
-8.40163766893014));
#19585=CARTESIAN_POINT('Ctrl Pts',(-7.2760316547009,-118.029519323734,-4.20081883445633));
#19586=CARTESIAN_POINT('Ctrl Pts',(-9.70137553959111,-117.854519323734,
1.74701439383464E-11));
#19587=CARTESIAN_POINT('Ctrl Pts',(-7.27603165468577,-117.679519323734,
4.20081883448254));
#19588=CARTESIAN_POINT('Ctrl Pts',(-4.85068776978043,-117.504519323734,
8.40163766894761));
#19589=CARTESIAN_POINT('Ctrl Pts',(1.51290740064448E-11,-117.329519323734,
8.40163766893887));
#19590=CARTESIAN_POINT('Ctrl Pts',(4.85068776981068,-117.154519323734,8.40163766893014));
#19591=CARTESIAN_POINT('Ctrl Pts',(7.2760316547009,-116.979519323734,4.20081883445634));
#19592=CARTESIAN_POINT('Ctrl Pts',(9.70137553959111,-116.804519323734,-1.74689558624962E-11));
#19593=CARTESIAN_POINT('Ctrl Pts',(7.27603165468577,-116.629519323734,-4.20081883448253));
#19594=CARTESIAN_POINT('Ctrl Pts',(4.85068776978043,-116.454519323734,-8.4016376689476));
#19595=CARTESIAN_POINT('Ctrl Pts',(-1.51301029103127E-11,-116.279519323734,
-8.40163766893887));
#19596=CARTESIAN_POINT('Ctrl Pts',(-4.85068776981069,-116.104519323734,
-8.40163766893014));
#19597=CARTESIAN_POINT('Ctrl Pts',(-7.2760316547009,-115.929519323734,-4.20081883445633));
#19598=CARTESIAN_POINT('Ctrl Pts',(-9.70137553959111,-115.754519323734,
1.74701439383464E-11));
#19599=CARTESIAN_POINT('Ctrl Pts',(-7.27603165468577,-115.579519323734,
4.20081883448254));
#19600=CARTESIAN_POINT('Ctrl Pts',(-4.85068776978043,-115.404519323734,
8.40163766894761));
#19601=CARTESIAN_POINT('Ctrl Pts',(1.51290740064448E-11,-115.229519323734,
8.40163766893887));
#19602=CARTESIAN_POINT('Ctrl Pts',(4.85068776981068,-115.054519323734,8.40163766893014));
#19603=CARTESIAN_POINT('Ctrl Pts',(7.2760316547009,-114.879519323734,4.20081883445634));
#19604=CARTESIAN_POINT('Ctrl Pts',(9.70137553959111,-114.704519323734,-1.74689558624962E-11));
#19605=CARTESIAN_POINT('Ctrl Pts',(7.27603165468577,-114.529519323734,-4.20081883448253));
#19606=CARTESIAN_POINT('Ctrl Pts',(4.85068776978043,-114.354519323734,-8.4016376689476));
#19607=CARTESIAN_POINT('Ctrl Pts',(-1.51301029103127E-11,-114.179519323734,
-8.40163766893887));
#19608=CARTESIAN_POINT('Ctrl Pts',(-4.85068776981069,-114.004519323734,
-8.40163766893014));
#19609=CARTESIAN_POINT('Ctrl Pts',(-7.2760316547009,-113.829519323734,-4.20081883445633));
#19610=CARTESIAN_POINT('Ctrl Pts',(-9.70137553959111,-113.654519323734,
1.74701439383464E-11));
#19611=CARTESIAN_POINT('Ctrl Pts',(-7.27603165468577,-113.479519323734,
4.20081883448254));
#19612=CARTESIAN_POINT('Ctrl Pts',(-4.85068776978043,-113.304519323734,
8.40163766894761));
#19613=CARTESIAN_POINT('Ctrl Pts',(1.51290740064448E-11,-113.129519323734,
8.40163766893887));
#19614=CARTESIAN_POINT('Ctrl Pts',(4.85068776981068,-112.954519323734,8.40163766893014));
#19615=CARTESIAN_POINT('Ctrl Pts',(7.2760316547009,-112.779519323734,4.20081883445634));
#19616=CARTESIAN_POINT('Ctrl Pts',(9.70137553959111,-112.604519323734,-1.74689558624962E-11));
#19617=CARTESIAN_POINT('Ctrl Pts',(7.27603165468577,-112.429519323734,-4.20081883448253));
#19618=CARTESIAN_POINT('Ctrl Pts',(4.85068776978043,-112.254519323734,-8.4016376689476));
#19619=CARTESIAN_POINT('Ctrl Pts',(-1.51301029103127E-11,-112.079519323734,
-8.40163766893887));
#19620=CARTESIAN_POINT('Ctrl Pts',(-4.85068776981069,-111.904519323734,
-8.40163766893014));
#19621=CARTESIAN_POINT('Ctrl Pts',(-7.2760316547009,-111.729519323734,-4.20081883445633));
#19622=CARTESIAN_POINT('Ctrl Pts',(-9.70137553959111,-111.554519323734,
1.74701439383464E-11));
#19623=CARTESIAN_POINT('Ctrl Pts',(-7.27603165468577,-111.379519323734,
4.20081883448254));
#19624=CARTESIAN_POINT('Ctrl Pts',(-4.85068776978043,-111.204519323734,
8.40163766894761));
#19625=CARTESIAN_POINT('Ctrl Pts',(1.51290740064448E-11,-111.029519323734,
8.40163766893887));
#19626=CARTESIAN_POINT('Ctrl Pts',(4.85068776981068,-110.854519323734,8.40163766893014));
#19627=CARTESIAN_POINT('Ctrl Pts',(7.2760316547009,-110.679519323734,4.20081883445634));
#19628=CARTESIAN_POINT('Ctrl Pts',(9.70137553959111,-110.504519323734,-1.74689558624962E-11));
#19629=CARTESIAN_POINT('Ctrl Pts',(7.27603165468577,-110.329519323734,-4.20081883448253));
#19630=CARTESIAN_POINT('Ctrl Pts',(4.85068776978043,-110.154519323734,-8.4016376689476));
#19631=CARTESIAN_POINT('Ctrl Pts',(-1.51301029103127E-11,-109.979519323734,
-8.40163766893887));
#19632=CARTESIAN_POINT('Ctrl Pts',(-4.85068776981069,-109.804519323734,
-8.40163766893014));
#19633=CARTESIAN_POINT('Ctrl Pts',(-7.2760316547009,-109.629519323734,-4.20081883445633));
#19634=CARTESIAN_POINT('Ctrl Pts',(-9.70137553959111,-109.454519323734,
1.74701439383464E-11));
#19635=CARTESIAN_POINT('Ctrl Pts',(-7.27603165468577,-109.279519323734,
4.20081883448254));
#19636=CARTESIAN_POINT('Ctrl Pts',(-4.85068776978043,-109.104519323734,
8.40163766894761));
#19637=CARTESIAN_POINT('Ctrl Pts',(1.51290740064448E-11,-108.929519323734,
8.40163766893887));
#19638=CARTESIAN_POINT('Ctrl Pts',(4.85068776981068,-108.754519323734,8.40163766893014));
#19639=CARTESIAN_POINT('Ctrl Pts',(7.2760316547009,-108.579519323734,4.20081883445634));
#19640=CARTESIAN_POINT('Ctrl Pts',(9.70137553959111,-108.404519323734,-1.74689558624962E-11));
#19641=CARTESIAN_POINT('Ctrl Pts',(7.27603165468577,-108.229519323734,-4.20081883448253));
#19642=CARTESIAN_POINT('Ctrl Pts',(4.85068776978043,-108.054519323734,-8.4016376689476));
#19643=CARTESIAN_POINT('Ctrl Pts',(-1.51301029103127E-11,-107.879519323734,
-8.40163766893887));
#19644=CARTESIAN_POINT('Ctrl Pts',(-4.85068776981069,-107.704519323734,
-8.40163766893014));
#19645=CARTESIAN_POINT('Ctrl Pts',(-7.2760316547009,-107.529519323734,-4.20081883445633));
#19646=CARTESIAN_POINT('Ctrl Pts',(-9.70137553959111,-107.354519323734,
1.74701439383464E-11));
#19647=CARTESIAN_POINT('Ctrl Pts',(-7.27603165468577,-107.179519323734,
4.20081883448254));
#19648=CARTESIAN_POINT('Ctrl Pts',(-4.85068776978043,-107.004519323734,
8.40163766894761));
#19649=CARTESIAN_POINT('Ctrl Pts',(1.51290740064448E-11,-106.829519323734,
8.40163766893887));
#19650=CARTESIAN_POINT('Ctrl Pts',(4.85068776981068,-106.654519323734,8.40163766893014));
#19651=CARTESIAN_POINT('Ctrl Pts',(7.2760316547009,-106.479519323734,4.20081883445634));
#19652=CARTESIAN_POINT('Ctrl Pts',(9.70137553959111,-106.304519323734,-1.74689558624962E-11));
#19653=CARTESIAN_POINT('Ctrl Pts',(7.27603165468577,-106.129519323734,-4.20081883448253));
#19654=CARTESIAN_POINT('Ctrl Pts',(4.85068776978043,-105.954519323734,-8.4016376689476));
#19655=CARTESIAN_POINT('Ctrl Pts',(-1.51301029103127E-11,-105.779519323734,
-8.40163766893887));
#19656=CARTESIAN_POINT('Ctrl Pts',(-4.85068776981069,-105.604519323734,
-8.40163766893014));
#19657=CARTESIAN_POINT('Ctrl Pts',(-7.2760316547009,-105.429519323734,-4.20081883445633));
#19658=CARTESIAN_POINT('Ctrl Pts',(-9.70137553959111,-105.254519323734,
1.74701439383464E-11));
#19659=CARTESIAN_POINT('Ctrl Pts',(-7.27603165468577,-105.079519323734,
4.20081883448254));
#19660=CARTESIAN_POINT('Ctrl Pts',(-4.85068776978043,-104.904519323734,
8.40163766894761));
#19661=CARTESIAN_POINT('Ctrl Pts',(1.51290740064448E-11,-104.729519323734,
8.40163766893887));
#19662=CARTESIAN_POINT('Ctrl Pts',(4.85068776981068,-104.554519323734,8.40163766893014));
#19663=CARTESIAN_POINT('Ctrl Pts',(7.2760316547009,-104.379519323734,4.20081883445634));
#19664=CARTESIAN_POINT('Ctrl Pts',(9.70137553959111,-104.204519323734,-1.74689558624962E-11));
#19665=CARTESIAN_POINT('Ctrl Pts',(7.27603165468577,-104.029519323734,-4.20081883448253));
#19666=CARTESIAN_POINT('Ctrl Pts',(4.85068776978043,-103.854519323734,-8.4016376689476));
#19667=CARTESIAN_POINT('Ctrl Pts',(-1.51301029103127E-11,-103.679519323734,
-8.40163766893887));
#19668=CARTESIAN_POINT('Ctrl Pts',(-4.85068776981069,-103.504519323734,
-8.40163766893014));
#19669=CARTESIAN_POINT('Ctrl Pts',(-7.2760316547009,-103.329519323734,-4.20081883445633));
#19670=CARTESIAN_POINT('Ctrl Pts',(-9.70137553959111,-103.154519323734,
1.74701439383464E-11));
#19671=CARTESIAN_POINT('Ctrl Pts',(-7.27603165468577,-102.979519323734,
4.20081883448254));
#19672=CARTESIAN_POINT('Ctrl Pts',(-4.85068776978043,-102.804519323734,
8.40163766894761));
#19673=CARTESIAN_POINT('Ctrl Pts',(1.51290740064448E-11,-102.629519323734,
8.40163766893887));
#19674=CARTESIAN_POINT('Ctrl Pts',(4.85068776981068,-102.454519323734,8.40163766893014));
#19675=CARTESIAN_POINT('Ctrl Pts',(7.2760316547009,-102.279519323734,4.20081883445634));
#19676=CARTESIAN_POINT('Ctrl Pts',(9.70137553959111,-102.104519323734,-1.74689558624962E-11));
#19677=CARTESIAN_POINT('Ctrl Pts',(7.27603165468577,-101.929519323734,-4.20081883448253));
#19678=CARTESIAN_POINT('Ctrl Pts',(4.85068776978043,-101.754519323734,-8.4016376689476));
#19679=CARTESIAN_POINT('Ctrl Pts',(-1.51301029103127E-11,-101.579519323734,
-8.40163766893887));
#19680=CARTESIAN_POINT('Ctrl Pts',(-4.85068776981069,-101.404519323734,
-8.40163766893014));
#19681=CARTESIAN_POINT('Ctrl Pts',(-7.2760316547009,-101.229519323734,-4.20081883445633));
#19682=CARTESIAN_POINT('Ctrl Pts',(-9.70137553959111,-101.054519323734,
1.74701439383464E-11));
#19683=CARTESIAN_POINT('Ctrl Pts',(-7.27603165468577,-100.879519323734,
4.20081883448254));
#19684=CARTESIAN_POINT('Ctrl Pts',(-4.85068776978043,-100.704519323734,
8.40163766894761));
#19685=CARTESIAN_POINT('Ctrl Pts',(1.51290740064448E-11,-100.529519323734,
8.40163766893887));
#19686=CARTESIAN_POINT('Ctrl Pts',(4.85068776981068,-100.354519323734,8.40163766893014));
#19687=CARTESIAN_POINT('Ctrl Pts',(7.2760316547009,-100.179519323734,4.20081883445634));
#19688=CARTESIAN_POINT('Ctrl Pts',(9.70137553959111,-100.004519323734,-1.74689558624962E-11));
#19689=CARTESIAN_POINT('Ctrl Pts',(7.27603165468577,-99.8295193237339,-4.20081883448253));
#19690=CARTESIAN_POINT('Ctrl Pts',(4.85068776978043,-99.6545193237339,-8.4016376689476));
#19691=CARTESIAN_POINT('Ctrl Pts',(-1.51301029103127E-11,-99.4795193237339,
-8.40163766893887));
#19692=CARTESIAN_POINT('Ctrl Pts',(-4.85068776981069,-99.3045193237339,
-8.40163766893014));
#19693=CARTESIAN_POINT('Ctrl Pts',(-7.2760316547009,-99.1295193237339,-4.20081883445633));
#19694=CARTESIAN_POINT('Ctrl Pts',(-9.70137553959111,-98.9545193237339,
1.74701439383464E-11));
#19695=CARTESIAN_POINT('Ctrl Pts',(-7.27603165468577,-98.7795193237339,
4.20081883448254));
#19696=CARTESIAN_POINT('Ctrl Pts',(-4.85068776978043,-98.6045193237339,
8.40163766894761));
#19697=CARTESIAN_POINT('Ctrl Pts',(1.51290740064448E-11,-98.4295193237339,
8.40163766893887));
#19698=CARTESIAN_POINT('Ctrl Pts',(4.85068776981068,-98.2545193237339,8.40163766893014));
#19699=CARTESIAN_POINT('Ctrl Pts',(7.2760316547009,-98.0795193237339,4.20081883445634));
#19700=CARTESIAN_POINT('Ctrl Pts',(9.70137553959111,-97.904519323734,-1.74689558624962E-11));
#19701=CARTESIAN_POINT('Ctrl Pts',(7.27603165468577,-97.7295193237339,-4.20081883448253));
#19702=CARTESIAN_POINT('Ctrl Pts',(4.85068776978043,-97.5545193237339,-8.4016376689476));
#19703=CARTESIAN_POINT('Ctrl Pts',(-1.51301029103127E-11,-97.3795193237339,
-8.40163766893887));
#19704=CARTESIAN_POINT('Ctrl Pts',(-4.85068776981069,-97.2045193237339,
-8.40163766893014));
#19705=CARTESIAN_POINT('Ctrl Pts',(-7.2760316547009,-97.0295193237339,-4.20081883445633));
#19706=CARTESIAN_POINT('Ctrl Pts',(-9.70137553959111,-96.8545193237339,
1.74701439383464E-11));
#19707=CARTESIAN_POINT('Ctrl Pts',(-7.27603165468577,-96.6795193237339,
4.20081883448254));
#19708=CARTESIAN_POINT('Ctrl Pts',(-4.85068776978043,-96.5045193237339,
8.40163766894761));
#19709=CARTESIAN_POINT('Ctrl Pts',(1.51290740064448E-11,-96.3295193237339,
8.40163766893887));
#19710=CARTESIAN_POINT('Ctrl Pts',(4.85068776981068,-96.1545193237339,8.40163766893014));
#19711=CARTESIAN_POINT('Ctrl Pts',(7.2760316547009,-95.9795193237339,4.20081883445634));
#19712=CARTESIAN_POINT('Ctrl Pts',(9.70137553959111,-95.804519323734,-1.74689558624962E-11));
#19713=CARTESIAN_POINT('Ctrl Pts',(7.27603165468577,-95.6295193237339,-4.20081883448253));
#19714=CARTESIAN_POINT('Ctrl Pts',(4.85068776978043,-95.4545193237339,-8.4016376689476));
#19715=CARTESIAN_POINT('Ctrl Pts',(-1.51301029103127E-11,-95.2795193237339,
-8.40163766893887));
#19716=CARTESIAN_POINT('Ctrl Pts',(-4.85068776981069,-95.1045193237339,
-8.40163766893014));
#19717=CARTESIAN_POINT('Ctrl Pts',(-7.2760316547009,-94.9295193237339,-4.20081883445633));
#19718=CARTESIAN_POINT('Ctrl Pts',(-9.70137553959111,-94.7545193237339,
1.74701439383464E-11));
#19719=CARTESIAN_POINT('Ctrl Pts',(-7.27603165468577,-94.5795193237339,
4.20081883448254));
#19720=CARTESIAN_POINT('Ctrl Pts',(-4.85068776978043,-94.4045193237339,
8.40163766894761));
#19721=CARTESIAN_POINT('Ctrl Pts',(1.51290740064448E-11,-94.2295193237339,
8.40163766893887));
#19722=CARTESIAN_POINT('Ctrl Pts',(4.85068776981068,-94.0545193237339,8.40163766893014));
#19723=CARTESIAN_POINT('Ctrl Pts',(7.2760316547009,-93.8795193237339,4.20081883445634));
#19724=CARTESIAN_POINT('Ctrl Pts',(9.70137553959111,-93.7045193237339,-1.74689558624962E-11));
#19725=CARTESIAN_POINT('Ctrl Pts',(7.27603165468577,-93.5295193237339,-4.20081883448253));
#19726=CARTESIAN_POINT('Ctrl Pts',(4.85068776978043,-93.3545193237339,-8.4016376689476));
#19727=CARTESIAN_POINT('Ctrl Pts',(-1.51301029103127E-11,-93.1795193237339,
-8.40163766893887));
#19728=CARTESIAN_POINT('Ctrl Pts',(-4.85068776981069,-93.0045193237339,
-8.40163766893014));
#19729=CARTESIAN_POINT('Ctrl Pts',(-7.2760316547009,-92.8295193237339,-4.20081883445633));
#19730=CARTESIAN_POINT('Ctrl Pts',(-9.70137553959111,-92.6545193237339,
1.74701439383464E-11));
#19731=CARTESIAN_POINT('Ctrl Pts',(-7.27603165468577,-92.4795193237339,
4.20081883448254));
#19732=CARTESIAN_POINT('Ctrl Pts',(-4.85068776978043,-92.3045193237339,
8.40163766894761));
#19733=CARTESIAN_POINT('Ctrl Pts',(1.51290740064448E-11,-92.1295193237339,
8.40163766893887));
#19734=CARTESIAN_POINT('Ctrl Pts',(4.85068776981068,-91.9545193237339,8.40163766893014));
#19735=CARTESIAN_POINT('Ctrl Pts',(7.2760316547009,-91.7795193237339,4.20081883445634));
#19736=CARTESIAN_POINT('Ctrl Pts',(9.70137553959111,-91.6045193237339,-1.74689558624962E-11));
#19737=CARTESIAN_POINT('Ctrl Pts',(7.27603165468577,-91.4295193237339,-4.20081883448253));
#19738=CARTESIAN_POINT('Ctrl Pts',(4.85068776978043,-91.2545193237339,-8.4016376689476));
#19739=CARTESIAN_POINT('Ctrl Pts',(-1.51301029103127E-11,-91.0795193237339,
-8.40163766893887));
#19740=CARTESIAN_POINT('Ctrl Pts',(-4.85068776981069,-90.9045193237339,
-8.40163766893014));
#19741=CARTESIAN_POINT('Ctrl Pts',(-7.2760316547009,-90.7295193237339,-4.20081883445633));
#19742=CARTESIAN_POINT('Ctrl Pts',(-9.70137553959111,-90.5545193237339,
1.74701439383464E-11));
#19743=CARTESIAN_POINT('Ctrl Pts',(-7.27603165468577,-90.3795193237339,
4.20081883448254));
#19744=CARTESIAN_POINT('Ctrl Pts',(-4.85068776978043,-90.2045193237339,
8.40163766894761));
#19745=CARTESIAN_POINT('Ctrl Pts',(1.51290740064448E-11,-90.0295193237339,
8.40163766893887));
#19746=CARTESIAN_POINT('Ctrl Pts',(4.85068776981068,-89.8545193237339,8.40163766893014));
#19747=CARTESIAN_POINT('Ctrl Pts',(7.2760316547009,-89.6795193237339,4.20081883445634));
#19748=CARTESIAN_POINT('Ctrl Pts',(9.70137553959111,-89.5045193237339,-1.74689558624962E-11));
#19749=CARTESIAN_POINT('Ctrl Pts',(7.27603165468577,-89.3295193237339,-4.20081883448253));
#19750=CARTESIAN_POINT('Ctrl Pts',(4.85068776978043,-89.154519323734,-8.4016376689476));
#19751=CARTESIAN_POINT('Ctrl Pts',(-1.51301029103127E-11,-88.9795193237339,
-8.40163766893887));
#19752=CARTESIAN_POINT('Ctrl Pts',(-4.85068776981069,-88.8045193237339,
-8.40163766893014));
#19753=CARTESIAN_POINT('Ctrl Pts',(-7.2760316547009,-88.6295193237339,-4.20081883445633));
#19754=CARTESIAN_POINT('Ctrl Pts',(-9.70137553959111,-88.4545193237339,
1.74701439383464E-11));
#19755=CARTESIAN_POINT('Ctrl Pts',(-7.27603165468577,-88.2795193237339,
4.20081883448254));
#19756=CARTESIAN_POINT('Ctrl Pts',(-4.85068776978043,-88.104519323734,8.40163766894761));
#19757=CARTESIAN_POINT('Ctrl Pts',(1.51290740064448E-11,-87.9295193237339,
8.40163766893887));
#19758=CARTESIAN_POINT('Ctrl Pts',(4.85068776981068,-87.7545193237339,8.40163766893014));
#19759=CARTESIAN_POINT('Ctrl Pts',(7.2760316547009,-87.5795193237339,4.20081883445634));
#19760=CARTESIAN_POINT('Ctrl Pts',(9.70137553959111,-87.404519323734,-1.74689558624962E-11));
#19761=CARTESIAN_POINT('Ctrl Pts',(7.27603165468577,-87.2295193237339,-4.20081883448253));
#19762=CARTESIAN_POINT('Ctrl Pts',(4.85068776978043,-87.054519323734,-8.4016376689476));
#19763=CARTESIAN_POINT('Ctrl Pts',(-1.51301029103127E-11,-86.8795193237339,
-8.40163766893887));
#19764=CARTESIAN_POINT('Ctrl Pts',(-4.85068776981069,-86.7045193237339,
-8.40163766893014));
#19765=CARTESIAN_POINT('Ctrl Pts',(-7.2760316547009,-86.529519323734,-4.20081883445633));
#19766=CARTESIAN_POINT('Ctrl Pts',(-9.70137553959111,-86.3545193237339,
1.74701439383464E-11));
#19767=CARTESIAN_POINT('Ctrl Pts',(-7.27603165468577,-86.1795193237339,
4.20081883448254));
#19768=CARTESIAN_POINT('Ctrl Pts',(-4.85068776978043,-86.0045193237339,
8.40163766894761));
#19769=CARTESIAN_POINT('Ctrl Pts',(1.51290740064448E-11,-85.8295193237339,
8.40163766893887));
#19770=CARTESIAN_POINT('Ctrl Pts',(4.85068776981068,-85.6545193237339,8.40163766893014));
#19771=CARTESIAN_POINT('Ctrl Pts',(7.2760316547009,-85.4795193237339,4.20081883445634));
#19772=CARTESIAN_POINT('Ctrl Pts',(9.70137553959111,-85.3045193237339,-1.74689558624962E-11));
#19773=CARTESIAN_POINT('Ctrl Pts',(7.27603165468577,-85.1295193237339,-4.20081883448253));
#19774=CARTESIAN_POINT('Ctrl Pts',(4.85068776978043,-84.9545193237339,-8.4016376689476));
#19775=CARTESIAN_POINT('Ctrl Pts',(-1.51301029103127E-11,-84.7795193237339,
-8.40163766893887));
#19776=CARTESIAN_POINT('Ctrl Pts',(-4.85068776981069,-84.604519323734,-8.40163766893014));
#19777=CARTESIAN_POINT('Ctrl Pts',(-7.2760316547009,-84.4295193237339,-4.20081883445633));
#19778=CARTESIAN_POINT('Ctrl Pts',(-9.70137553959111,-84.2545193237339,
1.74701439383464E-11));
#19779=CARTESIAN_POINT('Ctrl Pts',(-7.27603165468577,-84.0795193237339,
4.20081883448254));
#19780=CARTESIAN_POINT('Ctrl Pts',(-4.85068776978043,-83.9045193237339,
8.40163766894761));
#19781=CARTESIAN_POINT('Ctrl Pts',(1.51290740064448E-11,-83.7295193237339,
8.40163766893887));
#19782=CARTESIAN_POINT('Ctrl Pts',(4.85068776981068,-83.554519323734,8.40163766893014));
#19783=CARTESIAN_POINT('Ctrl Pts',(7.2760316547009,-83.3795193237339,4.20081883445634));
#19784=CARTESIAN_POINT('Ctrl Pts',(9.70137553959111,-83.2045193237339,-1.74689558624962E-11));
#19785=CARTESIAN_POINT('Ctrl Pts',(7.27603165468577,-83.029519323734,-4.20081883448253));
#19786=CARTESIAN_POINT('Ctrl Pts',(4.85068776978043,-82.8545193237339,-8.4016376689476));
#19787=CARTESIAN_POINT('Ctrl Pts',(-1.51301029103127E-11,-82.6795193237339,
-8.40163766893887));
#19788=CARTESIAN_POINT('Ctrl Pts',(-4.85068776981069,-82.504519323734,-8.40163766893014));
#19789=CARTESIAN_POINT('Ctrl Pts',(-7.2760316547009,-82.3295193237339,-4.20081883445633));
#19790=CARTESIAN_POINT('Ctrl Pts',(-9.70137553959111,-82.154519323734,1.74701439383464E-11));
#19791=CARTESIAN_POINT('Ctrl Pts',(-7.27603165468577,-81.9795193237339,
4.20081883448254));
#19792=CARTESIAN_POINT('Ctrl Pts',(-4.85068776978043,-81.8045193237339,
8.40163766894761));
#19793=CARTESIAN_POINT('Ctrl Pts',(1.51290740064448E-11,-81.6295193237339,
8.40163766893887));
#19794=CARTESIAN_POINT('Ctrl Pts',(4.85068776981068,-81.454519323734,8.40163766893014));
#19795=CARTESIAN_POINT('Ctrl Pts',(7.2760316547009,-81.2795193237339,4.20081883445634));
#19796=CARTESIAN_POINT('Ctrl Pts',(9.70137553959111,-81.1045193237339,-1.74689558624962E-11));
#19797=CARTESIAN_POINT('Ctrl Pts',(7.27603165468577,-80.929519323734,-4.20081883448253));
#19798=CARTESIAN_POINT('Ctrl Pts',(4.85068776978043,-80.754519323734,-8.4016376689476));
#19799=CARTESIAN_POINT('Ctrl Pts',(-1.51301029103127E-11,-80.5795193237339,
-8.40163766893887));
#19800=CARTESIAN_POINT('Ctrl Pts',(-4.85068776981069,-80.404519323734,-8.40163766893014));
#19801=CARTESIAN_POINT('Ctrl Pts',(-7.2760316547009,-80.2295193237339,-4.20081883445633));
#19802=CARTESIAN_POINT('Ctrl Pts',(-9.70137553959111,-80.054519323734,1.74701439383464E-11));
#19803=CARTESIAN_POINT('Ctrl Pts',(-7.27603165468577,-79.879519323734,4.20081883448254));
#19804=CARTESIAN_POINT('Ctrl Pts',(-4.85068776978043,-79.7045193237339,
8.40163766894761));
#19805=CARTESIAN_POINT('Ctrl Pts',(1.51290740064448E-11,-79.5295193237339,
8.40163766893887));
#19806=CARTESIAN_POINT('Ctrl Pts',(4.85068776981068,-79.354519323734,8.40163766893014));
#19807=CARTESIAN_POINT('Ctrl Pts',(7.2760316547009,-79.179519323734,4.20081883445634));
#19808=CARTESIAN_POINT('Ctrl Pts',(9.70137553959111,-79.0045193237339,-1.74689558624962E-11));
#19809=CARTESIAN_POINT('Ctrl Pts',(7.27603165468577,-78.829519323734,-4.20081883448253));
#19810=CARTESIAN_POINT('Ctrl Pts',(4.85068776978043,-78.654519323734,-8.4016376689476));
#19811=CARTESIAN_POINT('Ctrl Pts',(-1.51301029103127E-11,-78.4795193237339,
-8.40163766893887));
#19812=CARTESIAN_POINT('Ctrl Pts',(-4.85068776981069,-78.304519323734,-8.40163766893014));
#19813=CARTESIAN_POINT('Ctrl Pts',(-7.2760316547009,-78.129519323734,-4.20081883445633));
#19814=CARTESIAN_POINT('Ctrl Pts',(-9.70137553959111,-77.954519323734,1.74701439383464E-11));
#19815=CARTESIAN_POINT('Ctrl Pts',(-7.27603165468577,-77.779519323734,4.20081883448254));
#19816=CARTESIAN_POINT('Ctrl Pts',(-4.85068776978043,-77.604519323734,8.40163766894761));
#19817=CARTESIAN_POINT('Ctrl Pts',(1.51290740064448E-11,-77.4295193237339,
8.40163766893887));
#19818=CARTESIAN_POINT('Ctrl Pts',(4.85068776981068,-77.254519323734,8.40163766893014));
#19819=CARTESIAN_POINT('Ctrl Pts',(7.2760316547009,-77.0795193237339,4.20081883445634));
#19820=CARTESIAN_POINT('Ctrl Pts',(9.70137553959111,-76.904519323734,-1.74689558624962E-11));
#19821=CARTESIAN_POINT('Ctrl Pts',(7.27603165468577,-76.729519323734,-4.20081883448253));
#19822=CARTESIAN_POINT('Ctrl Pts',(4.85068776978043,-76.5545193237339,-8.4016376689476));
#19823=CARTESIAN_POINT('Ctrl Pts',(-1.51301029103127E-11,-76.379519323734,
-8.40163766893887));
#19824=CARTESIAN_POINT('Ctrl Pts',(-4.85068776981069,-76.204519323734,-8.40163766893014));
#19825=CARTESIAN_POINT('Ctrl Pts',(-7.2760316547009,-76.0295193237339,-4.20081883445633));
#19826=CARTESIAN_POINT('Ctrl Pts',(-9.70137553959111,-75.854519323734,1.74701439383464E-11));
#19827=CARTESIAN_POINT('Ctrl Pts',(-7.27603165468577,-75.679519323734,4.20081883448254));
#19828=CARTESIAN_POINT('Ctrl Pts',(-4.85068776978043,-75.5045193237339,
8.40163766894761));
#19829=CARTESIAN_POINT('Ctrl Pts',(1.51290740064448E-11,-75.329519323734,
8.40163766893887));
#19830=CARTESIAN_POINT('Ctrl Pts',(4.85068776981068,-75.1545193237339,8.40163766893014));
#19831=CARTESIAN_POINT('Ctrl Pts',(7.2760316547009,-74.9795193237339,4.20081883445634));
#19832=CARTESIAN_POINT('Ctrl Pts',(9.70137553959111,-74.804519323734,-1.74689558624962E-11));
#19833=CARTESIAN_POINT('Ctrl Pts',(7.27603165468577,-74.6295193237339,-4.20081883448253));
#19834=CARTESIAN_POINT('Ctrl Pts',(4.85068776978043,-74.454519323734,-8.4016376689476));
#19835=CARTESIAN_POINT('Ctrl Pts',(-1.51301029103127E-11,-74.279519323734,
-8.40163766893887));
#19836=CARTESIAN_POINT('Ctrl Pts',(-4.85068776981069,-74.104519323734,-8.40163766893014));
#19837=CARTESIAN_POINT('Ctrl Pts',(-7.2760316547009,-73.9295193237339,-4.20081883445633));
#19838=CARTESIAN_POINT('Ctrl Pts',(-9.70137553959111,-73.754519323734,1.74701439383464E-11));
#19839=CARTESIAN_POINT('Ctrl Pts',(-7.27603165468577,-73.579519323734,4.20081883448254));
#19840=CARTESIAN_POINT('Ctrl Pts',(-4.85068776978043,-73.404519323734,8.40163766894761));
#19841=CARTESIAN_POINT('Ctrl Pts',(1.51290740064448E-11,-73.229519323734,
8.40163766893887));
#19842=CARTESIAN_POINT('Ctrl Pts',(4.85068776981068,-73.054519323734,8.40163766893014));
#19843=CARTESIAN_POINT('Ctrl Pts',(7.2760316547009,-72.8795193237339,4.20081883445634));
#19844=CARTESIAN_POINT('Ctrl Pts',(9.70137553959111,-72.704519323734,-1.74689558624962E-11));
#19845=CARTESIAN_POINT('Ctrl Pts',(7.27603165468577,-72.529519323734,-4.20081883448253));
#19846=CARTESIAN_POINT('Ctrl Pts',(4.85068776978043,-72.354519323734,-8.4016376689476));
#19847=CARTESIAN_POINT('Ctrl Pts',(-1.51301029103127E-11,-72.179519323734,
-8.40163766893887));
#19848=CARTESIAN_POINT('Ctrl Pts',(-4.85068776981069,-72.004519323734,-8.40163766893014));
#19849=CARTESIAN_POINT('Ctrl Pts',(-7.2760316547009,-71.829519323734,-4.20081883445633));
#19850=CARTESIAN_POINT('Ctrl Pts',(-9.70137553959111,-71.654519323734,1.74701439383464E-11));
#19851=CARTESIAN_POINT('Ctrl Pts',(-7.27603165468577,-71.479519323734,4.20081883448254));
#19852=CARTESIAN_POINT('Ctrl Pts',(-4.85068776978043,-71.304519323734,8.40163766894761));
#19853=CARTESIAN_POINT('Ctrl Pts',(1.51290740064448E-11,-71.129519323734,
8.40163766893887));
#19854=CARTESIAN_POINT('Ctrl Pts',(4.85068776981068,-70.954519323734,8.40163766893014));
#19855=CARTESIAN_POINT('Ctrl Pts',(7.2760316547009,-70.779519323734,4.20081883445634));
#19856=CARTESIAN_POINT('Ctrl Pts',(9.70137553959111,-70.604519323734,-1.74689558624962E-11));
#19857=CARTESIAN_POINT('Ctrl Pts',(7.27603165468577,-70.429519323734,-4.20081883448253));
#19858=CARTESIAN_POINT('Ctrl Pts',(4.85068776978043,-70.254519323734,-8.4016376689476));
#19859=CARTESIAN_POINT('Ctrl Pts',(-1.51301029103127E-11,-70.079519323734,
-8.40163766893887));
#19860=CARTESIAN_POINT('Ctrl Pts',(-4.85068776981069,-69.904519323734,-8.40163766893014));
#19861=CARTESIAN_POINT('Ctrl Pts',(-7.2760316547009,-69.729519323734,-4.20081883445633));
#19862=CARTESIAN_POINT('Ctrl Pts',(-9.70137553959111,-69.554519323734,1.74701439383464E-11));
#19863=CARTESIAN_POINT('Ctrl Pts',(-7.27603165468577,-69.379519323734,4.20081883448254));
#19864=CARTESIAN_POINT('Ctrl Pts',(-4.85068776978043,-69.204519323734,8.40163766894761));
#19865=CARTESIAN_POINT('Ctrl Pts',(1.51290740064448E-11,-69.029519323734,
8.40163766893887));
#19866=CARTESIAN_POINT('Ctrl Pts',(4.85068776981068,-68.854519323734,8.40163766893014));
#19867=CARTESIAN_POINT('Ctrl Pts',(7.2760316547009,-68.679519323734,4.20081883445634));
#19868=CARTESIAN_POINT('Ctrl Pts',(9.70137553959111,-68.504519323734,-1.74689558624962E-11));
#19869=CARTESIAN_POINT('Ctrl Pts',(7.27603165468577,-68.3295193237339,-4.20081883448253));
#19870=CARTESIAN_POINT('Ctrl Pts',(4.85068776978043,-68.154519323734,-8.4016376689476));
#19871=CARTESIAN_POINT('Ctrl Pts',(-1.51301029103127E-11,-67.979519323734,
-8.40163766893887));
#19872=CARTESIAN_POINT('Ctrl Pts',(-4.85068776981069,-67.804519323734,-8.40163766893014));
#19873=CARTESIAN_POINT('Ctrl Pts',(-7.2760316547009,-67.629519323734,-4.20081883445633));
#19874=CARTESIAN_POINT('Ctrl Pts',(-9.70137553959111,-67.454519323734,1.74701439383464E-11));
#19875=CARTESIAN_POINT('Ctrl Pts',(-7.27603165468577,-67.279519323734,4.20081883448254));
#19876=CARTESIAN_POINT('Ctrl Pts',(-4.85068776978043,-67.104519323734,8.40163766894761));
#19877=CARTESIAN_POINT('Ctrl Pts',(1.51290740064448E-11,-66.929519323734,
8.40163766893887));
#19878=CARTESIAN_POINT('Ctrl Pts',(4.85068776981068,-66.754519323734,8.40163766893014));
#19879=CARTESIAN_POINT('Ctrl Pts',(7.2760316547009,-66.579519323734,4.20081883445634));
#19880=CARTESIAN_POINT('Ctrl Pts',(9.70137553959111,-66.404519323734,-1.74689558624962E-11));
#19881=CARTESIAN_POINT('Ctrl Pts',(7.27603165468577,-66.229519323734,-4.20081883448253));
#19882=CARTESIAN_POINT('Ctrl Pts',(4.85068776978043,-66.054519323734,-8.4016376689476));
#19883=CARTESIAN_POINT('Ctrl Pts',(-1.51301029103127E-11,-65.879519323734,
-8.40163766893887));
#19884=CARTESIAN_POINT('Ctrl Pts',(-4.85068776981069,-65.704519323734,-8.40163766893014));
#19885=CARTESIAN_POINT('Ctrl Pts',(-7.2760316547009,-65.529519323734,-4.20081883445633));
#19886=CARTESIAN_POINT('Ctrl Pts',(-9.70137553959111,-65.354519323734,1.74701439383464E-11));
#19887=CARTESIAN_POINT('Ctrl Pts',(-7.27603165468577,-65.179519323734,4.20081883448254));
#19888=CARTESIAN_POINT('Ctrl Pts',(-4.85068776978043,-65.004519323734,8.40163766894761));
#19889=CARTESIAN_POINT('Ctrl Pts',(1.51290740064448E-11,-64.829519323734,
8.40163766893887));
#19890=CARTESIAN_POINT('Ctrl Pts',(4.85068776981068,-64.654519323734,8.40163766893014));
#19891=CARTESIAN_POINT('Ctrl Pts',(7.2760316547009,-64.479519323734,4.20081883445634));
#19892=CARTESIAN_POINT('Ctrl Pts',(9.70137553959111,-64.304519323734,-1.74689558624962E-11));
#19893=CARTESIAN_POINT('Ctrl Pts',(7.27603165468577,-64.129519323734,-4.20081883448253));
#19894=CARTESIAN_POINT('Ctrl Pts',(4.85068776978043,-63.954519323734,-8.4016376689476));
#19895=CARTESIAN_POINT('Ctrl Pts',(-1.51301029103127E-11,-63.779519323734,
-8.40163766893887));
#19896=CARTESIAN_POINT('Ctrl Pts',(-4.85068776981069,-63.604519323734,-8.40163766893014));
#19897=CARTESIAN_POINT('Ctrl Pts',(-7.2760316547009,-63.429519323734,-4.20081883445633));
#19898=CARTESIAN_POINT('Ctrl Pts',(-9.70137553959111,-63.254519323734,1.74701439383464E-11));
#19899=CARTESIAN_POINT('Ctrl Pts',(-7.27603165468577,-63.079519323734,4.20081883448254));
#19900=CARTESIAN_POINT('Ctrl Pts',(-4.85068776978043,-62.904519323734,8.40163766894761));
#19901=CARTESIAN_POINT('Ctrl Pts',(1.51290740064448E-11,-62.729519323734,
8.40163766893887));
#19902=CARTESIAN_POINT('Ctrl Pts',(4.85068776981068,-62.554519323734,8.40163766893014));
#19903=CARTESIAN_POINT('Ctrl Pts',(7.2760316547009,-62.379519323734,4.20081883445634));
#19904=CARTESIAN_POINT('Ctrl Pts',(9.70137553959111,-62.204519323734,-1.74689558624962E-11));
#19905=CARTESIAN_POINT('Ctrl Pts',(7.27603165468577,-62.029519323734,-4.20081883448253));
#19906=CARTESIAN_POINT('Ctrl Pts',(4.85068776978043,-61.854519323734,-8.4016376689476));
#19907=CARTESIAN_POINT('Ctrl Pts',(-1.51301029103127E-11,-61.679519323734,
-8.40163766893887));
#19908=CARTESIAN_POINT('Ctrl Pts',(-4.85068776981069,-61.504519323734,-8.40163766893014));
#19909=CARTESIAN_POINT('Ctrl Pts',(-7.2760316547009,-61.329519323734,-4.20081883445633));
#19910=CARTESIAN_POINT('Ctrl Pts',(-9.70137553959111,-61.154519323734,1.74701439383464E-11));
#19911=CARTESIAN_POINT('Ctrl Pts',(-7.27603165468577,-60.979519323734,4.20081883448254));
#19912=CARTESIAN_POINT('Ctrl Pts',(-4.85068776978043,-60.804519323734,8.40163766894761));
#19913=CARTESIAN_POINT('Ctrl Pts',(1.51290740064448E-11,-60.629519323734,
8.40163766893887));
#19914=CARTESIAN_POINT('Ctrl Pts',(4.85068776981068,-60.454519323734,8.40163766893014));
#19915=CARTESIAN_POINT('Ctrl Pts',(7.2760316547009,-60.279519323734,4.20081883445634));
#19916=CARTESIAN_POINT('Ctrl Pts',(9.70137553959111,-60.104519323734,-1.74689558624962E-11));
#19917=CARTESIAN_POINT('Ctrl Pts',(7.27603165468577,-59.929519323734,-4.20081883448253));
#19918=CARTESIAN_POINT('Ctrl Pts',(4.85068776978043,-59.754519323734,-8.4016376689476));
#19919=CARTESIAN_POINT('Ctrl Pts',(-1.51301029103127E-11,-59.579519323734,
-8.40163766893887));
#19920=CARTESIAN_POINT('Ctrl Pts',(-4.85068776981069,-59.404519323734,-8.40163766893014));
#19921=CARTESIAN_POINT('Ctrl Pts',(-7.2760316547009,-59.229519323734,-4.20081883445633));
#19922=CARTESIAN_POINT('Ctrl Pts',(-9.70137553959111,-59.054519323734,1.74701439383464E-11));
#19923=CARTESIAN_POINT('Ctrl Pts',(-7.27603165468577,-58.879519323734,4.20081883448254));
#19924=CARTESIAN_POINT('Ctrl Pts',(-4.85068776978043,-58.704519323734,8.40163766894761));
#19925=CARTESIAN_POINT('Ctrl Pts',(1.51290740064448E-11,-58.529519323734,
8.40163766893887));
#19926=CARTESIAN_POINT('Ctrl Pts',(4.85068776981068,-58.354519323734,8.40163766893014));
#19927=CARTESIAN_POINT('Ctrl Pts',(7.2760316547009,-58.179519323734,4.20081883445634));
#19928=CARTESIAN_POINT('Ctrl Pts',(9.70137553959111,-58.004519323734,-1.74689558624962E-11));
#19929=CARTESIAN_POINT('Ctrl Pts',(7.27603165468577,-57.829519323734,-4.20081883448253));
#19930=CARTESIAN_POINT('Ctrl Pts',(4.85068776978043,-57.654519323734,-8.4016376689476));
#19931=CARTESIAN_POINT('Ctrl Pts',(-1.51301029103127E-11,-57.479519323734,
-8.40163766893887));
#19932=CARTESIAN_POINT('Ctrl Pts',(-4.85068776981069,-57.304519323734,-8.40163766893014));
#19933=CARTESIAN_POINT('Ctrl Pts',(-7.2760316547009,-57.129519323734,-4.20081883445633));
#19934=CARTESIAN_POINT('Ctrl Pts',(-9.70137553959111,-56.954519323734,1.74701439383464E-11));
#19935=CARTESIAN_POINT('Ctrl Pts',(-7.27603165468577,-56.779519323734,4.20081883448254));
#19936=CARTESIAN_POINT('Ctrl Pts',(-4.85068776978043,-56.604519323734,8.40163766894761));
#19937=CARTESIAN_POINT('Ctrl Pts',(1.51290740064448E-11,-56.429519323734,
8.40163766893887));
#19938=CARTESIAN_POINT('Ctrl Pts',(4.85068776981068,-56.254519323734,8.40163766893014));
#19939=CARTESIAN_POINT('Ctrl Pts',(7.2760316547009,-56.079519323734,4.20081883445634));
#19940=CARTESIAN_POINT('Ctrl Pts',(9.70137553959111,-55.904519323734,-1.74689558624962E-11));
#19941=CARTESIAN_POINT('Ctrl Pts',(7.27603165468577,-55.729519323734,-4.20081883448253));
#19942=CARTESIAN_POINT('Ctrl Pts',(4.85068776978043,-55.554519323734,-8.4016376689476));
#19943=CARTESIAN_POINT('Ctrl Pts',(-1.51301029103127E-11,-55.379519323734,
-8.40163766893887));
#19944=CARTESIAN_POINT('Ctrl Pts',(-4.85068776981069,-55.204519323734,-8.40163766893014));
#19945=CARTESIAN_POINT('Ctrl Pts',(-7.2760316547009,-55.029519323734,-4.20081883445633));
#19946=CARTESIAN_POINT('Ctrl Pts',(-9.70137553959111,-54.854519323734,1.74701439383464E-11));
#19947=CARTESIAN_POINT('Ctrl Pts',(-7.27603165468577,-54.679519323734,4.20081883448254));
#19948=CARTESIAN_POINT('Ctrl Pts',(-4.85068776978043,-54.504519323734,8.40163766894761));
#19949=CARTESIAN_POINT('Ctrl Pts',(1.51290740064448E-11,-54.329519323734,
8.40163766893887));
#19950=CARTESIAN_POINT('Ctrl Pts',(4.85068776981068,-54.154519323734,8.40163766893014));
#19951=CARTESIAN_POINT('Ctrl Pts',(7.2760316547009,-53.979519323734,4.20081883445634));
#19952=CARTESIAN_POINT('Ctrl Pts',(9.70137553959111,-53.804519323734,-1.74689558624962E-11));
#19953=CARTESIAN_POINT('Ctrl Pts',(7.27603165468577,-53.629519323734,-4.20081883448253));
#19954=CARTESIAN_POINT('Ctrl Pts',(4.85068776978043,-53.454519323734,-8.4016376689476));
#19955=CARTESIAN_POINT('Ctrl Pts',(-1.51301029103127E-11,-53.279519323734,
-8.40163766893887));
#19956=CARTESIAN_POINT('Ctrl Pts',(-4.85068776981069,-53.104519323734,-8.40163766893014));
#19957=CARTESIAN_POINT('Ctrl Pts',(-7.2760316547009,-52.929519323734,-4.20081883445633));
#19958=CARTESIAN_POINT('Ctrl Pts',(-9.70137553959111,-52.754519323734,1.74701439383464E-11));
#19959=CARTESIAN_POINT('Ctrl Pts',(-7.27603165468577,-52.579519323734,4.20081883448254));
#19960=CARTESIAN_POINT('Ctrl Pts',(-4.85068776978043,-52.404519323734,8.40163766894761));
#19961=CARTESIAN_POINT('Ctrl Pts',(1.51290740064448E-11,-52.229519323734,
8.40163766893887));
#19962=CARTESIAN_POINT('Ctrl Pts',(4.85068776981068,-52.054519323734,8.40163766893014));
#19963=CARTESIAN_POINT('Ctrl Pts',(7.2760316547009,-51.879519323734,4.20081883445634));
#19964=CARTESIAN_POINT('Ctrl Pts',(9.70137553959111,-51.704519323734,-1.74689558624962E-11));
#19965=CARTESIAN_POINT('Ctrl Pts',(7.27603165468577,-51.529519323734,-4.20081883448253));
#19966=CARTESIAN_POINT('Ctrl Pts',(4.85068776978043,-51.354519323734,-8.4016376689476));
#19967=CARTESIAN_POINT('Ctrl Pts',(-1.51301029103127E-11,-51.179519323734,
-8.40163766893887));
#19968=CARTESIAN_POINT('Ctrl Pts',(-4.85068776981069,-51.004519323734,-8.40163766893014));
#19969=CARTESIAN_POINT('Ctrl Pts',(-7.2760316547009,-50.829519323734,-4.20081883445633));
#19970=CARTESIAN_POINT('Ctrl Pts',(-9.70137553959111,-50.654519323734,1.74701439383464E-11));
#19971=CARTESIAN_POINT('Ctrl Pts',(-7.27603165468577,-50.479519323734,4.20081883448254));
#19972=CARTESIAN_POINT('Ctrl Pts',(-4.85068776978043,-50.304519323734,8.40163766894761));
#19973=CARTESIAN_POINT('Ctrl Pts',(1.51290740064448E-11,-50.129519323734,
8.40163766893887));
#19974=CARTESIAN_POINT('Ctrl Pts',(4.85068776981068,-49.954519323734,8.40163766893014));
#19975=CARTESIAN_POINT('Ctrl Pts',(7.2760316547009,-49.779519323734,4.20081883445634));
#19976=CARTESIAN_POINT('Ctrl Pts',(9.70137553959111,-49.604519323734,-1.74689558624962E-11));
#19977=CARTESIAN_POINT('Ctrl Pts',(7.27603165468577,-49.429519323734,-4.20081883448253));
#19978=CARTESIAN_POINT('Ctrl Pts',(4.85068776978043,-49.254519323734,-8.4016376689476));
#19979=CARTESIAN_POINT('Ctrl Pts',(-1.51301029103127E-11,-49.079519323734,
-8.40163766893887));
#19980=CARTESIAN_POINT('Ctrl Pts',(-4.85068776981069,-48.904519323734,-8.40163766893014));
#19981=CARTESIAN_POINT('Ctrl Pts',(-7.2760316547009,-48.729519323734,-4.20081883445633));
#19982=CARTESIAN_POINT('Ctrl Pts',(-9.70137553959111,-48.554519323734,1.74701439383464E-11));
#19983=CARTESIAN_POINT('Ctrl Pts',(-7.27603165468577,-48.379519323734,4.20081883448254));
#19984=CARTESIAN_POINT('Ctrl Pts',(-4.85068776978043,-48.204519323734,8.40163766894761));
#19985=CARTESIAN_POINT('Ctrl Pts',(1.51290740064448E-11,-48.029519323734,
8.40163766893887));
#19986=CARTESIAN_POINT('Ctrl Pts',(4.85068776981068,-47.854519323734,8.40163766893014));
#19987=CARTESIAN_POINT('Ctrl Pts',(7.2760316547009,-47.679519323734,4.20081883445634));
#19988=CARTESIAN_POINT('Ctrl Pts',(9.70137553959111,-47.5045193237341,-1.74689558624962E-11));
#19989=CARTESIAN_POINT('Ctrl Pts',(7.27603165468577,-47.329519323734,-4.20081883448253));
#19990=CARTESIAN_POINT('Ctrl Pts',(4.85068776978043,-47.154519323734,-8.4016376689476));
#19991=CARTESIAN_POINT('Ctrl Pts',(-1.51301029103127E-11,-46.979519323734,
-8.40163766893887));
#19992=CARTESIAN_POINT('Ctrl Pts',(-4.85068776981069,-46.804519323734,-8.40163766893014));
#19993=CARTESIAN_POINT('Ctrl Pts',(-7.2760316547009,-46.629519323734,-4.20081883445633));
#19994=CARTESIAN_POINT('Ctrl Pts',(-9.70137553959111,-46.454519323734,1.74701439383464E-11));
#19995=CARTESIAN_POINT('Ctrl Pts',(-7.27603165468577,-46.279519323734,4.20081883448254));
#19996=CARTESIAN_POINT('Ctrl Pts',(-4.85068776978043,-46.104519323734,8.40163766894761));
#19997=CARTESIAN_POINT('Ctrl Pts',(1.51290740064448E-11,-45.929519323734,
8.40163766893887));
#19998=CARTESIAN_POINT('Ctrl Pts',(4.85068776981068,-45.754519323734,8.40163766893014));
#19999=CARTESIAN_POINT('Ctrl Pts',(7.2760316547009,-45.579519323734,4.20081883445634));
#20000=CARTESIAN_POINT('Ctrl Pts',(9.70137553959111,-45.404519323734,-1.74689558624962E-11));
#20001=CARTESIAN_POINT('Ctrl Pts',(7.27603165468577,-45.229519323734,-4.20081883448253));
#20002=CARTESIAN_POINT('Ctrl Pts',(4.85068776978043,-45.054519323734,-8.4016376689476));
#20003=CARTESIAN_POINT('Ctrl Pts',(-1.51301029103127E-11,-44.879519323734,
-8.40163766893887));
#20004=CARTESIAN_POINT('Ctrl Pts',(-4.85068776981069,-44.704519323734,-8.40163766893014));
#20005=CARTESIAN_POINT('Ctrl Pts',(-7.2760316547009,-44.529519323734,-4.20081883445633));
#20006=CARTESIAN_POINT('Ctrl Pts',(-9.70137553959111,-44.354519323734,1.74701439383464E-11));
#20007=CARTESIAN_POINT('Ctrl Pts',(-7.27603165468577,-44.179519323734,4.20081883448254));
#20008=CARTESIAN_POINT('Ctrl Pts',(-4.85068776978043,-44.004519323734,8.40163766894761));
#20009=CARTESIAN_POINT('Ctrl Pts',(1.51290740064448E-11,-43.829519323734,
8.40163766893887));
#20010=CARTESIAN_POINT('Ctrl Pts',(4.85068776981068,-43.654519323734,8.40163766893014));
#20011=CARTESIAN_POINT('Ctrl Pts',(7.2760316547009,-43.479519323734,4.20081883445634));
#20012=CARTESIAN_POINT('Ctrl Pts',(9.70137553959111,-43.304519323734,-1.74689558624962E-11));
#20013=CARTESIAN_POINT('Ctrl Pts',(7.27603165468577,-43.129519323734,-4.20081883448253));
#20014=CARTESIAN_POINT('Ctrl Pts',(4.85068776978043,-42.954519323734,-8.4016376689476));
#20015=CARTESIAN_POINT('Ctrl Pts',(-1.51301029103127E-11,-42.779519323734,
-8.40163766893887));
#20016=CARTESIAN_POINT('Ctrl Pts',(-4.85068776981069,-42.6045193237341,
-8.40163766893014));
#20017=CARTESIAN_POINT('Ctrl Pts',(-7.2760316547009,-42.429519323734,-4.20081883445633));
#20018=CARTESIAN_POINT('Ctrl Pts',(-9.70137553959111,-42.254519323734,1.74701439383464E-11));
#20019=CARTESIAN_POINT('Ctrl Pts',(-7.27603165468577,-42.079519323734,4.20081883448254));
#20020=CARTESIAN_POINT('Ctrl Pts',(-4.85068776978043,-41.904519323734,8.40163766894761));
#20021=CARTESIAN_POINT('Ctrl Pts',(1.51290740064448E-11,-41.729519323734,
8.40163766893887));
#20022=CARTESIAN_POINT('Ctrl Pts',(4.85068776981068,-41.554519323734,8.40163766893014));
#20023=CARTESIAN_POINT('Ctrl Pts',(7.2760316547009,-41.379519323734,4.20081883445634));
#20024=CARTESIAN_POINT('Ctrl Pts',(9.70137553959111,-41.2045193237341,-1.74689558624962E-11));
#20025=CARTESIAN_POINT('Ctrl Pts',(7.27603165468577,-41.029519323734,-4.20081883448253));
#20026=CARTESIAN_POINT('Ctrl Pts',(4.85068776978043,-40.854519323734,-8.4016376689476));
#20027=CARTESIAN_POINT('Ctrl Pts',(-1.51301029103127E-11,-40.679519323734,
-8.40163766893887));
#20028=CARTESIAN_POINT('Ctrl Pts',(-4.85068776981069,-40.504519323734,-8.40163766893014));
#20029=CARTESIAN_POINT('Ctrl Pts',(-7.2760316547009,-40.329519323734,-4.20081883445633));
#20030=CARTESIAN_POINT('Ctrl Pts',(-9.70137553959111,-40.154519323734,1.74701439383464E-11));
#20031=CARTESIAN_POINT('Ctrl Pts',(-7.27603165468577,-39.979519323734,4.20081883448254));
#20032=CARTESIAN_POINT('Ctrl Pts',(-4.85068776978043,-39.804519323734,8.40163766894761));
#20033=CARTESIAN_POINT('Ctrl Pts',(1.51290740064448E-11,-39.629519323734,
8.40163766893887));
#20034=CARTESIAN_POINT('Ctrl Pts',(4.85068776981068,-39.454519323734,8.40163766893014));
#20035=CARTESIAN_POINT('Ctrl Pts',(7.2760316547009,-39.279519323734,4.20081883445634));
#20036=CARTESIAN_POINT('Ctrl Pts',(9.70137553959111,-39.104519323734,-1.74689558624962E-11));
#20037=CARTESIAN_POINT('Ctrl Pts',(7.27603165468577,-38.929519323734,-4.20081883448253));
#20038=CARTESIAN_POINT('Ctrl Pts',(4.85068776978043,-38.7545193237341,-8.4016376689476));
#20039=CARTESIAN_POINT('Ctrl Pts',(-1.51301029103127E-11,-38.579519323734,
-8.40163766893887));
#20040=CARTESIAN_POINT('Ctrl Pts',(-4.85068776981069,-38.404519323734,-8.40163766893014));
#20041=CARTESIAN_POINT('Ctrl Pts',(-7.2760316547009,-38.2295193237341,-4.20081883445633));
#20042=CARTESIAN_POINT('Ctrl Pts',(-9.70137553959111,-38.054519323734,1.74701439383464E-11));
#20043=CARTESIAN_POINT('Ctrl Pts',(-7.27603165468577,-37.879519323734,4.20081883448254));
#20044=CARTESIAN_POINT('Ctrl Pts',(-4.85068776978043,-37.704519323734,8.40163766894761));
#20045=CARTESIAN_POINT('Ctrl Pts',(1.51290740064448E-11,-37.529519323734,
8.40163766893887));
#20046=CARTESIAN_POINT('Ctrl Pts',(4.85068776981068,-37.354519323734,8.40163766893014));
#20047=CARTESIAN_POINT('Ctrl Pts',(7.2760316547009,-37.179519323734,4.20081883445634));
#20048=CARTESIAN_POINT('Ctrl Pts',(9.70137553959111,-37.0045193237341,-1.74689558624962E-11));
#20049=CARTESIAN_POINT('Ctrl Pts',(7.27603165468577,-36.829519323734,-4.20081883448253));
#20050=CARTESIAN_POINT('Ctrl Pts',(4.85068776978043,-36.654519323734,-8.4016376689476));
#20051=CARTESIAN_POINT('Ctrl Pts',(-1.51301029103127E-11,-36.479519323734,
-8.40163766893887));
#20052=CARTESIAN_POINT('Ctrl Pts',(-4.85068776981069,-36.3045193237341,
-8.40163766893014));
#20053=CARTESIAN_POINT('Ctrl Pts',(-7.2760316547009,-36.129519323734,-4.20081883445633));
#20054=CARTESIAN_POINT('Ctrl Pts',(-9.70137553959111,-35.9545193237341,
1.74701439383464E-11));
#20055=CARTESIAN_POINT('Ctrl Pts',(-7.27603165468577,-35.779519323734,4.20081883448254));
#20056=CARTESIAN_POINT('Ctrl Pts',(-4.85068776978043,-35.604519323734,8.40163766894761));
#20057=CARTESIAN_POINT('Ctrl Pts',(1.51290740064448E-11,-35.429519323734,
8.40163766893887));
#20058=CARTESIAN_POINT('Ctrl Pts',(4.85068776981068,-35.2545193237341,8.40163766893014));
#20059=CARTESIAN_POINT('Ctrl Pts',(7.2760316547009,-35.079519323734,4.20081883445634));
#20060=CARTESIAN_POINT('Ctrl Pts',(9.70137553959111,-34.9045193237341,-1.74689558624962E-11));
#20061=CARTESIAN_POINT('Ctrl Pts',(7.27603165468577,-34.729519323734,-4.20081883448253));
#20062=CARTESIAN_POINT('Ctrl Pts',(4.85068776978043,-34.5545193237341,-8.4016376689476));
#20063=CARTESIAN_POINT('Ctrl Pts',(-1.51301029103127E-11,-34.3795193237341,
-8.40163766893887));
#20064=CARTESIAN_POINT('Ctrl Pts',(-4.85068776981069,-34.204519323734,-8.40163766893014));
#20065=CARTESIAN_POINT('Ctrl Pts',(-7.2760316547009,-34.029519323734,-4.20081883445633));
#20066=CARTESIAN_POINT('Ctrl Pts',(-9.70137553959111,-33.8545193237341,
1.74701439383464E-11));
#20067=CARTESIAN_POINT('Ctrl Pts',(-7.27603165468577,-33.679519323734,4.20081883448254));
#20068=CARTESIAN_POINT('Ctrl Pts',(-4.85068776978043,-33.504519323734,8.40163766894761));
#20069=CARTESIAN_POINT('Ctrl Pts',(1.51290740064448E-11,-33.3295193237341,
8.40163766893887));
#20070=CARTESIAN_POINT('Ctrl Pts',(4.85068776981068,-33.154519323734,8.40163766893014));
#20071=CARTESIAN_POINT('Ctrl Pts',(7.2760316547009,-32.9795193237341,4.20081883445634));
#20072=CARTESIAN_POINT('Ctrl Pts',(9.70137553959111,-32.8045193237341,-1.74689558624962E-11));
#20073=CARTESIAN_POINT('Ctrl Pts',(7.27603165468577,-32.6295193237341,-4.20081883448253));
#20074=CARTESIAN_POINT('Ctrl Pts',(4.85068776978043,-32.4545193237341,-8.4016376689476));
#20075=CARTESIAN_POINT('Ctrl Pts',(-1.51301029103127E-11,-32.279519323734,
-8.40163766893887));
#20076=CARTESIAN_POINT('Ctrl Pts',(-4.85068776981069,-32.1045193237341,
-8.40163766893014));
#20077=CARTESIAN_POINT('Ctrl Pts',(-7.2760316547009,-31.9295193237341,-4.20081883445633));
#20078=CARTESIAN_POINT('Ctrl Pts',(-9.70137553959111,-31.7545193237341,
1.74701439383464E-11));
#20079=CARTESIAN_POINT('Ctrl Pts',(-7.27603165468577,-31.5795193237341,
4.20081883448254));
#20080=CARTESIAN_POINT('Ctrl Pts',(-4.85068776978043,-31.4045193237341,
8.40163766894761));
#20081=CARTESIAN_POINT('Ctrl Pts',(1.51290740064448E-11,-31.2295193237341,
8.40163766893887));
#20082=CARTESIAN_POINT('Ctrl Pts',(4.85068776981068,-31.0545193237341,8.40163766893014));
#20083=CARTESIAN_POINT('Ctrl Pts',(7.2760316547009,-30.8795193237341,4.20081883445634));
#20084=CARTESIAN_POINT('Ctrl Pts',(9.70137553959111,-30.7045193237341,-1.74689558624962E-11));
#20085=CARTESIAN_POINT('Ctrl Pts',(7.27603165468577,-30.5295193237341,-4.20081883448253));
#20086=CARTESIAN_POINT('Ctrl Pts',(4.85068776978043,-30.3545193237341,-8.4016376689476));
#20087=CARTESIAN_POINT('Ctrl Pts',(-1.51301029103127E-11,-30.1795193237341,
-8.40163766893887));
#20088=CARTESIAN_POINT('Ctrl Pts',(-4.85068776981069,-30.0045193237341,
-8.40163766893014));
#20089=CARTESIAN_POINT('Ctrl Pts',(-7.2760316547009,-29.8295193237341,-4.20081883445633));
#20090=CARTESIAN_POINT('Ctrl Pts',(-9.70137553959111,-29.6545193237341,
1.74701439383464E-11));
#20091=CARTESIAN_POINT('Ctrl Pts',(-7.27603165468577,-29.4795193237341,
4.20081883448254));
#20092=CARTESIAN_POINT('Ctrl Pts',(-4.85068776978043,-29.3045193237341,
8.40163766894761));
#20093=CARTESIAN_POINT('Ctrl Pts',(1.51290740064448E-11,-29.1295193237341,
8.40163766893887));
#20094=CARTESIAN_POINT('Ctrl Pts',(4.85068776981068,-28.9545193237341,8.40163766893014));
#20095=CARTESIAN_POINT('Ctrl Pts',(7.2760316547009,-28.7795193237341,4.20081883445634));
#20096=CARTESIAN_POINT('Ctrl Pts',(9.70137553959111,-28.6045193237341,-1.74689558624962E-11));
#20097=CARTESIAN_POINT('Ctrl Pts',(7.27603165468577,-28.4295193237341,-4.20081883448253));
#20098=CARTESIAN_POINT('Ctrl Pts',(4.85068776978043,-28.2545193237341,-8.4016376689476));
#20099=CARTESIAN_POINT('Ctrl Pts',(-1.51301029103127E-11,-28.0795193237341,
-8.40163766893887));
#20100=CARTESIAN_POINT('Ctrl Pts',(-4.85068776981069,-27.9045193237341,
-8.40163766893014));
#20101=CARTESIAN_POINT('Ctrl Pts',(-7.2760316547009,-27.7295193237341,-4.20081883445633));
#20102=CARTESIAN_POINT('Ctrl Pts',(-9.70137553959111,-27.5545193237341,
1.74701439383464E-11));
#20103=CARTESIAN_POINT('Ctrl Pts',(-7.27603165468577,-27.3795193237341,
4.20081883448254));
#20104=CARTESIAN_POINT('Ctrl Pts',(-4.85068776978043,-27.2045193237341,
8.40163766894761));
#20105=CARTESIAN_POINT('Ctrl Pts',(1.51290740064448E-11,-27.0295193237341,
8.40163766893887));
#20106=CARTESIAN_POINT('Ctrl Pts',(4.85068776981068,-26.8545193237341,8.40163766893014));
#20107=CARTESIAN_POINT('Ctrl Pts',(7.2760316547009,-26.6795193237341,4.20081883445634));
#20108=CARTESIAN_POINT('Ctrl Pts',(9.70137553959111,-26.5045193237341,-1.74689558624962E-11));
#20109=CARTESIAN_POINT('Ctrl Pts',(7.27603165468577,-26.3295193237341,-4.20081883448253));
#20110=CARTESIAN_POINT('Ctrl Pts',(4.85068776978043,-26.1545193237341,-8.4016376689476));
#20111=CARTESIAN_POINT('Ctrl Pts',(-1.51301029103127E-11,-25.9795193237341,
-8.40163766893887));
#20112=CARTESIAN_POINT('Ctrl Pts',(-4.85068776981069,-25.8045193237341,
-8.40163766893014));
#20113=CARTESIAN_POINT('Ctrl Pts',(-7.2760316547009,-25.6295193237341,-4.20081883445633));
#20114=CARTESIAN_POINT('Ctrl Pts',(-9.70137553959111,-25.4545193237341,
1.74701439383464E-11));
#20115=CARTESIAN_POINT('Ctrl Pts',(-7.27603165468577,-25.2795193237341,
4.20081883448254));
#20116=CARTESIAN_POINT('Ctrl Pts',(-4.85068776978043,-25.1045193237341,
8.40163766894761));
#20117=CARTESIAN_POINT('Ctrl Pts',(1.51290740064448E-11,-24.9295193237341,
8.40163766893887));
#20118=CARTESIAN_POINT('Ctrl Pts',(4.85068776981068,-24.7545193237341,8.40163766893014));
#20119=CARTESIAN_POINT('Ctrl Pts',(7.2760316547009,-24.5795193237341,4.20081883445634));
#20120=CARTESIAN_POINT('Ctrl Pts',(9.70137553959111,-24.4045193237341,-1.74689558624962E-11));
#20121=CARTESIAN_POINT('Ctrl Pts',(7.27603165468577,-24.2295193237341,-4.20081883448253));
#20122=CARTESIAN_POINT('Ctrl Pts',(4.85068776978043,-24.0545193237341,-8.4016376689476));
#20123=CARTESIAN_POINT('Ctrl Pts',(-1.51301029103127E-11,-23.8795193237341,
-8.40163766893887));
#20124=CARTESIAN_POINT('Ctrl Pts',(-4.85068776981069,-23.7045193237341,
-8.40163766893014));
#20125=CARTESIAN_POINT('Ctrl Pts',(-7.2760316547009,-23.5295193237341,-4.20081883445633));
#20126=CARTESIAN_POINT('Ctrl Pts',(-9.70137553959111,-23.3545193237341,
1.74701439383464E-11));
#20127=CARTESIAN_POINT('Ctrl Pts',(-7.27603165468577,-23.1795193237341,
4.20081883448254));
#20128=CARTESIAN_POINT('Ctrl Pts',(-4.85068776978043,-23.0045193237341,
8.40163766894761));
#20129=CARTESIAN_POINT('Ctrl Pts',(1.51290740064448E-11,-22.8295193237341,
8.40163766893887));
#20130=CARTESIAN_POINT('Ctrl Pts',(4.85068776981068,-22.6545193237341,8.40163766893014));
#20131=CARTESIAN_POINT('Ctrl Pts',(7.2760316547009,-22.4795193237341,4.20081883445634));
#20132=CARTESIAN_POINT('Ctrl Pts',(9.70137553959111,-22.3045193237341,-1.74689558624962E-11));
#20133=CARTESIAN_POINT('Ctrl Pts',(7.27603165468577,-22.1295193237341,-4.20081883448253));
#20134=CARTESIAN_POINT('Ctrl Pts',(4.85068776978043,-21.9545193237341,-8.4016376689476));
#20135=CARTESIAN_POINT('Ctrl Pts',(-1.51301029103127E-11,-21.7795193237341,
-8.40163766893887));
#20136=CARTESIAN_POINT('Ctrl Pts',(-4.85068776981069,-21.6045193237341,
-8.40163766893014));
#20137=CARTESIAN_POINT('Ctrl Pts',(-7.2760316547009,-21.4295193237341,-4.20081883445633));
#20138=CARTESIAN_POINT('Ctrl Pts',(-9.70137553959111,-21.2545193237341,
1.74701439383464E-11));
#20139=CARTESIAN_POINT('Ctrl Pts',(-7.27603165468577,-21.0795193237341,
4.20081883448254));
#20140=CARTESIAN_POINT('Ctrl Pts',(-4.85068776978043,-20.9045193237341,
8.40163766894761));
#20141=CARTESIAN_POINT('Ctrl Pts',(1.51290740064448E-11,-20.7295193237341,
8.40163766893887));
#20142=CARTESIAN_POINT('Ctrl Pts',(4.85068776981068,-20.5545193237341,8.40163766893014));
#20143=CARTESIAN_POINT('Ctrl Pts',(7.2760316547009,-20.3795193237341,4.20081883445634));
#20144=CARTESIAN_POINT('Ctrl Pts',(9.70137553959111,-20.2045193237341,-1.74689558624962E-11));
#20145=CARTESIAN_POINT('Ctrl Pts',(7.27603165468577,-20.0295193237341,-4.20081883448253));
#20146=CARTESIAN_POINT('Ctrl Pts',(4.85068776978043,-19.8545193237341,-8.4016376689476));
#20147=CARTESIAN_POINT('Ctrl Pts',(-1.51301029103127E-11,-19.6795193237341,
-8.40163766893887));
#20148=CARTESIAN_POINT('Ctrl Pts',(-4.85068776981069,-19.5045193237341,
-8.40163766893014));
#20149=CARTESIAN_POINT('Ctrl Pts',(-7.2760316547009,-19.3295193237341,-4.20081883445633));
#20150=CARTESIAN_POINT('Ctrl Pts',(-9.70137553959111,-19.1545193237341,
1.74701439383464E-11));
#20151=CARTESIAN_POINT('Ctrl Pts',(-7.27603165468577,-18.9795193237341,
4.20081883448254));
#20152=CARTESIAN_POINT('Ctrl Pts',(-4.85068776978043,-18.8045193237341,
8.40163766894761));
#20153=CARTESIAN_POINT('Ctrl Pts',(1.51290740064448E-11,-18.6295193237341,
8.40163766893887));
#20154=CARTESIAN_POINT('Ctrl Pts',(4.85068776981068,-18.4545193237341,8.40163766893014));
#20155=CARTESIAN_POINT('Ctrl Pts',(7.2760316547009,-18.2795193237341,4.20081883445634));
#20156=CARTESIAN_POINT('Ctrl Pts',(9.70137553959111,-18.1045193237341,-1.74689558624962E-11));
#20157=CARTESIAN_POINT('Ctrl Pts',(7.27603165468577,-17.9295193237341,-4.20081883448253));
#20158=CARTESIAN_POINT('Ctrl Pts',(4.85068776978043,-17.7545193237341,-8.4016376689476));
#20159=CARTESIAN_POINT('Ctrl Pts',(-1.51301029103127E-11,-17.5795193237341,
-8.40163766893887));
#20160=CARTESIAN_POINT('Ctrl Pts',(-4.85068776981069,-17.4045193237341,
-8.40163766893014));
#20161=CARTESIAN_POINT('Ctrl Pts',(-7.2760316547009,-17.2295193237341,-4.20081883445633));
#20162=CARTESIAN_POINT('Ctrl Pts',(-9.70137553959111,-17.0545193237341,
1.74701439383464E-11));
#20163=CARTESIAN_POINT('Ctrl Pts',(-7.27603165468577,-16.8795193237341,
4.20081883448254));
#20164=CARTESIAN_POINT('Ctrl Pts',(-4.85068776978043,-16.7045193237341,
8.40163766894761));
#20165=CARTESIAN_POINT('Ctrl Pts',(1.51290740064448E-11,-16.5295193237341,
8.40163766893887));
#20166=CARTESIAN_POINT('Ctrl Pts',(4.85068776981068,-16.3545193237341,8.40163766893014));
#20167=CARTESIAN_POINT('Ctrl Pts',(7.2760316547009,-16.1795193237341,4.20081883445634));
#20168=CARTESIAN_POINT('Ctrl Pts',(9.70137553959111,-16.0045193237341,-1.74689558624962E-11));
#20169=CARTESIAN_POINT('Ctrl Pts',(7.27603165468577,-15.8295193237341,-4.20081883448253));
#20170=CARTESIAN_POINT('Ctrl Pts',(4.85068776978043,-15.6545193237341,-8.4016376689476));
#20171=CARTESIAN_POINT('Ctrl Pts',(-1.51301029103127E-11,-15.4795193237341,
-8.40163766893887));
#20172=CARTESIAN_POINT('Ctrl Pts',(-4.85068776981069,-15.3045193237341,
-8.40163766893014));
#20173=CARTESIAN_POINT('Ctrl Pts',(-7.2760316547009,-15.1295193237341,-4.20081883445633));
#20174=CARTESIAN_POINT('Ctrl Pts',(-9.70137553959111,-14.9545193237341,
1.74701439383464E-11));
#20175=CARTESIAN_POINT('Ctrl Pts',(-7.27603165468577,-14.7795193237341,
4.20081883448254));
#20176=CARTESIAN_POINT('Ctrl Pts',(-4.85068776978043,-14.6045193237341,
8.40163766894761));
#20177=CARTESIAN_POINT('Ctrl Pts',(1.51290740064448E-11,-14.4295193237341,
8.40163766893887));
#20178=CARTESIAN_POINT('Ctrl Pts',(4.85068776981068,-14.2545193237341,8.40163766893014));
#20179=CARTESIAN_POINT('Ctrl Pts',(7.2760316547009,-14.0795193237341,4.20081883445634));
#20180=CARTESIAN_POINT('Ctrl Pts',(9.70137553959111,-13.9045193237341,-1.74689558624962E-11));
#20181=CARTESIAN_POINT('Ctrl Pts',(7.27603165468577,-13.7295193237341,-4.20081883448253));
#20182=CARTESIAN_POINT('Ctrl Pts',(4.85068776978043,-13.5545193237341,-8.4016376689476));
#20183=CARTESIAN_POINT('Ctrl Pts',(-1.51301029103127E-11,-13.3795193237341,
-8.40163766893887));
#20184=CARTESIAN_POINT('Ctrl Pts',(-4.85068776981069,-13.2045193237341,
-8.40163766893014));
#20185=CARTESIAN_POINT('Ctrl Pts',(-7.2760316547009,-13.0295193237341,-4.20081883445633));
#20186=CARTESIAN_POINT('Ctrl Pts',(-9.70137553959111,-12.8545193237341,
1.74701439383464E-11));
#20187=CARTESIAN_POINT('Ctrl Pts',(-7.27603165468577,-12.6795193237341,
4.20081883448254));
#20188=CARTESIAN_POINT('Ctrl Pts',(-4.85068776978043,-12.5045193237341,
8.40163766894761));
#20189=CARTESIAN_POINT('Ctrl Pts',(1.51290740064448E-11,-12.3295193237341,
8.40163766893887));
#20190=CARTESIAN_POINT('Ctrl Pts',(4.85068776981068,-12.1545193237341,8.40163766893014));
#20191=CARTESIAN_POINT('Ctrl Pts',(7.2760316547009,-11.9795193237341,4.20081883445634));
#20192=CARTESIAN_POINT('Ctrl Pts',(9.70137553959111,-11.8045193237341,-1.74689558624962E-11));
#20193=CARTESIAN_POINT('Ctrl Pts',(7.27603165468577,-11.6295193237341,-4.20081883448253));
#20194=CARTESIAN_POINT('Ctrl Pts',(4.85068776978043,-11.4545193237341,-8.4016376689476));
#20195=CARTESIAN_POINT('Ctrl Pts',(-1.51301029103127E-11,-11.2795193237341,
-8.40163766893887));
#20196=CARTESIAN_POINT('Ctrl Pts',(-4.85068776981069,-11.1045193237341,
-8.40163766893014));
#20197=CARTESIAN_POINT('Ctrl Pts',(-7.2760316547009,-10.9295193237341,-4.20081883445633));
#20198=CARTESIAN_POINT('Ctrl Pts',(-9.70137553959111,-10.7545193237341,
1.74701439383464E-11));
#20199=CARTESIAN_POINT('Ctrl Pts',(-7.27603165468577,-10.5795193237341,
4.20081883448254));
#20200=CARTESIAN_POINT('Ctrl Pts',(-4.85068776978043,-10.4045193237341,
8.40163766894761));
#20201=CARTESIAN_POINT('Ctrl Pts',(1.51290740064448E-11,-10.2295193237341,
8.40163766893887));
#20202=CARTESIAN_POINT('Ctrl Pts',(4.85068776981068,-10.0545193237341,8.40163766893014));
#20203=CARTESIAN_POINT('Ctrl Pts',(7.2760316547009,-9.87951932373411,4.20081883445634));
#20204=CARTESIAN_POINT('Ctrl Pts',(9.70137553959111,-9.70451932373411,-1.74689558624962E-11));
#20205=CARTESIAN_POINT('Ctrl Pts',(7.27603165468577,-9.5295193237341,-4.20081883448253));
#20206=CARTESIAN_POINT('Ctrl Pts',(4.85068776978043,-9.35451932373412,-8.4016376689476));
#20207=CARTESIAN_POINT('Ctrl Pts',(-1.51301029103127E-11,-9.17951932373411,
-8.40163766893887));
#20208=CARTESIAN_POINT('Ctrl Pts',(-4.85068776981069,-9.00451932373411,
-8.40163766893014));
#20209=CARTESIAN_POINT('Ctrl Pts',(-7.2760316547009,-8.82951932373412,-4.20081883445633));
#20210=CARTESIAN_POINT('Ctrl Pts',(-9.70137553959111,-8.65451932373411,
1.74701439383464E-11));
#20211=CARTESIAN_POINT('Ctrl Pts',(-7.27603165468577,-8.4795193237341,4.20081883448254));
#20212=CARTESIAN_POINT('Ctrl Pts',(-4.85068776978043,-8.30451932373413,
8.40163766894761));
#20213=CARTESIAN_POINT('Ctrl Pts',(1.51290740064448E-11,-8.12951932373411,
8.40163766893887));
#20214=CARTESIAN_POINT('Ctrl Pts',(4.85068776981068,-7.95451932373411,8.40163766893014));
#20215=CARTESIAN_POINT('Ctrl Pts',(7.2760316547009,-7.77951932373412,4.20081883445634));
#20216=CARTESIAN_POINT('Ctrl Pts',(9.70137553959111,-7.60451932373411,-1.74689558624962E-11));
#20217=CARTESIAN_POINT('Ctrl Pts',(7.27603165468577,-7.42951932373411,-4.20081883448253));
#20218=CARTESIAN_POINT('Ctrl Pts',(4.85068776978043,-7.25451932373413,-8.4016376689476));
#20219=CARTESIAN_POINT('Ctrl Pts',(-1.51301029103127E-11,-7.07951932373412,
-8.40163766893887));
#20220=CARTESIAN_POINT('Ctrl Pts',(-4.85068776981069,-6.90451932373412,
-8.40163766893014));
#20221=CARTESIAN_POINT('Ctrl Pts',(-7.2760316547009,-6.7295193237341,-4.20081883445633));
#20222=CARTESIAN_POINT('Ctrl Pts',(-9.70137553959111,-6.55451932373412,
1.74701439383464E-11));
#20223=CARTESIAN_POINT('Ctrl Pts',(-7.27603165468577,-6.37951932373411,
4.20081883448254));
#20224=CARTESIAN_POINT('Ctrl Pts',(-4.85068776978043,-6.2045193237341,8.40163766894761));
#20225=CARTESIAN_POINT('Ctrl Pts',(1.51290740064448E-11,-6.02951932373412,
8.40163766893887));
#20226=CARTESIAN_POINT('Ctrl Pts',(4.85068776981068,-5.85451932373412,8.40163766893014));
#20227=CARTESIAN_POINT('Ctrl Pts',(7.2760316547009,-5.6795193237341,4.20081883445634));
#20228=CARTESIAN_POINT('Ctrl Pts',(9.70137553959111,-5.50451932373412,-1.74689558624962E-11));
#20229=CARTESIAN_POINT('Ctrl Pts',(7.27603165468577,-5.32951932373411,-4.20081883448253));
#20230=CARTESIAN_POINT('Ctrl Pts',(4.85068776978043,-5.15451932373411,-8.4016376689476));
#20231=CARTESIAN_POINT('Ctrl Pts',(-1.51301029103127E-11,-4.97951932373413,
-8.40163766893887));
#20232=CARTESIAN_POINT('Ctrl Pts',(-4.85068776981069,-4.80451932373413,
-8.40163766893014));
#20233=CARTESIAN_POINT('Ctrl Pts',(-7.2760316547009,-4.62951932373411,-4.20081883445633));
#20234=CARTESIAN_POINT('Ctrl Pts',(-9.70137553959111,-4.45451932373413,
1.74701439383464E-11));
#20235=CARTESIAN_POINT('Ctrl Pts',(-7.27603165468577,-4.27951932373412,
4.20081883448254));
#20236=CARTESIAN_POINT('Ctrl Pts',(-4.85068776978043,-4.10451932373411,
8.40163766894761));
#20237=CARTESIAN_POINT('Ctrl Pts',(1.51290740064448E-11,-3.92951932373413,
8.40163766893887));
#20238=CARTESIAN_POINT('Ctrl Pts',(4.85068776981068,-3.75451932373413,8.40163766893014));
#20239=CARTESIAN_POINT('Ctrl Pts',(7.2760316547009,-3.57951932373411,4.20081883445634));
#20240=CARTESIAN_POINT('Ctrl Pts',(9.70137553959111,-3.40451932373413,-1.74689558624962E-11));
#20241=CARTESIAN_POINT('Ctrl Pts',(7.27603165468577,-3.22951932373412,-4.20081883448253));
#20242=CARTESIAN_POINT('Ctrl Pts',(4.85068776978043,-3.05451932373412,-8.4016376689476));
#20243=CARTESIAN_POINT('Ctrl Pts',(-1.51301029103127E-11,-2.87951932373413,
-8.40163766893887));
#20244=CARTESIAN_POINT('Ctrl Pts',(-4.85068776981069,-2.70451932373414,
-8.40163766893014));
#20245=CARTESIAN_POINT('Ctrl Pts',(-7.2760316547009,-2.52951932373412,-4.20081883445633));
#20246=CARTESIAN_POINT('Ctrl Pts',(-9.70137553959111,-2.35451932373412,
1.74701439383464E-11));
#20247=CARTESIAN_POINT('Ctrl Pts',(-7.27603165468577,-2.17951932373413,
4.20081883448254));
#20248=CARTESIAN_POINT('Ctrl Pts',(-4.85068776978043,-2.00451932373412,
8.40163766894761));
#20249=CARTESIAN_POINT('Ctrl Pts',(1.51290740064448E-11,-1.82951932373411,
8.40163766893887));
#20250=CARTESIAN_POINT('Ctrl Pts',(4.85068776981068,-1.65451932373413,8.40163766893014));
#20251=CARTESIAN_POINT('Ctrl Pts',(7.2760316547009,-1.47951932373412,4.20081883445634));
#20252=CARTESIAN_POINT('Ctrl Pts',(9.70137553959111,-1.30451932373412,-1.74689558624962E-11));
#20253=CARTESIAN_POINT('Ctrl Pts',(7.27603165468577,-1.12951932373413,-4.20081883448253));
#20254=CARTESIAN_POINT('Ctrl Pts',(4.85068776978043,-0.954519323734127,
-8.4016376689476));
#20255=CARTESIAN_POINT('Ctrl Pts',(-1.51301029103127E-11,-0.779519323734116,
-8.40163766893887));
#20256=CARTESIAN_POINT('Ctrl Pts',(-4.85068776981069,-0.604519323734136,
-8.40163766893014));
#20257=CARTESIAN_POINT('Ctrl Pts',(-7.2760316547009,-0.429519323734127,
-4.20081883445633));
#20258=CARTESIAN_POINT('Ctrl Pts',(-9.70137553959111,-0.254519323734122,
1.74701439383464E-11));
#20259=CARTESIAN_POINT('Ctrl Pts',(-7.27603165468577,-0.0795193237341377,
4.20081883448254));
#20260=CARTESIAN_POINT('Ctrl Pts',(-4.85068776978043,0.0954806762658689,
8.40163766894761));
#20261=CARTESIAN_POINT('Ctrl Pts',(1.51290740064448E-11,0.270480676265879,
8.40163766893887));
#20262=CARTESIAN_POINT('Ctrl Pts',(4.85068776981068,0.445480676265859,8.40163766893014));
#20263=CARTESIAN_POINT('Ctrl Pts',(7.2760316547009,0.620480676265869,4.20081883445634));
#20264=CARTESIAN_POINT('Ctrl Pts',(9.70137553959111,0.795480676265874,-1.74689558624962E-11));
#20265=CARTESIAN_POINT('Ctrl Pts',(7.27603165468577,0.970480676265858,-4.20081883448253));
#20266=CARTESIAN_POINT('Ctrl Pts',(4.85068776978043,1.14548067626586,-8.4016376689476));
#20267=CARTESIAN_POINT('Ctrl Pts',(-1.51301029103127E-11,1.32048067626587,
-8.40163766893887));
#20268=CARTESIAN_POINT('Ctrl Pts',(-4.85068776981069,1.49548067626586,-8.40163766893014));
#20269=CARTESIAN_POINT('Ctrl Pts',(-7.2760316547009,1.67048067626586,-4.20081883445633));
#20270=CARTESIAN_POINT('Ctrl Pts',(-9.70137553959111,1.84548067626587,1.74701439383464E-11));
#20271=CARTESIAN_POINT('Ctrl Pts',(-7.27603165468577,2.02048067626588,4.20081883448254));
#20272=CARTESIAN_POINT('Ctrl Pts',(-4.85068776978043,2.19548067626586,8.40163766894761));
#20273=CARTESIAN_POINT('Ctrl Pts',(1.51290740064448E-11,2.37048067626587,
8.40163766893887));
#20274=CARTESIAN_POINT('Ctrl Pts',(4.85068776981068,2.54548067626587,8.40163766893014));
#20275=CARTESIAN_POINT('Ctrl Pts',(7.2760316547009,2.72048067626586,4.20081883445634));
#20276=CARTESIAN_POINT('Ctrl Pts',(9.70137553959111,2.89548067626586,-1.74689558624962E-11));
#20277=CARTESIAN_POINT('Ctrl Pts',(7.27603165468577,3.07048067626588,-4.20081883448253));
#20278=CARTESIAN_POINT('Ctrl Pts',(4.85068776978043,3.24548067626586,-8.4016376689476));
#20279=CARTESIAN_POINT('Ctrl Pts',(-1.51301029103127E-11,3.42048067626587,
-8.40163766893887));
#20280=CARTESIAN_POINT('Ctrl Pts',(-4.85068776981069,3.59548067626587,-8.40163766893014));
#20281=CARTESIAN_POINT('Ctrl Pts',(-7.2760316547009,3.77048067626585,-4.20081883445633));
#20282=CARTESIAN_POINT('Ctrl Pts',(-9.70137553959111,3.94548067626586,1.74701439383464E-11));
#20283=CARTESIAN_POINT('Ctrl Pts',(-7.27603165468577,4.12048067626587,4.20081883448254));
#20284=CARTESIAN_POINT('Ctrl Pts',(-4.85068776978043,4.29548067626585,8.40163766894761));
#20285=CARTESIAN_POINT('Ctrl Pts',(1.51290740064448E-11,4.47048067626586,
8.40163766893887));
#20286=CARTESIAN_POINT('Ctrl Pts',(4.85068776981068,4.64548067626587,8.40163766893014));
#20287=CARTESIAN_POINT('Ctrl Pts',(7.2760316547009,4.82048067626585,4.20081883445634));
#20288=CARTESIAN_POINT('Ctrl Pts',(9.70137553959111,4.99548067626586,-1.74689558624962E-11));
#20289=CARTESIAN_POINT('Ctrl Pts',(7.27603165468577,5.17048067626587,-4.20081883448253));
#20290=CARTESIAN_POINT('Ctrl Pts',(4.85068776978043,5.34548067626585,-8.4016376689476));
#20291=CARTESIAN_POINT('Ctrl Pts',(-1.51301029103127E-11,5.52048067626585,
-8.40163766893887));
#20292=CARTESIAN_POINT('Ctrl Pts',(-4.85068776981069,5.69548067626586,-8.40163766893014));
#20293=CARTESIAN_POINT('Ctrl Pts',(-7.2760316547009,5.87048067626585,-4.20081883445633));
#20294=CARTESIAN_POINT('Ctrl Pts',(-9.70137553959111,6.04548067626585,1.74701439383464E-11));
#20295=CARTESIAN_POINT('Ctrl Pts',(-7.27603165468577,6.22048067626586,4.20081883448254));
#20296=CARTESIAN_POINT('Ctrl Pts',(-4.85068776978043,6.39548067626584,8.40163766894761));
#20297=CARTESIAN_POINT('Ctrl Pts',(1.51290740064448E-11,6.57048067626585,
8.40163766893887));
#20298=CARTESIAN_POINT('Ctrl Pts',(4.85068776981068,6.74548067626586,8.40163766893014));
#20299=CARTESIAN_POINT('Ctrl Pts',(7.2760316547009,6.92048067626587,4.20081883445634));
#20300=CARTESIAN_POINT('Ctrl Pts',(9.70137553959111,7.09548067626585,-1.74689558624962E-11));
#20301=CARTESIAN_POINT('Ctrl Pts',(7.27603165468577,7.27048067626586,-4.20081883448253));
#20302=CARTESIAN_POINT('Ctrl Pts',(4.85068776978043,7.44548067626586,-8.4016376689476));
#20303=CARTESIAN_POINT('Ctrl Pts',(-1.51301029103127E-11,7.62048067626585,
-8.40163766893887));
#20304=CARTESIAN_POINT('Ctrl Pts',(-4.85068776981069,7.79548067626585,-8.40163766893014));
#20305=CARTESIAN_POINT('Ctrl Pts',(-7.2760316547009,7.97048067626586,-4.20081883445633));
#20306=CARTESIAN_POINT('Ctrl Pts',(-9.70137553959111,8.14548067626584,1.74701439383464E-11));
#20307=CARTESIAN_POINT('Ctrl Pts',(-7.27603165468577,8.32048067626585,4.20081883448254));
#20308=CARTESIAN_POINT('Ctrl Pts',(-4.85068776978043,8.49548067626586,8.40163766894761));
#20309=CARTESIAN_POINT('Ctrl Pts',(1.51290740064448E-11,8.67048067626584,
8.40163766893887));
#20310=CARTESIAN_POINT('Ctrl Pts',(4.85068776981068,8.84548067626585,8.40163766893014));
#20311=CARTESIAN_POINT('Ctrl Pts',(7.2760316547009,9.02048067626586,4.20081883445634));
#20312=CARTESIAN_POINT('Ctrl Pts',(9.70137553959111,9.19548067626584,-1.74689558624962E-11));
#20313=CARTESIAN_POINT('Ctrl Pts',(7.27603165468577,9.37048067626585,-4.20081883448253));
#20314=CARTESIAN_POINT('Ctrl Pts',(4.85068776978043,9.54548067626585,-8.4016376689476));
#20315=CARTESIAN_POINT('Ctrl Pts',(-1.51301029103127E-11,9.72048067626584,
-8.40163766893887));
#20316=CARTESIAN_POINT('Ctrl Pts',(-4.85068776981069,9.89548067626584,-8.40163766893014));
#20317=CARTESIAN_POINT('Ctrl Pts',(-7.2760316547009,10.0704806762659,-4.20081883445633));
#20318=CARTESIAN_POINT('Ctrl Pts',(-9.70137553959111,10.2454806762658,1.74701439383464E-11));
#20319=CARTESIAN_POINT('Ctrl Pts',(-7.27603165468577,10.4204806762658,4.20081883448254));
#20320=CARTESIAN_POINT('Ctrl Pts',(-4.85068776978043,10.5954806762658,8.40163766894761));
#20321=CARTESIAN_POINT('Ctrl Pts',(1.51290740064448E-11,10.7704806762658,
8.40163766893887));
#20322=CARTESIAN_POINT('Ctrl Pts',(4.85068776981068,10.9454806762658,8.40163766893014));
#20323=CARTESIAN_POINT('Ctrl Pts',(7.2760316547009,11.1204806762658,4.20081883445634));
#20324=CARTESIAN_POINT('Ctrl Pts',(9.70137553959111,11.2954806762659,-1.74689558624962E-11));
#20325=CARTESIAN_POINT('Ctrl Pts',(7.27603165468577,11.4704806762658,-4.20081883448253));
#20326=CARTESIAN_POINT('Ctrl Pts',(4.85068776978043,11.6454806762658,-8.4016376689476));
#20327=CARTESIAN_POINT('Ctrl Pts',(-1.51301029103127E-11,11.8204806762659,
-8.40163766893887));
#20328=CARTESIAN_POINT('Ctrl Pts',(-4.85068776981069,11.9954806762658,-8.40163766893014));
#20329=CARTESIAN_POINT('Ctrl Pts',(-7.2760316547009,12.1704806762658,-4.20081883445633));
#20330=CARTESIAN_POINT('Ctrl Pts',(-9.70137553959111,12.3454806762658,1.74701439383464E-11));
#20331=CARTESIAN_POINT('Ctrl Pts',(-7.27603165468577,12.5204806762658,4.20081883448254));
#20332=CARTESIAN_POINT('Ctrl Pts',(-4.85068776978043,12.6954806762658,8.40163766894761));
#20333=CARTESIAN_POINT('Ctrl Pts',(1.51290740064448E-11,12.8704806762659,
8.40163766893887));
#20334=CARTESIAN_POINT('Ctrl Pts',(4.85068776981068,13.0454806762658,8.40163766893014));
#20335=CARTESIAN_POINT('Ctrl Pts',(7.2760316547009,13.2204806762658,4.20081883445634));
#20336=CARTESIAN_POINT('Ctrl Pts',(9.70137553959111,13.3954806762658,-1.74689558624962E-11));
#20337=CARTESIAN_POINT('Ctrl Pts',(7.27603165468577,13.5704806762658,-4.20081883448253));
#20338=CARTESIAN_POINT('Ctrl Pts',(4.85068776978043,13.7454806762658,-8.4016376689476));
#20339=CARTESIAN_POINT('Ctrl Pts',(-1.51301029103127E-11,13.9204806762658,
-8.40163766893887));
#20340=CARTESIAN_POINT('Ctrl Pts',(-4.85068776981069,14.0954806762658,-8.40163766893014));
#20341=CARTESIAN_POINT('Ctrl Pts',(-7.2760316547009,14.2704806762658,-4.20081883445633));
#20342=CARTESIAN_POINT('Ctrl Pts',(-9.70137553959111,14.4454806762658,1.74701439383464E-11));
#20343=CARTESIAN_POINT('Ctrl Pts',(-7.27603165468577,14.6204806762658,4.20081883448254));
#20344=CARTESIAN_POINT('Ctrl Pts',(-4.85068776978043,14.7954806762658,8.40163766894761));
#20345=CARTESIAN_POINT('Ctrl Pts',(1.51290740064448E-11,14.9704806762658,
8.40163766893887));
#20346=CARTESIAN_POINT('Ctrl Pts',(4.85068776981068,15.1454806762658,8.40163766893014));
#20347=CARTESIAN_POINT('Ctrl Pts',(7.2760316547009,15.3204806762658,4.20081883445634));
#20348=CARTESIAN_POINT('Ctrl Pts',(9.70137553959111,15.4954806762658,-1.74689558624962E-11));
#20349=CARTESIAN_POINT('Ctrl Pts',(7.27603165468577,15.6704806762658,-4.20081883448253));
#20350=CARTESIAN_POINT('Ctrl Pts',(4.85068776978043,15.8454806762658,-8.4016376689476));
#20351=CARTESIAN_POINT('Ctrl Pts',(-1.51301029103127E-11,16.0204806762658,
-8.40163766893887));
#20352=CARTESIAN_POINT('Ctrl Pts',(-4.85068776981069,16.1954806762658,-8.40163766893014));
#20353=CARTESIAN_POINT('Ctrl Pts',(-7.2760316547009,16.3704806762658,-4.20081883445633));
#20354=CARTESIAN_POINT('Ctrl Pts',(-9.70137553959111,16.5454806762658,1.74701439383464E-11));
#20355=CARTESIAN_POINT('Ctrl Pts',(-7.27603165468577,16.7204806762658,4.20081883448254));
#20356=CARTESIAN_POINT('Ctrl Pts',(-4.85068776978043,16.8954806762658,8.40163766894761));
#20357=CARTESIAN_POINT('Ctrl Pts',(1.51290740064448E-11,17.0704806762658,
8.40163766893887));
#20358=CARTESIAN_POINT('Ctrl Pts',(4.85068776981068,17.2454806762658,8.40163766893014));
#20359=CARTESIAN_POINT('Ctrl Pts',(7.2760316547009,17.4204806762658,4.20081883445634));
#20360=CARTESIAN_POINT('Ctrl Pts',(9.70137553959111,17.5954806762658,-1.74689558624962E-11));
#20361=CARTESIAN_POINT('Ctrl Pts',(7.27603165468577,17.7704806762658,-4.20081883448253));
#20362=CARTESIAN_POINT('Ctrl Pts',(4.85068776978043,17.9454806762658,-8.4016376689476));
#20363=CARTESIAN_POINT('Ctrl Pts',(-1.51301029103127E-11,18.1204806762658,
-8.40163766893887));
#20364=CARTESIAN_POINT('Ctrl Pts',(-4.85068776981069,18.2954806762658,-8.40163766893014));
#20365=CARTESIAN_POINT('Ctrl Pts',(-7.2760316547009,18.4704806762658,-4.20081883445633));
#20366=CARTESIAN_POINT('Ctrl Pts',(-9.70137553959111,18.6454806762658,1.74701439383464E-11));
#20367=CARTESIAN_POINT('Ctrl Pts',(-7.27603165468577,18.8204806762658,4.20081883448254));
#20368=CARTESIAN_POINT('Ctrl Pts',(-4.85068776978043,18.9954806762658,8.40163766894761));
#20369=CARTESIAN_POINT('Ctrl Pts',(1.51290740064448E-11,19.1704806762658,
8.40163766893887));
#20370=CARTESIAN_POINT('Ctrl Pts',(4.85068776981068,19.3454806762658,8.40163766893014));
#20371=CARTESIAN_POINT('Ctrl Pts',(7.2760316547009,19.5204806762658,4.20081883445634));
#20372=CARTESIAN_POINT('Ctrl Pts',(9.70137553959111,19.6954806762658,-1.74689558624962E-11));
#20373=CARTESIAN_POINT('Ctrl Pts',(7.27603165468577,19.8704806762658,-4.20081883448253));
#20374=CARTESIAN_POINT('Ctrl Pts',(4.85068776978043,20.0454806762658,-8.4016376689476));
#20375=CARTESIAN_POINT('Ctrl Pts',(-1.51301029103127E-11,20.2204806762658,
-8.40163766893887));
#20376=CARTESIAN_POINT('Ctrl Pts',(-4.85068776981069,20.3954806762658,-8.40163766893014));
#20377=CARTESIAN_POINT('Ctrl Pts',(-7.2760316547009,20.5704806762658,-4.20081883445633));
#20378=CARTESIAN_POINT('Ctrl Pts',(-9.70137553959111,20.7454806762658,1.74701439383464E-11));
#20379=CARTESIAN_POINT('Ctrl Pts',(-7.27603165468577,20.9204806762658,4.20081883448254));
#20380=CARTESIAN_POINT('Ctrl Pts',(-4.85068776978043,21.0954806762658,8.40163766894761));
#20381=CARTESIAN_POINT('Ctrl Pts',(1.51290740064448E-11,21.2704806762658,
8.40163766893887));
#20382=CARTESIAN_POINT('Ctrl Pts',(4.85068776981068,21.4454806762658,8.40163766893014));
#20383=CARTESIAN_POINT('Ctrl Pts',(7.2760316547009,21.6204806762658,4.20081883445634));
#20384=CARTESIAN_POINT('Ctrl Pts',(9.70137553959111,21.7954806762658,-1.74689558624962E-11));
#20385=CARTESIAN_POINT('Ctrl Pts',(7.27603165468577,21.9704806762658,-4.20081883448253));
#20386=CARTESIAN_POINT('Ctrl Pts',(4.85068776978043,22.1454806762658,-8.4016376689476));
#20387=CARTESIAN_POINT('Ctrl Pts',(-1.51301029103127E-11,22.3204806762658,
-8.40163766893887));
#20388=CARTESIAN_POINT('Ctrl Pts',(-4.85068776981069,22.4954806762658,-8.40163766893014));
#20389=CARTESIAN_POINT('Ctrl Pts',(-7.2760316547009,22.6704806762658,-4.20081883445633));
#20390=CARTESIAN_POINT('Ctrl Pts',(-9.70137553959111,22.8454806762658,1.74701439383464E-11));
#20391=CARTESIAN_POINT('Ctrl Pts',(-7.27603165468577,23.0204806762658,4.20081883448254));
#20392=CARTESIAN_POINT('Ctrl Pts',(-4.85068776978043,23.1954806762658,8.40163766894761));
#20393=CARTESIAN_POINT('Ctrl Pts',(1.51290740064448E-11,23.3704806762658,
8.40163766893887));
#20394=CARTESIAN_POINT('Ctrl Pts',(4.85068776981068,23.5454806762658,8.40163766893014));
#20395=CARTESIAN_POINT('Ctrl Pts',(7.2760316547009,23.7204806762658,4.20081883445634));
#20396=CARTESIAN_POINT('Ctrl Pts',(9.70137553959111,23.8954806762658,-1.74689558624962E-11));
#20397=CARTESIAN_POINT('Ctrl Pts',(7.27603165468577,24.0704806762658,-4.20081883448253));
#20398=CARTESIAN_POINT('Ctrl Pts',(4.85068776978043,24.2454806762658,-8.4016376689476));
#20399=CARTESIAN_POINT('Ctrl Pts',(-1.51301029103127E-11,24.4204806762658,
-8.40163766893887));
#20400=CARTESIAN_POINT('Ctrl Pts',(-4.85068776981069,24.5954806762658,-8.40163766893014));
#20401=CARTESIAN_POINT('Ctrl Pts',(-7.2760316547009,24.7704806762658,-4.20081883445633));
#20402=CARTESIAN_POINT('Ctrl Pts',(-9.70137553959111,24.9454806762658,1.74701439383464E-11));
#20403=CARTESIAN_POINT('Ctrl Pts',(-7.27603165468577,25.1204806762658,4.20081883448254));
#20404=CARTESIAN_POINT('Ctrl Pts',(-4.85068776978043,25.2954806762658,8.40163766894761));
#20405=CARTESIAN_POINT('Ctrl Pts',(1.51290740064448E-11,25.4704806762658,
8.40163766893887));
#20406=CARTESIAN_POINT('Ctrl Pts',(4.85068776981068,25.6454806762658,8.40163766893014));
#20407=CARTESIAN_POINT('Ctrl Pts',(7.2760316547009,25.8204806762658,4.20081883445634));
#20408=CARTESIAN_POINT('Ctrl Pts',(9.70137553959111,25.9954806762658,-1.74689558624962E-11));
#20409=CARTESIAN_POINT('Ctrl Pts',(7.27603165468577,26.1704806762658,-4.20081883448253));
#20410=CARTESIAN_POINT('Ctrl Pts',(4.85068776978043,26.3454806762658,-8.4016376689476));
#20411=CARTESIAN_POINT('Ctrl Pts',(-1.51301029103127E-11,26.5204806762658,
-8.40163766893887));
#20412=CARTESIAN_POINT('Ctrl Pts',(-1.78726082715848E-11,-142.78675111262,
-9.92453123331945));
#20413=CARTESIAN_POINT('Ctrl Pts',(-5.7299307791557,-142.61175111262,-9.92453123330913));
#20414=CARTESIAN_POINT('Ctrl Pts',(-8.59489616871569,-142.43675111262,-4.96226561664425));
#20415=CARTESIAN_POINT('Ctrl Pts',(-11.4598615582757,-142.26175111262,2.06368086793017E-11));
#20416=CARTESIAN_POINT('Ctrl Pts',(-8.59489616869782,-142.08675111262,4.9622656166752));
#20417=CARTESIAN_POINT('Ctrl Pts',(-5.72993077911996,-141.91175111262,9.92453123332977));
#20418=CARTESIAN_POINT('Ctrl Pts',(1.7871392867044E-11,-141.73675111262,
9.92453123331945));
#20419=CARTESIAN_POINT('Ctrl Pts',(5.7299307791557,-141.56175111262,9.92453123330913));
#20420=CARTESIAN_POINT('Ctrl Pts',(8.59489616871569,-141.38675111262,4.96226561664425));
#20421=CARTESIAN_POINT('Ctrl Pts',(11.4598615582757,-141.21175111262,-2.06354052510241E-11));
#20422=CARTESIAN_POINT('Ctrl Pts',(8.59489616869782,-141.03675111262,-4.9622656166752));
#20423=CARTESIAN_POINT('Ctrl Pts',(5.72993077911996,-140.86175111262,-9.92453123332976));
#20424=CARTESIAN_POINT('Ctrl Pts',(-1.78726082715848E-11,-140.68675111262,
-9.92453123331945));
#20425=CARTESIAN_POINT('Ctrl Pts',(-5.7299307791557,-140.51175111262,-9.92453123330913));
#20426=CARTESIAN_POINT('Ctrl Pts',(-8.59489616871569,-140.33675111262,-4.96226561664425));
#20427=CARTESIAN_POINT('Ctrl Pts',(-11.4598615582757,-140.16175111262,2.06368086793017E-11));
#20428=CARTESIAN_POINT('Ctrl Pts',(-8.59489616869782,-139.98675111262,4.9622656166752));
#20429=CARTESIAN_POINT('Ctrl Pts',(-5.72993077911996,-139.81175111262,9.92453123332977));
#20430=CARTESIAN_POINT('Ctrl Pts',(1.7871392867044E-11,-139.63675111262,
9.92453123331945));
#20431=CARTESIAN_POINT('Ctrl Pts',(5.7299307791557,-139.46175111262,9.92453123330913));
#20432=CARTESIAN_POINT('Ctrl Pts',(8.59489616871569,-139.28675111262,4.96226561664425));
#20433=CARTESIAN_POINT('Ctrl Pts',(11.4598615582757,-139.11175111262,-2.06354052510241E-11));
#20434=CARTESIAN_POINT('Ctrl Pts',(8.59489616869782,-138.93675111262,-4.9622656166752));
#20435=CARTESIAN_POINT('Ctrl Pts',(5.72993077911996,-138.76175111262,-9.92453123332976));
#20436=CARTESIAN_POINT('Ctrl Pts',(-1.78726082715848E-11,-138.58675111262,
-9.92453123331945));
#20437=CARTESIAN_POINT('Ctrl Pts',(-5.7299307791557,-138.41175111262,-9.92453123330913));
#20438=CARTESIAN_POINT('Ctrl Pts',(-8.59489616871569,-138.23675111262,-4.96226561664425));
#20439=CARTESIAN_POINT('Ctrl Pts',(-11.4598615582757,-138.06175111262,2.06368086793017E-11));
#20440=CARTESIAN_POINT('Ctrl Pts',(-8.59489616869782,-137.88675111262,4.9622656166752));
#20441=CARTESIAN_POINT('Ctrl Pts',(-5.72993077911996,-137.71175111262,9.92453123332977));
#20442=CARTESIAN_POINT('Ctrl Pts',(1.7871392867044E-11,-137.53675111262,
9.92453123331945));
#20443=CARTESIAN_POINT('Ctrl Pts',(5.7299307791557,-137.36175111262,9.92453123330913));
#20444=CARTESIAN_POINT('Ctrl Pts',(8.59489616871569,-137.18675111262,4.96226561664425));
#20445=CARTESIAN_POINT('Ctrl Pts',(11.4598615582757,-137.01175111262,-2.06354052510241E-11));
#20446=CARTESIAN_POINT('Ctrl Pts',(8.59489616869782,-136.83675111262,-4.9622656166752));
#20447=CARTESIAN_POINT('Ctrl Pts',(5.72993077911996,-136.66175111262,-9.92453123332976));
#20448=CARTESIAN_POINT('Ctrl Pts',(-1.78726082715848E-11,-136.48675111262,
-9.92453123331945));
#20449=CARTESIAN_POINT('Ctrl Pts',(-5.7299307791557,-136.31175111262,-9.92453123330913));
#20450=CARTESIAN_POINT('Ctrl Pts',(-8.59489616871569,-136.13675111262,-4.96226561664425));
#20451=CARTESIAN_POINT('Ctrl Pts',(-11.4598615582757,-135.96175111262,2.06368086793017E-11));
#20452=CARTESIAN_POINT('Ctrl Pts',(-8.59489616869782,-135.78675111262,4.9622656166752));
#20453=CARTESIAN_POINT('Ctrl Pts',(-5.72993077911996,-135.61175111262,9.92453123332977));
#20454=CARTESIAN_POINT('Ctrl Pts',(1.7871392867044E-11,-135.43675111262,
9.92453123331945));
#20455=CARTESIAN_POINT('Ctrl Pts',(5.7299307791557,-135.26175111262,9.92453123330913));
#20456=CARTESIAN_POINT('Ctrl Pts',(8.59489616871569,-135.08675111262,4.96226561664425));
#20457=CARTESIAN_POINT('Ctrl Pts',(11.4598615582757,-134.91175111262,-2.06354052510241E-11));
#20458=CARTESIAN_POINT('Ctrl Pts',(8.59489616869782,-134.73675111262,-4.9622656166752));
#20459=CARTESIAN_POINT('Ctrl Pts',(5.72993077911996,-134.56175111262,-9.92453123332976));
#20460=CARTESIAN_POINT('Ctrl Pts',(-1.78726082715848E-11,-134.38675111262,
-9.92453123331945));
#20461=CARTESIAN_POINT('Ctrl Pts',(-5.7299307791557,-134.21175111262,-9.92453123330913));
#20462=CARTESIAN_POINT('Ctrl Pts',(-8.59489616871569,-134.03675111262,-4.96226561664425));
#20463=CARTESIAN_POINT('Ctrl Pts',(-11.4598615582757,-133.86175111262,2.06368086793017E-11));
#20464=CARTESIAN_POINT('Ctrl Pts',(-8.59489616869782,-133.68675111262,4.9622656166752));
#20465=CARTESIAN_POINT('Ctrl Pts',(-5.72993077911996,-133.51175111262,9.92453123332977));
#20466=CARTESIAN_POINT('Ctrl Pts',(1.7871392867044E-11,-133.33675111262,
9.92453123331945));
#20467=CARTESIAN_POINT('Ctrl Pts',(5.7299307791557,-133.16175111262,9.92453123330913));
#20468=CARTESIAN_POINT('Ctrl Pts',(8.59489616871569,-132.98675111262,4.96226561664425));
#20469=CARTESIAN_POINT('Ctrl Pts',(11.4598615582757,-132.81175111262,-2.06354052510241E-11));
#20470=CARTESIAN_POINT('Ctrl Pts',(8.59489616869782,-132.63675111262,-4.9622656166752));
#20471=CARTESIAN_POINT('Ctrl Pts',(5.72993077911996,-132.46175111262,-9.92453123332976));
#20472=CARTESIAN_POINT('Ctrl Pts',(-1.78726082715848E-11,-132.28675111262,
-9.92453123331945));
#20473=CARTESIAN_POINT('Ctrl Pts',(-5.7299307791557,-132.11175111262,-9.92453123330913));
#20474=CARTESIAN_POINT('Ctrl Pts',(-8.59489616871569,-131.93675111262,-4.96226561664425));
#20475=CARTESIAN_POINT('Ctrl Pts',(-11.4598615582757,-131.76175111262,2.06368086793017E-11));
#20476=CARTESIAN_POINT('Ctrl Pts',(-8.59489616869782,-131.58675111262,4.9622656166752));
#20477=CARTESIAN_POINT('Ctrl Pts',(-5.72993077911996,-131.41175111262,9.92453123332977));
#20478=CARTESIAN_POINT('Ctrl Pts',(1.7871392867044E-11,-131.23675111262,
9.92453123331945));
#20479=CARTESIAN_POINT('Ctrl Pts',(5.7299307791557,-131.06175111262,9.92453123330913));
#20480=CARTESIAN_POINT('Ctrl Pts',(8.59489616871569,-130.88675111262,4.96226561664425));
#20481=CARTESIAN_POINT('Ctrl Pts',(11.4598615582757,-130.71175111262,-2.06354052510241E-11));
#20482=CARTESIAN_POINT('Ctrl Pts',(8.59489616869782,-130.53675111262,-4.9622656166752));
#20483=CARTESIAN_POINT('Ctrl Pts',(5.72993077911996,-130.36175111262,-9.92453123332976));
#20484=CARTESIAN_POINT('Ctrl Pts',(-1.78726082715848E-11,-130.18675111262,
-9.92453123331945));
#20485=CARTESIAN_POINT('Ctrl Pts',(-5.7299307791557,-130.01175111262,-9.92453123330913));
#20486=CARTESIAN_POINT('Ctrl Pts',(-8.59489616871569,-129.83675111262,-4.96226561664425));
#20487=CARTESIAN_POINT('Ctrl Pts',(-11.4598615582757,-129.66175111262,2.06368086793017E-11));
#20488=CARTESIAN_POINT('Ctrl Pts',(-8.59489616869782,-129.48675111262,4.9622656166752));
#20489=CARTESIAN_POINT('Ctrl Pts',(-5.72993077911996,-129.31175111262,9.92453123332977));
#20490=CARTESIAN_POINT('Ctrl Pts',(1.7871392867044E-11,-129.13675111262,
9.92453123331945));
#20491=CARTESIAN_POINT('Ctrl Pts',(5.7299307791557,-128.96175111262,9.92453123330913));
#20492=CARTESIAN_POINT('Ctrl Pts',(8.59489616871569,-128.78675111262,4.96226561664425));
#20493=CARTESIAN_POINT('Ctrl Pts',(11.4598615582757,-128.61175111262,-2.06354052510241E-11));
#20494=CARTESIAN_POINT('Ctrl Pts',(8.59489616869782,-128.43675111262,-4.9622656166752));
#20495=CARTESIAN_POINT('Ctrl Pts',(5.72993077911996,-128.26175111262,-9.92453123332976));
#20496=CARTESIAN_POINT('Ctrl Pts',(-1.78726082715848E-11,-128.08675111262,
-9.92453123331945));
#20497=CARTESIAN_POINT('Ctrl Pts',(-5.7299307791557,-127.91175111262,-9.92453123330913));
#20498=CARTESIAN_POINT('Ctrl Pts',(-8.59489616871569,-127.73675111262,-4.96226561664425));
#20499=CARTESIAN_POINT('Ctrl Pts',(-11.4598615582757,-127.56175111262,2.06368086793017E-11));
#20500=CARTESIAN_POINT('Ctrl Pts',(-8.59489616869782,-127.38675111262,4.9622656166752));
#20501=CARTESIAN_POINT('Ctrl Pts',(-5.72993077911996,-127.21175111262,9.92453123332977));
#20502=CARTESIAN_POINT('Ctrl Pts',(1.7871392867044E-11,-127.03675111262,
9.92453123331945));
#20503=CARTESIAN_POINT('Ctrl Pts',(5.7299307791557,-126.86175111262,9.92453123330913));
#20504=CARTESIAN_POINT('Ctrl Pts',(8.59489616871569,-126.68675111262,4.96226561664425));
#20505=CARTESIAN_POINT('Ctrl Pts',(11.4598615582757,-126.51175111262,-2.06354052510241E-11));
#20506=CARTESIAN_POINT('Ctrl Pts',(8.59489616869782,-126.33675111262,-4.9622656166752));
#20507=CARTESIAN_POINT('Ctrl Pts',(5.72993077911996,-126.16175111262,-9.92453123332976));
#20508=CARTESIAN_POINT('Ctrl Pts',(-1.78726082715848E-11,-125.98675111262,
-9.92453123331945));
#20509=CARTESIAN_POINT('Ctrl Pts',(-5.7299307791557,-125.81175111262,-9.92453123330913));
#20510=CARTESIAN_POINT('Ctrl Pts',(-8.59489616871569,-125.63675111262,-4.96226561664425));
#20511=CARTESIAN_POINT('Ctrl Pts',(-11.4598615582757,-125.46175111262,2.06368086793017E-11));
#20512=CARTESIAN_POINT('Ctrl Pts',(-8.59489616869782,-125.28675111262,4.9622656166752));
#20513=CARTESIAN_POINT('Ctrl Pts',(-5.72993077911996,-125.11175111262,9.92453123332977));
#20514=CARTESIAN_POINT('Ctrl Pts',(1.7871392867044E-11,-124.93675111262,
9.92453123331945));
#20515=CARTESIAN_POINT('Ctrl Pts',(5.7299307791557,-124.76175111262,9.92453123330913));
#20516=CARTESIAN_POINT('Ctrl Pts',(8.59489616871569,-124.58675111262,4.96226561664425));
#20517=CARTESIAN_POINT('Ctrl Pts',(11.4598615582757,-124.41175111262,-2.06354052510241E-11));
#20518=CARTESIAN_POINT('Ctrl Pts',(8.59489616869782,-124.23675111262,-4.9622656166752));
#20519=CARTESIAN_POINT('Ctrl Pts',(5.72993077911996,-124.06175111262,-9.92453123332976));
#20520=CARTESIAN_POINT('Ctrl Pts',(-1.78726082715848E-11,-123.88675111262,
-9.92453123331945));
#20521=CARTESIAN_POINT('Ctrl Pts',(-5.7299307791557,-123.71175111262,-9.92453123330913));
#20522=CARTESIAN_POINT('Ctrl Pts',(-8.59489616871569,-123.53675111262,-4.96226561664425));
#20523=CARTESIAN_POINT('Ctrl Pts',(-11.4598615582757,-123.36175111262,2.06368086793017E-11));
#20524=CARTESIAN_POINT('Ctrl Pts',(-8.59489616869782,-123.18675111262,4.9622656166752));
#20525=CARTESIAN_POINT('Ctrl Pts',(-5.72993077911996,-123.01175111262,9.92453123332977));
#20526=CARTESIAN_POINT('Ctrl Pts',(1.7871392867044E-11,-122.83675111262,
9.92453123331945));
#20527=CARTESIAN_POINT('Ctrl Pts',(5.7299307791557,-122.66175111262,9.92453123330913));
#20528=CARTESIAN_POINT('Ctrl Pts',(8.59489616871569,-122.48675111262,4.96226561664425));
#20529=CARTESIAN_POINT('Ctrl Pts',(11.4598615582757,-122.31175111262,-2.06354052510241E-11));
#20530=CARTESIAN_POINT('Ctrl Pts',(8.59489616869782,-122.13675111262,-4.9622656166752));
#20531=CARTESIAN_POINT('Ctrl Pts',(5.72993077911996,-121.96175111262,-9.92453123332976));
#20532=CARTESIAN_POINT('Ctrl Pts',(-1.78726082715848E-11,-121.78675111262,
-9.92453123331945));
#20533=CARTESIAN_POINT('Ctrl Pts',(-5.7299307791557,-121.61175111262,-9.92453123330913));
#20534=CARTESIAN_POINT('Ctrl Pts',(-8.59489616871569,-121.43675111262,-4.96226561664425));
#20535=CARTESIAN_POINT('Ctrl Pts',(-11.4598615582757,-121.26175111262,2.06368086793017E-11));
#20536=CARTESIAN_POINT('Ctrl Pts',(-8.59489616869782,-121.08675111262,4.9622656166752));
#20537=CARTESIAN_POINT('Ctrl Pts',(-5.72993077911996,-120.91175111262,9.92453123332977));
#20538=CARTESIAN_POINT('Ctrl Pts',(1.7871392867044E-11,-120.73675111262,
9.92453123331945));
#20539=CARTESIAN_POINT('Ctrl Pts',(5.7299307791557,-120.56175111262,9.92453123330913));
#20540=CARTESIAN_POINT('Ctrl Pts',(8.59489616871569,-120.38675111262,4.96226561664425));
#20541=CARTESIAN_POINT('Ctrl Pts',(11.4598615582757,-120.21175111262,-2.06354052510241E-11));
#20542=CARTESIAN_POINT('Ctrl Pts',(8.59489616869782,-120.03675111262,-4.9622656166752));
#20543=CARTESIAN_POINT('Ctrl Pts',(5.72993077911996,-119.86175111262,-9.92453123332976));
#20544=CARTESIAN_POINT('Ctrl Pts',(-1.78726082715848E-11,-119.68675111262,
-9.92453123331945));
#20545=CARTESIAN_POINT('Ctrl Pts',(-5.7299307791557,-119.51175111262,-9.92453123330913));
#20546=CARTESIAN_POINT('Ctrl Pts',(-8.59489616871569,-119.33675111262,-4.96226561664425));
#20547=CARTESIAN_POINT('Ctrl Pts',(-11.4598615582757,-119.16175111262,2.06368086793017E-11));
#20548=CARTESIAN_POINT('Ctrl Pts',(-8.59489616869782,-118.98675111262,4.9622656166752));
#20549=CARTESIAN_POINT('Ctrl Pts',(-5.72993077911996,-118.81175111262,9.92453123332977));
#20550=CARTESIAN_POINT('Ctrl Pts',(1.7871392867044E-11,-118.63675111262,
9.92453123331945));
#20551=CARTESIAN_POINT('Ctrl Pts',(5.7299307791557,-118.46175111262,9.92453123330913));
#20552=CARTESIAN_POINT('Ctrl Pts',(8.59489616871569,-118.28675111262,4.96226561664425));
#20553=CARTESIAN_POINT('Ctrl Pts',(11.4598615582757,-118.11175111262,-2.06354052510241E-11));
#20554=CARTESIAN_POINT('Ctrl Pts',(8.59489616869782,-117.93675111262,-4.9622656166752));
#20555=CARTESIAN_POINT('Ctrl Pts',(5.72993077911996,-117.76175111262,-9.92453123332976));
#20556=CARTESIAN_POINT('Ctrl Pts',(-1.78726082715848E-11,-117.58675111262,
-9.92453123331945));
#20557=CARTESIAN_POINT('Ctrl Pts',(-5.7299307791557,-117.41175111262,-9.92453123330913));
#20558=CARTESIAN_POINT('Ctrl Pts',(-8.59489616871569,-117.23675111262,-4.96226561664425));
#20559=CARTESIAN_POINT('Ctrl Pts',(-11.4598615582757,-117.06175111262,2.06368086793017E-11));
#20560=CARTESIAN_POINT('Ctrl Pts',(-8.59489616869782,-116.88675111262,4.9622656166752));
#20561=CARTESIAN_POINT('Ctrl Pts',(-5.72993077911996,-116.71175111262,9.92453123332977));
#20562=CARTESIAN_POINT('Ctrl Pts',(1.7871392867044E-11,-116.53675111262,
9.92453123331945));
#20563=CARTESIAN_POINT('Ctrl Pts',(5.7299307791557,-116.36175111262,9.92453123330913));
#20564=CARTESIAN_POINT('Ctrl Pts',(8.59489616871569,-116.18675111262,4.96226561664425));
#20565=CARTESIAN_POINT('Ctrl Pts',(11.4598615582757,-116.01175111262,-2.06354052510241E-11));
#20566=CARTESIAN_POINT('Ctrl Pts',(8.59489616869782,-115.83675111262,-4.9622656166752));
#20567=CARTESIAN_POINT('Ctrl Pts',(5.72993077911996,-115.66175111262,-9.92453123332976));
#20568=CARTESIAN_POINT('Ctrl Pts',(-1.78726082715848E-11,-115.48675111262,
-9.92453123331945));
#20569=CARTESIAN_POINT('Ctrl Pts',(-5.7299307791557,-115.31175111262,-9.92453123330913));
#20570=CARTESIAN_POINT('Ctrl Pts',(-8.59489616871569,-115.13675111262,-4.96226561664425));
#20571=CARTESIAN_POINT('Ctrl Pts',(-11.4598615582757,-114.96175111262,2.06368086793017E-11));
#20572=CARTESIAN_POINT('Ctrl Pts',(-8.59489616869782,-114.78675111262,4.9622656166752));
#20573=CARTESIAN_POINT('Ctrl Pts',(-5.72993077911996,-114.61175111262,9.92453123332977));
#20574=CARTESIAN_POINT('Ctrl Pts',(1.7871392867044E-11,-114.43675111262,
9.92453123331945));
#20575=CARTESIAN_POINT('Ctrl Pts',(5.7299307791557,-114.26175111262,9.92453123330913));
#20576=CARTESIAN_POINT('Ctrl Pts',(8.59489616871569,-114.08675111262,4.96226561664425));
#20577=CARTESIAN_POINT('Ctrl Pts',(11.4598615582757,-113.91175111262,-2.06354052510241E-11));
#20578=CARTESIAN_POINT('Ctrl Pts',(8.59489616869782,-113.73675111262,-4.9622656166752));
#20579=CARTESIAN_POINT('Ctrl Pts',(5.72993077911996,-113.56175111262,-9.92453123332976));
#20580=CARTESIAN_POINT('Ctrl Pts',(-1.78726082715848E-11,-113.38675111262,
-9.92453123331945));
#20581=CARTESIAN_POINT('Ctrl Pts',(-5.7299307791557,-113.21175111262,-9.92453123330913));
#20582=CARTESIAN_POINT('Ctrl Pts',(-8.59489616871569,-113.03675111262,-4.96226561664425));
#20583=CARTESIAN_POINT('Ctrl Pts',(-11.4598615582757,-112.86175111262,2.06368086793017E-11));
#20584=CARTESIAN_POINT('Ctrl Pts',(-8.59489616869782,-112.68675111262,4.9622656166752));
#20585=CARTESIAN_POINT('Ctrl Pts',(-5.72993077911996,-112.51175111262,9.92453123332977));
#20586=CARTESIAN_POINT('Ctrl Pts',(1.7871392867044E-11,-112.33675111262,
9.92453123331945));
#20587=CARTESIAN_POINT('Ctrl Pts',(5.7299307791557,-112.16175111262,9.92453123330913));
#20588=CARTESIAN_POINT('Ctrl Pts',(8.59489616871569,-111.98675111262,4.96226561664425));
#20589=CARTESIAN_POINT('Ctrl Pts',(11.4598615582757,-111.81175111262,-2.06354052510241E-11));
#20590=CARTESIAN_POINT('Ctrl Pts',(8.59489616869782,-111.63675111262,-4.9622656166752));
#20591=CARTESIAN_POINT('Ctrl Pts',(5.72993077911996,-111.46175111262,-9.92453123332976));
#20592=CARTESIAN_POINT('Ctrl Pts',(-1.78726082715848E-11,-111.28675111262,
-9.92453123331945));
#20593=CARTESIAN_POINT('Ctrl Pts',(-5.7299307791557,-111.11175111262,-9.92453123330913));
#20594=CARTESIAN_POINT('Ctrl Pts',(-8.59489616871569,-110.93675111262,-4.96226561664425));
#20595=CARTESIAN_POINT('Ctrl Pts',(-11.4598615582757,-110.76175111262,2.06368086793017E-11));
#20596=CARTESIAN_POINT('Ctrl Pts',(-8.59489616869782,-110.58675111262,4.9622656166752));
#20597=CARTESIAN_POINT('Ctrl Pts',(-5.72993077911996,-110.41175111262,9.92453123332977));
#20598=CARTESIAN_POINT('Ctrl Pts',(1.7871392867044E-11,-110.23675111262,
9.92453123331945));
#20599=CARTESIAN_POINT('Ctrl Pts',(5.7299307791557,-110.06175111262,9.92453123330913));
#20600=CARTESIAN_POINT('Ctrl Pts',(8.59489616871569,-109.88675111262,4.96226561664425));
#20601=CARTESIAN_POINT('Ctrl Pts',(11.4598615582757,-109.71175111262,-2.06354052510241E-11));
#20602=CARTESIAN_POINT('Ctrl Pts',(8.59489616869782,-109.53675111262,-4.9622656166752));
#20603=CARTESIAN_POINT('Ctrl Pts',(5.72993077911996,-109.36175111262,-9.92453123332976));
#20604=CARTESIAN_POINT('Ctrl Pts',(-1.78726082715848E-11,-109.18675111262,
-9.92453123331945));
#20605=CARTESIAN_POINT('Ctrl Pts',(-5.7299307791557,-109.01175111262,-9.92453123330913));
#20606=CARTESIAN_POINT('Ctrl Pts',(-8.59489616871569,-108.83675111262,-4.96226561664425));
#20607=CARTESIAN_POINT('Ctrl Pts',(-11.4598615582757,-108.66175111262,2.06368086793017E-11));
#20608=CARTESIAN_POINT('Ctrl Pts',(-8.59489616869782,-108.48675111262,4.9622656166752));
#20609=CARTESIAN_POINT('Ctrl Pts',(-5.72993077911996,-108.31175111262,9.92453123332977));
#20610=CARTESIAN_POINT('Ctrl Pts',(1.7871392867044E-11,-108.13675111262,
9.92453123331945));
#20611=CARTESIAN_POINT('Ctrl Pts',(5.7299307791557,-107.96175111262,9.92453123330913));
#20612=CARTESIAN_POINT('Ctrl Pts',(8.59489616871569,-107.78675111262,4.96226561664425));
#20613=CARTESIAN_POINT('Ctrl Pts',(11.4598615582757,-107.61175111262,-2.06354052510241E-11));
#20614=CARTESIAN_POINT('Ctrl Pts',(8.59489616869782,-107.43675111262,-4.9622656166752));
#20615=CARTESIAN_POINT('Ctrl Pts',(5.72993077911996,-107.26175111262,-9.92453123332976));
#20616=CARTESIAN_POINT('Ctrl Pts',(-1.78726082715848E-11,-107.08675111262,
-9.92453123331945));
#20617=CARTESIAN_POINT('Ctrl Pts',(-5.7299307791557,-106.91175111262,-9.92453123330913));
#20618=CARTESIAN_POINT('Ctrl Pts',(-8.59489616871569,-106.73675111262,-4.96226561664425));
#20619=CARTESIAN_POINT('Ctrl Pts',(-11.4598615582757,-106.56175111262,2.06368086793017E-11));
#20620=CARTESIAN_POINT('Ctrl Pts',(-8.59489616869782,-106.38675111262,4.9622656166752));
#20621=CARTESIAN_POINT('Ctrl Pts',(-5.72993077911996,-106.21175111262,9.92453123332977));
#20622=CARTESIAN_POINT('Ctrl Pts',(1.7871392867044E-11,-106.03675111262,
9.92453123331945));
#20623=CARTESIAN_POINT('Ctrl Pts',(5.7299307791557,-105.86175111262,9.92453123330913));
#20624=CARTESIAN_POINT('Ctrl Pts',(8.59489616871569,-105.68675111262,4.96226561664425));
#20625=CARTESIAN_POINT('Ctrl Pts',(11.4598615582757,-105.51175111262,-2.06354052510241E-11));
#20626=CARTESIAN_POINT('Ctrl Pts',(8.59489616869782,-105.33675111262,-4.9622656166752));
#20627=CARTESIAN_POINT('Ctrl Pts',(5.72993077911996,-105.16175111262,-9.92453123332976));
#20628=CARTESIAN_POINT('Ctrl Pts',(-1.78726082715848E-11,-104.98675111262,
-9.92453123331945));
#20629=CARTESIAN_POINT('Ctrl Pts',(-5.7299307791557,-104.81175111262,-9.92453123330913));
#20630=CARTESIAN_POINT('Ctrl Pts',(-8.59489616871569,-104.63675111262,-4.96226561664425));
#20631=CARTESIAN_POINT('Ctrl Pts',(-11.4598615582757,-104.46175111262,2.06368086793017E-11));
#20632=CARTESIAN_POINT('Ctrl Pts',(-8.59489616869782,-104.28675111262,4.9622656166752));
#20633=CARTESIAN_POINT('Ctrl Pts',(-5.72993077911996,-104.11175111262,9.92453123332977));
#20634=CARTESIAN_POINT('Ctrl Pts',(1.7871392867044E-11,-103.93675111262,
9.92453123331945));
#20635=CARTESIAN_POINT('Ctrl Pts',(5.7299307791557,-103.76175111262,9.92453123330913));
#20636=CARTESIAN_POINT('Ctrl Pts',(8.59489616871569,-103.58675111262,4.96226561664425));
#20637=CARTESIAN_POINT('Ctrl Pts',(11.4598615582757,-103.41175111262,-2.06354052510241E-11));
#20638=CARTESIAN_POINT('Ctrl Pts',(8.59489616869782,-103.23675111262,-4.9622656166752));
#20639=CARTESIAN_POINT('Ctrl Pts',(5.72993077911996,-103.06175111262,-9.92453123332976));
#20640=CARTESIAN_POINT('Ctrl Pts',(-1.78726082715848E-11,-102.88675111262,
-9.92453123331945));
#20641=CARTESIAN_POINT('Ctrl Pts',(-5.7299307791557,-102.71175111262,-9.92453123330913));
#20642=CARTESIAN_POINT('Ctrl Pts',(-8.59489616871569,-102.53675111262,-4.96226561664425));
#20643=CARTESIAN_POINT('Ctrl Pts',(-11.4598615582757,-102.36175111262,2.06368086793017E-11));
#20644=CARTESIAN_POINT('Ctrl Pts',(-8.59489616869782,-102.18675111262,4.9622656166752));
#20645=CARTESIAN_POINT('Ctrl Pts',(-5.72993077911996,-102.01175111262,9.92453123332977));
#20646=CARTESIAN_POINT('Ctrl Pts',(1.7871392867044E-11,-101.83675111262,
9.92453123331945));
#20647=CARTESIAN_POINT('Ctrl Pts',(5.7299307791557,-101.66175111262,9.92453123330913));
#20648=CARTESIAN_POINT('Ctrl Pts',(8.59489616871569,-101.48675111262,4.96226561664425));
#20649=CARTESIAN_POINT('Ctrl Pts',(11.4598615582757,-101.31175111262,-2.06354052510241E-11));
#20650=CARTESIAN_POINT('Ctrl Pts',(8.59489616869782,-101.13675111262,-4.9622656166752));
#20651=CARTESIAN_POINT('Ctrl Pts',(5.72993077911996,-100.96175111262,-9.92453123332976));
#20652=CARTESIAN_POINT('Ctrl Pts',(-1.78726082715848E-11,-100.78675111262,
-9.92453123331945));
#20653=CARTESIAN_POINT('Ctrl Pts',(-5.7299307791557,-100.61175111262,-9.92453123330913));
#20654=CARTESIAN_POINT('Ctrl Pts',(-8.59489616871569,-100.43675111262,-4.96226561664425));
#20655=CARTESIAN_POINT('Ctrl Pts',(-11.4598615582757,-100.26175111262,2.06368086793017E-11));
#20656=CARTESIAN_POINT('Ctrl Pts',(-8.59489616869782,-100.08675111262,4.9622656166752));
#20657=CARTESIAN_POINT('Ctrl Pts',(-5.72993077911996,-99.91175111262,9.92453123332977));
#20658=CARTESIAN_POINT('Ctrl Pts',(1.7871392867044E-11,-99.7367511126201,
9.92453123331945));
#20659=CARTESIAN_POINT('Ctrl Pts',(5.7299307791557,-99.5617511126201,9.92453123330913));
#20660=CARTESIAN_POINT('Ctrl Pts',(8.59489616871569,-99.3867511126201,4.96226561664425));
#20661=CARTESIAN_POINT('Ctrl Pts',(11.4598615582757,-99.2117511126201,-2.06354052510241E-11));
#20662=CARTESIAN_POINT('Ctrl Pts',(8.59489616869782,-99.0367511126201,-4.9622656166752));
#20663=CARTESIAN_POINT('Ctrl Pts',(5.72993077911996,-98.8617511126201,-9.92453123332976));
#20664=CARTESIAN_POINT('Ctrl Pts',(-1.78726082715848E-11,-98.6867511126201,
-9.92453123331945));
#20665=CARTESIAN_POINT('Ctrl Pts',(-5.7299307791557,-98.5117511126201,-9.92453123330913));
#20666=CARTESIAN_POINT('Ctrl Pts',(-8.59489616871569,-98.33675111262,-4.96226561664425));
#20667=CARTESIAN_POINT('Ctrl Pts',(-11.4598615582757,-98.16175111262,2.06368086793017E-11));
#20668=CARTESIAN_POINT('Ctrl Pts',(-8.59489616869782,-97.9867511126201,
4.9622656166752));
#20669=CARTESIAN_POINT('Ctrl Pts',(-5.72993077911996,-97.81175111262,9.92453123332977));
#20670=CARTESIAN_POINT('Ctrl Pts',(1.7871392867044E-11,-97.6367511126201,
9.92453123331945));
#20671=CARTESIAN_POINT('Ctrl Pts',(5.7299307791557,-97.46175111262,9.92453123330913));
#20672=CARTESIAN_POINT('Ctrl Pts',(8.59489616871569,-97.2867511126201,4.96226561664425));
#20673=CARTESIAN_POINT('Ctrl Pts',(11.4598615582757,-97.1117511126201,-2.06354052510241E-11));
#20674=CARTESIAN_POINT('Ctrl Pts',(8.59489616869782,-96.9367511126201,-4.9622656166752));
#20675=CARTESIAN_POINT('Ctrl Pts',(5.72993077911996,-96.7617511126201,-9.92453123332976));
#20676=CARTESIAN_POINT('Ctrl Pts',(-1.78726082715848E-11,-96.5867511126201,
-9.92453123331945));
#20677=CARTESIAN_POINT('Ctrl Pts',(-5.7299307791557,-96.4117511126201,-9.92453123330913));
#20678=CARTESIAN_POINT('Ctrl Pts',(-8.59489616871569,-96.2367511126201,
-4.96226561664425));
#20679=CARTESIAN_POINT('Ctrl Pts',(-11.4598615582757,-96.0617511126201,
2.06368086793017E-11));
#20680=CARTESIAN_POINT('Ctrl Pts',(-8.59489616869782,-95.8867511126201,
4.9622656166752));
#20681=CARTESIAN_POINT('Ctrl Pts',(-5.72993077911996,-95.7117511126201,
9.92453123332977));
#20682=CARTESIAN_POINT('Ctrl Pts',(1.7871392867044E-11,-95.5367511126201,
9.92453123331945));
#20683=CARTESIAN_POINT('Ctrl Pts',(5.7299307791557,-95.3617511126201,9.92453123330913));
#20684=CARTESIAN_POINT('Ctrl Pts',(8.59489616871569,-95.1867511126201,4.96226561664425));
#20685=CARTESIAN_POINT('Ctrl Pts',(11.4598615582757,-95.0117511126201,-2.06354052510241E-11));
#20686=CARTESIAN_POINT('Ctrl Pts',(8.59489616869782,-94.8367511126201,-4.9622656166752));
#20687=CARTESIAN_POINT('Ctrl Pts',(5.72993077911996,-94.6617511126201,-9.92453123332976));
#20688=CARTESIAN_POINT('Ctrl Pts',(-1.78726082715848E-11,-94.4867511126201,
-9.92453123331945));
#20689=CARTESIAN_POINT('Ctrl Pts',(-5.7299307791557,-94.3117511126201,-9.92453123330913));
#20690=CARTESIAN_POINT('Ctrl Pts',(-8.59489616871569,-94.1367511126201,
-4.96226561664425));
#20691=CARTESIAN_POINT('Ctrl Pts',(-11.4598615582757,-93.9617511126201,
2.06368086793017E-11));
#20692=CARTESIAN_POINT('Ctrl Pts',(-8.59489616869782,-93.7867511126201,
4.9622656166752));
#20693=CARTESIAN_POINT('Ctrl Pts',(-5.72993077911996,-93.6117511126201,
9.92453123332977));
#20694=CARTESIAN_POINT('Ctrl Pts',(1.7871392867044E-11,-93.4367511126201,
9.92453123331945));
#20695=CARTESIAN_POINT('Ctrl Pts',(5.7299307791557,-93.2617511126201,9.92453123330913));
#20696=CARTESIAN_POINT('Ctrl Pts',(8.59489616871569,-93.0867511126201,4.96226561664425));
#20697=CARTESIAN_POINT('Ctrl Pts',(11.4598615582757,-92.9117511126201,-2.06354052510241E-11));
#20698=CARTESIAN_POINT('Ctrl Pts',(8.59489616869782,-92.7367511126201,-4.9622656166752));
#20699=CARTESIAN_POINT('Ctrl Pts',(5.72993077911996,-92.5617511126201,-9.92453123332976));
#20700=CARTESIAN_POINT('Ctrl Pts',(-1.78726082715848E-11,-92.3867511126201,
-9.92453123331945));
#20701=CARTESIAN_POINT('Ctrl Pts',(-5.7299307791557,-92.2117511126201,-9.92453123330913));
#20702=CARTESIAN_POINT('Ctrl Pts',(-8.59489616871569,-92.0367511126201,
-4.96226561664425));
#20703=CARTESIAN_POINT('Ctrl Pts',(-11.4598615582757,-91.8617511126201,
2.06368086793017E-11));
#20704=CARTESIAN_POINT('Ctrl Pts',(-8.59489616869782,-91.6867511126201,
4.9622656166752));
#20705=CARTESIAN_POINT('Ctrl Pts',(-5.72993077911996,-91.5117511126201,
9.92453123332977));
#20706=CARTESIAN_POINT('Ctrl Pts',(1.7871392867044E-11,-91.3367511126201,
9.92453123331945));
#20707=CARTESIAN_POINT('Ctrl Pts',(5.7299307791557,-91.1617511126201,9.92453123330913));
#20708=CARTESIAN_POINT('Ctrl Pts',(8.59489616871569,-90.9867511126201,4.96226561664425));
#20709=CARTESIAN_POINT('Ctrl Pts',(11.4598615582757,-90.8117511126201,-2.06354052510241E-11));
#20710=CARTESIAN_POINT('Ctrl Pts',(8.59489616869782,-90.6367511126201,-4.9622656166752));
#20711=CARTESIAN_POINT('Ctrl Pts',(5.72993077911996,-90.4617511126201,-9.92453123332976));
#20712=CARTESIAN_POINT('Ctrl Pts',(-1.78726082715848E-11,-90.2867511126201,
-9.92453123331945));
#20713=CARTESIAN_POINT('Ctrl Pts',(-5.7299307791557,-90.1117511126201,-9.92453123330913));
#20714=CARTESIAN_POINT('Ctrl Pts',(-8.59489616871569,-89.9367511126201,
-4.96226561664425));
#20715=CARTESIAN_POINT('Ctrl Pts',(-11.4598615582757,-89.7617511126201,
2.06368086793017E-11));
#20716=CARTESIAN_POINT('Ctrl Pts',(-8.59489616869782,-89.5867511126201,
4.9622656166752));
#20717=CARTESIAN_POINT('Ctrl Pts',(-5.72993077911996,-89.4117511126201,
9.92453123332977));
#20718=CARTESIAN_POINT('Ctrl Pts',(1.7871392867044E-11,-89.2367511126201,
9.92453123331945));
#20719=CARTESIAN_POINT('Ctrl Pts',(5.7299307791557,-89.0617511126201,9.92453123330913));
#20720=CARTESIAN_POINT('Ctrl Pts',(8.59489616871569,-88.8867511126201,4.96226561664425));
#20721=CARTESIAN_POINT('Ctrl Pts',(11.4598615582757,-88.7117511126201,-2.06354052510241E-11));
#20722=CARTESIAN_POINT('Ctrl Pts',(8.59489616869782,-88.5367511126201,-4.9622656166752));
#20723=CARTESIAN_POINT('Ctrl Pts',(5.72993077911996,-88.3617511126201,-9.92453123332976));
#20724=CARTESIAN_POINT('Ctrl Pts',(-1.78726082715848E-11,-88.1867511126201,
-9.92453123331945));
#20725=CARTESIAN_POINT('Ctrl Pts',(-5.7299307791557,-88.0117511126201,-9.92453123330913));
#20726=CARTESIAN_POINT('Ctrl Pts',(-8.59489616871569,-87.8367511126201,
-4.96226561664425));
#20727=CARTESIAN_POINT('Ctrl Pts',(-11.4598615582757,-87.6617511126201,
2.06368086793017E-11));
#20728=CARTESIAN_POINT('Ctrl Pts',(-8.59489616869782,-87.4867511126201,
4.9622656166752));
#20729=CARTESIAN_POINT('Ctrl Pts',(-5.72993077911996,-87.3117511126201,
9.92453123332977));
#20730=CARTESIAN_POINT('Ctrl Pts',(1.7871392867044E-11,-87.1367511126201,
9.92453123331945));
#20731=CARTESIAN_POINT('Ctrl Pts',(5.7299307791557,-86.9617511126201,9.92453123330913));
#20732=CARTESIAN_POINT('Ctrl Pts',(8.59489616871569,-86.7867511126201,4.96226561664425));
#20733=CARTESIAN_POINT('Ctrl Pts',(11.4598615582757,-86.6117511126201,-2.06354052510241E-11));
#20734=CARTESIAN_POINT('Ctrl Pts',(8.59489616869782,-86.4367511126201,-4.9622656166752));
#20735=CARTESIAN_POINT('Ctrl Pts',(5.72993077911996,-86.2617511126201,-9.92453123332976));
#20736=CARTESIAN_POINT('Ctrl Pts',(-1.78726082715848E-11,-86.0867511126201,
-9.92453123331945));
#20737=CARTESIAN_POINT('Ctrl Pts',(-5.7299307791557,-85.9117511126201,-9.92453123330913));
#20738=CARTESIAN_POINT('Ctrl Pts',(-8.59489616871569,-85.7367511126201,
-4.96226561664425));
#20739=CARTESIAN_POINT('Ctrl Pts',(-11.4598615582757,-85.5617511126201,
2.06368086793017E-11));
#20740=CARTESIAN_POINT('Ctrl Pts',(-8.59489616869782,-85.3867511126201,
4.9622656166752));
#20741=CARTESIAN_POINT('Ctrl Pts',(-5.72993077911996,-85.2117511126201,
9.92453123332977));
#20742=CARTESIAN_POINT('Ctrl Pts',(1.7871392867044E-11,-85.0367511126201,
9.92453123331945));
#20743=CARTESIAN_POINT('Ctrl Pts',(5.7299307791557,-84.8617511126201,9.92453123330913));
#20744=CARTESIAN_POINT('Ctrl Pts',(8.59489616871569,-84.6867511126201,4.96226561664425));
#20745=CARTESIAN_POINT('Ctrl Pts',(11.4598615582757,-84.5117511126201,-2.06354052510241E-11));
#20746=CARTESIAN_POINT('Ctrl Pts',(8.59489616869782,-84.3367511126201,-4.9622656166752));
#20747=CARTESIAN_POINT('Ctrl Pts',(5.72993077911996,-84.1617511126201,-9.92453123332976));
#20748=CARTESIAN_POINT('Ctrl Pts',(-1.78726082715848E-11,-83.9867511126201,
-9.92453123331945));
#20749=CARTESIAN_POINT('Ctrl Pts',(-5.7299307791557,-83.8117511126201,-9.92453123330913));
#20750=CARTESIAN_POINT('Ctrl Pts',(-8.59489616871569,-83.6367511126201,
-4.96226561664425));
#20751=CARTESIAN_POINT('Ctrl Pts',(-11.4598615582757,-83.4617511126201,
2.06368086793017E-11));
#20752=CARTESIAN_POINT('Ctrl Pts',(-8.59489616869782,-83.2867511126201,
4.9622656166752));
#20753=CARTESIAN_POINT('Ctrl Pts',(-5.72993077911996,-83.1117511126201,
9.92453123332977));
#20754=CARTESIAN_POINT('Ctrl Pts',(1.7871392867044E-11,-82.9367511126201,
9.92453123331945));
#20755=CARTESIAN_POINT('Ctrl Pts',(5.7299307791557,-82.7617511126201,9.92453123330913));
#20756=CARTESIAN_POINT('Ctrl Pts',(8.59489616871569,-82.5867511126201,4.96226561664425));
#20757=CARTESIAN_POINT('Ctrl Pts',(11.4598615582757,-82.4117511126201,-2.06354052510241E-11));
#20758=CARTESIAN_POINT('Ctrl Pts',(8.59489616869782,-82.2367511126201,-4.9622656166752));
#20759=CARTESIAN_POINT('Ctrl Pts',(5.72993077911996,-82.0617511126201,-9.92453123332976));
#20760=CARTESIAN_POINT('Ctrl Pts',(-1.78726082715848E-11,-81.8867511126201,
-9.92453123331945));
#20761=CARTESIAN_POINT('Ctrl Pts',(-5.7299307791557,-81.7117511126201,-9.92453123330913));
#20762=CARTESIAN_POINT('Ctrl Pts',(-8.59489616871569,-81.5367511126201,
-4.96226561664425));
#20763=CARTESIAN_POINT('Ctrl Pts',(-11.4598615582757,-81.3617511126201,
2.06368086793017E-11));
#20764=CARTESIAN_POINT('Ctrl Pts',(-8.59489616869782,-81.1867511126201,
4.9622656166752));
#20765=CARTESIAN_POINT('Ctrl Pts',(-5.72993077911996,-81.0117511126201,
9.92453123332977));
#20766=CARTESIAN_POINT('Ctrl Pts',(1.7871392867044E-11,-80.8367511126201,
9.92453123331945));
#20767=CARTESIAN_POINT('Ctrl Pts',(5.7299307791557,-80.6617511126201,9.92453123330913));
#20768=CARTESIAN_POINT('Ctrl Pts',(8.59489616871569,-80.4867511126201,4.96226561664425));
#20769=CARTESIAN_POINT('Ctrl Pts',(11.4598615582757,-80.3117511126201,-2.06354052510241E-11));
#20770=CARTESIAN_POINT('Ctrl Pts',(8.59489616869782,-80.1367511126201,-4.9622656166752));
#20771=CARTESIAN_POINT('Ctrl Pts',(5.72993077911996,-79.9617511126201,-9.92453123332976));
#20772=CARTESIAN_POINT('Ctrl Pts',(-1.78726082715848E-11,-79.7867511126201,
-9.92453123331945));
#20773=CARTESIAN_POINT('Ctrl Pts',(-5.7299307791557,-79.6117511126201,-9.92453123330913));
#20774=CARTESIAN_POINT('Ctrl Pts',(-8.59489616871569,-79.4367511126201,
-4.96226561664425));
#20775=CARTESIAN_POINT('Ctrl Pts',(-11.4598615582757,-79.2617511126201,
2.06368086793017E-11));
#20776=CARTESIAN_POINT('Ctrl Pts',(-8.59489616869782,-79.0867511126201,
4.9622656166752));
#20777=CARTESIAN_POINT('Ctrl Pts',(-5.72993077911996,-78.9117511126201,
9.92453123332977));
#20778=CARTESIAN_POINT('Ctrl Pts',(1.7871392867044E-11,-78.7367511126201,
9.92453123331945));
#20779=CARTESIAN_POINT('Ctrl Pts',(5.7299307791557,-78.5617511126201,9.92453123330913));
#20780=CARTESIAN_POINT('Ctrl Pts',(8.59489616871569,-78.3867511126201,4.96226561664425));
#20781=CARTESIAN_POINT('Ctrl Pts',(11.4598615582757,-78.2117511126201,-2.06354052510241E-11));
#20782=CARTESIAN_POINT('Ctrl Pts',(8.59489616869782,-78.0367511126201,-4.9622656166752));
#20783=CARTESIAN_POINT('Ctrl Pts',(5.72993077911996,-77.8617511126201,-9.92453123332976));
#20784=CARTESIAN_POINT('Ctrl Pts',(-1.78726082715848E-11,-77.6867511126201,
-9.92453123331945));
#20785=CARTESIAN_POINT('Ctrl Pts',(-5.7299307791557,-77.5117511126201,-9.92453123330913));
#20786=CARTESIAN_POINT('Ctrl Pts',(-8.59489616871569,-77.3367511126201,
-4.96226561664425));
#20787=CARTESIAN_POINT('Ctrl Pts',(-11.4598615582757,-77.1617511126201,
2.06368086793017E-11));
#20788=CARTESIAN_POINT('Ctrl Pts',(-8.59489616869782,-76.9867511126201,
4.9622656166752));
#20789=CARTESIAN_POINT('Ctrl Pts',(-5.72993077911996,-76.8117511126201,
9.92453123332977));
#20790=CARTESIAN_POINT('Ctrl Pts',(1.7871392867044E-11,-76.6367511126201,
9.92453123331945));
#20791=CARTESIAN_POINT('Ctrl Pts',(5.7299307791557,-76.4617511126201,9.92453123330913));
#20792=CARTESIAN_POINT('Ctrl Pts',(8.59489616871569,-76.2867511126201,4.96226561664425));
#20793=CARTESIAN_POINT('Ctrl Pts',(11.4598615582757,-76.1117511126201,-2.06354052510241E-11));
#20794=CARTESIAN_POINT('Ctrl Pts',(8.59489616869782,-75.9367511126201,-4.9622656166752));
#20795=CARTESIAN_POINT('Ctrl Pts',(5.72993077911996,-75.7617511126201,-9.92453123332976));
#20796=CARTESIAN_POINT('Ctrl Pts',(-1.78726082715848E-11,-75.5867511126201,
-9.92453123331945));
#20797=CARTESIAN_POINT('Ctrl Pts',(-5.7299307791557,-75.4117511126202,-9.92453123330913));
#20798=CARTESIAN_POINT('Ctrl Pts',(-8.59489616871569,-75.2367511126201,
-4.96226561664425));
#20799=CARTESIAN_POINT('Ctrl Pts',(-11.4598615582757,-75.0617511126201,
2.06368086793017E-11));
#20800=CARTESIAN_POINT('Ctrl Pts',(-8.59489616869782,-74.8867511126201,
4.9622656166752));
#20801=CARTESIAN_POINT('Ctrl Pts',(-5.72993077911996,-74.7117511126201,
9.92453123332977));
#20802=CARTESIAN_POINT('Ctrl Pts',(1.7871392867044E-11,-74.5367511126201,
9.92453123331945));
#20803=CARTESIAN_POINT('Ctrl Pts',(5.7299307791557,-74.3617511126201,9.92453123330913));
#20804=CARTESIAN_POINT('Ctrl Pts',(8.59489616871569,-74.1867511126201,4.96226561664425));
#20805=CARTESIAN_POINT('Ctrl Pts',(11.4598615582757,-74.0117511126201,-2.06354052510241E-11));
#20806=CARTESIAN_POINT('Ctrl Pts',(8.59489616869782,-73.8367511126201,-4.9622656166752));
#20807=CARTESIAN_POINT('Ctrl Pts',(5.72993077911996,-73.6617511126201,-9.92453123332976));
#20808=CARTESIAN_POINT('Ctrl Pts',(-1.78726082715848E-11,-73.4867511126201,
-9.92453123331945));
#20809=CARTESIAN_POINT('Ctrl Pts',(-5.7299307791557,-73.3117511126201,-9.92453123330913));
#20810=CARTESIAN_POINT('Ctrl Pts',(-8.59489616871569,-73.1367511126201,
-4.96226561664425));
#20811=CARTESIAN_POINT('Ctrl Pts',(-11.4598615582757,-72.9617511126201,
2.06368086793017E-11));
#20812=CARTESIAN_POINT('Ctrl Pts',(-8.59489616869782,-72.7867511126201,
4.9622656166752));
#20813=CARTESIAN_POINT('Ctrl Pts',(-5.72993077911996,-72.6117511126201,
9.92453123332977));
#20814=CARTESIAN_POINT('Ctrl Pts',(1.7871392867044E-11,-72.4367511126201,
9.92453123331945));
#20815=CARTESIAN_POINT('Ctrl Pts',(5.7299307791557,-72.2617511126201,9.92453123330913));
#20816=CARTESIAN_POINT('Ctrl Pts',(8.59489616871569,-72.0867511126201,4.96226561664425));
#20817=CARTESIAN_POINT('Ctrl Pts',(11.4598615582757,-71.9117511126201,-2.06354052510241E-11));
#20818=CARTESIAN_POINT('Ctrl Pts',(8.59489616869782,-71.7367511126201,-4.9622656166752));
#20819=CARTESIAN_POINT('Ctrl Pts',(5.72993077911996,-71.5617511126201,-9.92453123332976));
#20820=CARTESIAN_POINT('Ctrl Pts',(-1.78726082715848E-11,-71.3867511126201,
-9.92453123331945));
#20821=CARTESIAN_POINT('Ctrl Pts',(-5.7299307791557,-71.2117511126201,-9.92453123330913));
#20822=CARTESIAN_POINT('Ctrl Pts',(-8.59489616871569,-71.0367511126201,
-4.96226561664425));
#20823=CARTESIAN_POINT('Ctrl Pts',(-11.4598615582757,-70.8617511126201,
2.06368086793017E-11));
#20824=CARTESIAN_POINT('Ctrl Pts',(-8.59489616869782,-70.6867511126201,
4.9622656166752));
#20825=CARTESIAN_POINT('Ctrl Pts',(-5.72993077911996,-70.5117511126201,
9.92453123332977));
#20826=CARTESIAN_POINT('Ctrl Pts',(1.7871392867044E-11,-70.3367511126201,
9.92453123331945));
#20827=CARTESIAN_POINT('Ctrl Pts',(5.7299307791557,-70.1617511126201,9.92453123330913));
#20828=CARTESIAN_POINT('Ctrl Pts',(8.59489616871569,-69.9867511126201,4.96226561664425));
#20829=CARTESIAN_POINT('Ctrl Pts',(11.4598615582757,-69.8117511126202,-2.06354052510241E-11));
#20830=CARTESIAN_POINT('Ctrl Pts',(8.59489616869782,-69.6367511126201,-4.9622656166752));
#20831=CARTESIAN_POINT('Ctrl Pts',(5.72993077911996,-69.4617511126201,-9.92453123332976));
#20832=CARTESIAN_POINT('Ctrl Pts',(-1.78726082715848E-11,-69.2867511126201,
-9.92453123331945));
#20833=CARTESIAN_POINT('Ctrl Pts',(-5.7299307791557,-69.1117511126201,-9.92453123330913));
#20834=CARTESIAN_POINT('Ctrl Pts',(-8.59489616871569,-68.9367511126201,
-4.96226561664425));
#20835=CARTESIAN_POINT('Ctrl Pts',(-11.4598615582757,-68.7617511126201,
2.06368086793017E-11));
#20836=CARTESIAN_POINT('Ctrl Pts',(-8.59489616869782,-68.5867511126201,
4.9622656166752));
#20837=CARTESIAN_POINT('Ctrl Pts',(-5.72993077911996,-68.4117511126201,
9.92453123332977));
#20838=CARTESIAN_POINT('Ctrl Pts',(1.7871392867044E-11,-68.2367511126201,
9.92453123331945));
#20839=CARTESIAN_POINT('Ctrl Pts',(5.7299307791557,-68.0617511126201,9.92453123330913));
#20840=CARTESIAN_POINT('Ctrl Pts',(8.59489616871569,-67.8867511126201,4.96226561664425));
#20841=CARTESIAN_POINT('Ctrl Pts',(11.4598615582757,-67.7117511126201,-2.06354052510241E-11));
#20842=CARTESIAN_POINT('Ctrl Pts',(8.59489616869782,-67.5367511126201,-4.9622656166752));
#20843=CARTESIAN_POINT('Ctrl Pts',(5.72993077911996,-67.3617511126201,-9.92453123332976));
#20844=CARTESIAN_POINT('Ctrl Pts',(-1.78726082715848E-11,-67.1867511126202,
-9.92453123331945));
#20845=CARTESIAN_POINT('Ctrl Pts',(-5.7299307791557,-67.0117511126201,-9.92453123330913));
#20846=CARTESIAN_POINT('Ctrl Pts',(-8.59489616871569,-66.8367511126201,
-4.96226561664425));
#20847=CARTESIAN_POINT('Ctrl Pts',(-11.4598615582757,-66.6617511126202,
2.06368086793017E-11));
#20848=CARTESIAN_POINT('Ctrl Pts',(-8.59489616869782,-66.4867511126201,
4.9622656166752));
#20849=CARTESIAN_POINT('Ctrl Pts',(-5.72993077911996,-66.3117511126201,
9.92453123332977));
#20850=CARTESIAN_POINT('Ctrl Pts',(1.7871392867044E-11,-66.1367511126202,
9.92453123331945));
#20851=CARTESIAN_POINT('Ctrl Pts',(5.7299307791557,-65.9617511126201,9.92453123330913));
#20852=CARTESIAN_POINT('Ctrl Pts',(8.59489616871569,-65.7867511126201,4.96226561664425));
#20853=CARTESIAN_POINT('Ctrl Pts',(11.4598615582757,-65.6117511126202,-2.06354052510241E-11));
#20854=CARTESIAN_POINT('Ctrl Pts',(8.59489616869782,-65.4367511126201,-4.9622656166752));
#20855=CARTESIAN_POINT('Ctrl Pts',(5.72993077911996,-65.2617511126201,-9.92453123332976));
#20856=CARTESIAN_POINT('Ctrl Pts',(-1.78726082715848E-11,-65.0867511126201,
-9.92453123331945));
#20857=CARTESIAN_POINT('Ctrl Pts',(-5.7299307791557,-64.9117511126201,-9.92453123330913));
#20858=CARTESIAN_POINT('Ctrl Pts',(-8.59489616871569,-64.7367511126201,
-4.96226561664425));
#20859=CARTESIAN_POINT('Ctrl Pts',(-11.4598615582757,-64.5617511126202,
2.06368086793017E-11));
#20860=CARTESIAN_POINT('Ctrl Pts',(-8.59489616869782,-64.3867511126201,
4.9622656166752));
#20861=CARTESIAN_POINT('Ctrl Pts',(-5.72993077911996,-64.2117511126201,
9.92453123332977));
#20862=CARTESIAN_POINT('Ctrl Pts',(1.7871392867044E-11,-64.0367511126202,
9.92453123331945));
#20863=CARTESIAN_POINT('Ctrl Pts',(5.7299307791557,-63.8617511126201,9.92453123330913));
#20864=CARTESIAN_POINT('Ctrl Pts',(8.59489616871569,-63.6867511126202,4.96226561664425));
#20865=CARTESIAN_POINT('Ctrl Pts',(11.4598615582757,-63.5117511126202,-2.06354052510241E-11));
#20866=CARTESIAN_POINT('Ctrl Pts',(8.59489616869782,-63.3367511126201,-4.9622656166752));
#20867=CARTESIAN_POINT('Ctrl Pts',(5.72993077911996,-63.1617511126202,-9.92453123332976));
#20868=CARTESIAN_POINT('Ctrl Pts',(-1.78726082715848E-11,-62.9867511126201,
-9.92453123331945));
#20869=CARTESIAN_POINT('Ctrl Pts',(-5.7299307791557,-62.8117511126201,-9.92453123330913));
#20870=CARTESIAN_POINT('Ctrl Pts',(-8.59489616871569,-62.6367511126202,
-4.96226561664425));
#20871=CARTESIAN_POINT('Ctrl Pts',(-11.4598615582757,-62.4617511126202,
2.06368086793017E-11));
#20872=CARTESIAN_POINT('Ctrl Pts',(-8.59489616869782,-62.2867511126201,
4.9622656166752));
#20873=CARTESIAN_POINT('Ctrl Pts',(-5.72993077911996,-62.1117511126202,
9.92453123332977));
#20874=CARTESIAN_POINT('Ctrl Pts',(1.7871392867044E-11,-61.9367511126202,
9.92453123331945));
#20875=CARTESIAN_POINT('Ctrl Pts',(5.7299307791557,-61.7617511126201,9.92453123330913));
#20876=CARTESIAN_POINT('Ctrl Pts',(8.59489616871569,-61.5867511126202,4.96226561664425));
#20877=CARTESIAN_POINT('Ctrl Pts',(11.4598615582757,-61.4117511126202,-2.06354052510241E-11));
#20878=CARTESIAN_POINT('Ctrl Pts',(8.59489616869782,-61.2367511126201,-4.9622656166752));
#20879=CARTESIAN_POINT('Ctrl Pts',(5.72993077911996,-61.0617511126202,-9.92453123332976));
#20880=CARTESIAN_POINT('Ctrl Pts',(-1.78726082715848E-11,-60.8867511126202,
-9.92453123331945));
#20881=CARTESIAN_POINT('Ctrl Pts',(-5.7299307791557,-60.7117511126201,-9.92453123330913));
#20882=CARTESIAN_POINT('Ctrl Pts',(-8.59489616871569,-60.5367511126202,
-4.96226561664425));
#20883=CARTESIAN_POINT('Ctrl Pts',(-11.4598615582757,-60.3617511126202,
2.06368086793017E-11));
#20884=CARTESIAN_POINT('Ctrl Pts',(-8.59489616869782,-60.1867511126201,
4.9622656166752));
#20885=CARTESIAN_POINT('Ctrl Pts',(-5.72993077911996,-60.0117511126202,
9.92453123332977));
#20886=CARTESIAN_POINT('Ctrl Pts',(1.7871392867044E-11,-59.8367511126202,
9.92453123331945));
#20887=CARTESIAN_POINT('Ctrl Pts',(5.7299307791557,-59.6617511126202,9.92453123330913));
#20888=CARTESIAN_POINT('Ctrl Pts',(8.59489616871569,-59.4867511126202,4.96226561664425));
#20889=CARTESIAN_POINT('Ctrl Pts',(11.4598615582757,-59.3117511126202,-2.06354052510241E-11));
#20890=CARTESIAN_POINT('Ctrl Pts',(8.59489616869782,-59.1367511126202,-4.9622656166752));
#20891=CARTESIAN_POINT('Ctrl Pts',(5.72993077911996,-58.9617511126202,-9.92453123332976));
#20892=CARTESIAN_POINT('Ctrl Pts',(-1.78726082715848E-11,-58.7867511126202,
-9.92453123331945));
#20893=CARTESIAN_POINT('Ctrl Pts',(-5.7299307791557,-58.6117511126201,-9.92453123330913));
#20894=CARTESIAN_POINT('Ctrl Pts',(-8.59489616871569,-58.4367511126202,
-4.96226561664425));
#20895=CARTESIAN_POINT('Ctrl Pts',(-11.4598615582757,-58.2617511126201,
2.06368086793017E-11));
#20896=CARTESIAN_POINT('Ctrl Pts',(-8.59489616869782,-58.0867511126202,
4.9622656166752));
#20897=CARTESIAN_POINT('Ctrl Pts',(-5.72993077911996,-57.9117511126202,
9.92453123332977));
#20898=CARTESIAN_POINT('Ctrl Pts',(1.7871392867044E-11,-57.7367511126201,
9.92453123331945));
#20899=CARTESIAN_POINT('Ctrl Pts',(5.7299307791557,-57.5617511126202,9.92453123330913));
#20900=CARTESIAN_POINT('Ctrl Pts',(8.59489616871569,-57.3867511126202,4.96226561664425));
#20901=CARTESIAN_POINT('Ctrl Pts',(11.4598615582757,-57.2117511126201,-2.06354052510241E-11));
#20902=CARTESIAN_POINT('Ctrl Pts',(8.59489616869782,-57.0367511126202,-4.9622656166752));
#20903=CARTESIAN_POINT('Ctrl Pts',(5.72993077911996,-56.8617511126202,-9.92453123332976));
#20904=CARTESIAN_POINT('Ctrl Pts',(-1.78726082715848E-11,-56.6867511126202,
-9.92453123331945));
#20905=CARTESIAN_POINT('Ctrl Pts',(-5.7299307791557,-56.5117511126202,-9.92453123330913));
#20906=CARTESIAN_POINT('Ctrl Pts',(-8.59489616871569,-56.3367511126202,
-4.96226561664425));
#20907=CARTESIAN_POINT('Ctrl Pts',(-11.4598615582757,-56.1617511126202,
2.06368086793017E-11));
#20908=CARTESIAN_POINT('Ctrl Pts',(-8.59489616869782,-55.9867511126202,
4.9622656166752));
#20909=CARTESIAN_POINT('Ctrl Pts',(-5.72993077911996,-55.8117511126202,
9.92453123332977));
#20910=CARTESIAN_POINT('Ctrl Pts',(1.7871392867044E-11,-55.6367511126201,
9.92453123331945));
#20911=CARTESIAN_POINT('Ctrl Pts',(5.7299307791557,-55.4617511126202,9.92453123330913));
#20912=CARTESIAN_POINT('Ctrl Pts',(8.59489616871569,-55.2867511126202,4.96226561664425));
#20913=CARTESIAN_POINT('Ctrl Pts',(11.4598615582757,-55.1117511126202,-2.06354052510241E-11));
#20914=CARTESIAN_POINT('Ctrl Pts',(8.59489616869782,-54.9367511126202,-4.9622656166752));
#20915=CARTESIAN_POINT('Ctrl Pts',(5.72993077911996,-54.7617511126202,-9.92453123332976));
#20916=CARTESIAN_POINT('Ctrl Pts',(-1.78726082715848E-11,-54.5867511126202,
-9.92453123331945));
#20917=CARTESIAN_POINT('Ctrl Pts',(-5.7299307791557,-54.4117511126202,-9.92453123330913));
#20918=CARTESIAN_POINT('Ctrl Pts',(-8.59489616871569,-54.2367511126202,
-4.96226561664425));
#20919=CARTESIAN_POINT('Ctrl Pts',(-11.4598615582757,-54.0617511126202,
2.06368086793017E-11));
#20920=CARTESIAN_POINT('Ctrl Pts',(-8.59489616869782,-53.8867511126202,
4.9622656166752));
#20921=CARTESIAN_POINT('Ctrl Pts',(-5.72993077911996,-53.7117511126202,
9.92453123332977));
#20922=CARTESIAN_POINT('Ctrl Pts',(1.7871392867044E-11,-53.5367511126202,
9.92453123331945));
#20923=CARTESIAN_POINT('Ctrl Pts',(5.7299307791557,-53.3617511126202,9.92453123330913));
#20924=CARTESIAN_POINT('Ctrl Pts',(8.59489616871569,-53.1867511126202,4.96226561664425));
#20925=CARTESIAN_POINT('Ctrl Pts',(11.4598615582757,-53.0117511126202,-2.06354052510241E-11));
#20926=CARTESIAN_POINT('Ctrl Pts',(8.59489616869782,-52.8367511126202,-4.9622656166752));
#20927=CARTESIAN_POINT('Ctrl Pts',(5.72993077911996,-52.6617511126202,-9.92453123332976));
#20928=CARTESIAN_POINT('Ctrl Pts',(-1.78726082715848E-11,-52.4867511126202,
-9.92453123331945));
#20929=CARTESIAN_POINT('Ctrl Pts',(-5.7299307791557,-52.3117511126202,-9.92453123330913));
#20930=CARTESIAN_POINT('Ctrl Pts',(-8.59489616871569,-52.1367511126202,
-4.96226561664425));
#20931=CARTESIAN_POINT('Ctrl Pts',(-11.4598615582757,-51.9617511126202,
2.06368086793017E-11));
#20932=CARTESIAN_POINT('Ctrl Pts',(-8.59489616869782,-51.7867511126202,
4.9622656166752));
#20933=CARTESIAN_POINT('Ctrl Pts',(-5.72993077911996,-51.6117511126202,
9.92453123332977));
#20934=CARTESIAN_POINT('Ctrl Pts',(1.7871392867044E-11,-51.4367511126202,
9.92453123331945));
#20935=CARTESIAN_POINT('Ctrl Pts',(5.7299307791557,-51.2617511126202,9.92453123330913));
#20936=CARTESIAN_POINT('Ctrl Pts',(8.59489616871569,-51.0867511126202,4.96226561664425));
#20937=CARTESIAN_POINT('Ctrl Pts',(11.4598615582757,-50.9117511126202,-2.06354052510241E-11));
#20938=CARTESIAN_POINT('Ctrl Pts',(8.59489616869782,-50.7367511126202,-4.9622656166752));
#20939=CARTESIAN_POINT('Ctrl Pts',(5.72993077911996,-50.5617511126202,-9.92453123332976));
#20940=CARTESIAN_POINT('Ctrl Pts',(-1.78726082715848E-11,-50.3867511126202,
-9.92453123331945));
#20941=CARTESIAN_POINT('Ctrl Pts',(-5.7299307791557,-50.2117511126202,-9.92453123330913));
#20942=CARTESIAN_POINT('Ctrl Pts',(-8.59489616871569,-50.0367511126202,
-4.96226561664425));
#20943=CARTESIAN_POINT('Ctrl Pts',(-11.4598615582757,-49.8617511126202,
2.06368086793017E-11));
#20944=CARTESIAN_POINT('Ctrl Pts',(-8.59489616869782,-49.6867511126202,
4.9622656166752));
#20945=CARTESIAN_POINT('Ctrl Pts',(-5.72993077911996,-49.5117511126202,
9.92453123332977));
#20946=CARTESIAN_POINT('Ctrl Pts',(1.7871392867044E-11,-49.3367511126202,
9.92453123331945));
#20947=CARTESIAN_POINT('Ctrl Pts',(5.7299307791557,-49.1617511126202,9.92453123330913));
#20948=CARTESIAN_POINT('Ctrl Pts',(8.59489616871569,-48.9867511126202,4.96226561664425));
#20949=CARTESIAN_POINT('Ctrl Pts',(11.4598615582757,-48.8117511126202,-2.06354052510241E-11));
#20950=CARTESIAN_POINT('Ctrl Pts',(8.59489616869782,-48.6367511126202,-4.9622656166752));
#20951=CARTESIAN_POINT('Ctrl Pts',(5.72993077911996,-48.4617511126202,-9.92453123332976));
#20952=CARTESIAN_POINT('Ctrl Pts',(-1.78726082715848E-11,-48.2867511126202,
-9.92453123331945));
#20953=CARTESIAN_POINT('Ctrl Pts',(-5.7299307791557,-48.1117511126202,-9.92453123330913));
#20954=CARTESIAN_POINT('Ctrl Pts',(-8.59489616871569,-47.9367511126202,
-4.96226561664425));
#20955=CARTESIAN_POINT('Ctrl Pts',(-11.4598615582757,-47.7617511126202,
2.06368086793017E-11));
#20956=CARTESIAN_POINT('Ctrl Pts',(-8.59489616869782,-47.5867511126202,
4.9622656166752));
#20957=CARTESIAN_POINT('Ctrl Pts',(-5.72993077911996,-47.4117511126202,
9.92453123332977));
#20958=CARTESIAN_POINT('Ctrl Pts',(1.7871392867044E-11,-47.2367511126202,
9.92453123331945));
#20959=CARTESIAN_POINT('Ctrl Pts',(5.7299307791557,-47.0617511126202,9.92453123330913));
#20960=CARTESIAN_POINT('Ctrl Pts',(8.59489616871569,-46.8867511126202,4.96226561664425));
#20961=CARTESIAN_POINT('Ctrl Pts',(11.4598615582757,-46.7117511126202,-2.06354052510241E-11));
#20962=CARTESIAN_POINT('Ctrl Pts',(8.59489616869782,-46.5367511126202,-4.9622656166752));
#20963=CARTESIAN_POINT('Ctrl Pts',(5.72993077911996,-46.3617511126202,-9.92453123332976));
#20964=CARTESIAN_POINT('Ctrl Pts',(-1.78726082715848E-11,-46.1867511126202,
-9.92453123331945));
#20965=CARTESIAN_POINT('Ctrl Pts',(-5.7299307791557,-46.0117511126202,-9.92453123330913));
#20966=CARTESIAN_POINT('Ctrl Pts',(-8.59489616871569,-45.8367511126202,
-4.96226561664425));
#20967=CARTESIAN_POINT('Ctrl Pts',(-11.4598615582757,-45.6617511126202,
2.06368086793017E-11));
#20968=CARTESIAN_POINT('Ctrl Pts',(-8.59489616869782,-45.4867511126202,
4.9622656166752));
#20969=CARTESIAN_POINT('Ctrl Pts',(-5.72993077911996,-45.3117511126202,
9.92453123332977));
#20970=CARTESIAN_POINT('Ctrl Pts',(1.7871392867044E-11,-45.1367511126202,
9.92453123331945));
#20971=CARTESIAN_POINT('Ctrl Pts',(5.7299307791557,-44.9617511126202,9.92453123330913));
#20972=CARTESIAN_POINT('Ctrl Pts',(8.59489616871569,-44.7867511126202,4.96226561664425));
#20973=CARTESIAN_POINT('Ctrl Pts',(11.4598615582757,-44.6117511126202,-2.06354052510241E-11));
#20974=CARTESIAN_POINT('Ctrl Pts',(8.59489616869782,-44.4367511126202,-4.9622656166752));
#20975=CARTESIAN_POINT('Ctrl Pts',(5.72993077911996,-44.2617511126202,-9.92453123332976));
#20976=CARTESIAN_POINT('Ctrl Pts',(-1.78726082715848E-11,-44.0867511126202,
-9.92453123331945));
#20977=CARTESIAN_POINT('Ctrl Pts',(-5.7299307791557,-43.9117511126202,-9.92453123330913));
#20978=CARTESIAN_POINT('Ctrl Pts',(-8.59489616871569,-43.7367511126202,
-4.96226561664425));
#20979=CARTESIAN_POINT('Ctrl Pts',(-11.4598615582757,-43.5617511126202,
2.06368086793017E-11));
#20980=CARTESIAN_POINT('Ctrl Pts',(-8.59489616869782,-43.3867511126202,
4.9622656166752));
#20981=CARTESIAN_POINT('Ctrl Pts',(-5.72993077911996,-43.2117511126202,
9.92453123332977));
#20982=CARTESIAN_POINT('Ctrl Pts',(1.7871392867044E-11,-43.0367511126202,
9.92453123331945));
#20983=CARTESIAN_POINT('Ctrl Pts',(5.7299307791557,-42.8617511126202,9.92453123330913));
#20984=CARTESIAN_POINT('Ctrl Pts',(8.59489616871569,-42.6867511126202,4.96226561664425));
#20985=CARTESIAN_POINT('Ctrl Pts',(11.4598615582757,-42.5117511126202,-2.06354052510241E-11));
#20986=CARTESIAN_POINT('Ctrl Pts',(8.59489616869782,-42.3367511126202,-4.9622656166752));
#20987=CARTESIAN_POINT('Ctrl Pts',(5.72993077911996,-42.1617511126202,-9.92453123332976));
#20988=CARTESIAN_POINT('Ctrl Pts',(-1.78726082715848E-11,-41.9867511126202,
-9.92453123331945));
#20989=CARTESIAN_POINT('Ctrl Pts',(-5.7299307791557,-41.8117511126202,-9.92453123330913));
#20990=CARTESIAN_POINT('Ctrl Pts',(-8.59489616871569,-41.6367511126202,
-4.96226561664425));
#20991=CARTESIAN_POINT('Ctrl Pts',(-11.4598615582757,-41.4617511126202,
2.06368086793017E-11));
#20992=CARTESIAN_POINT('Ctrl Pts',(-8.59489616869782,-41.2867511126202,
4.9622656166752));
#20993=CARTESIAN_POINT('Ctrl Pts',(-5.72993077911996,-41.1117511126202,
9.92453123332977));
#20994=CARTESIAN_POINT('Ctrl Pts',(1.7871392867044E-11,-40.9367511126202,
9.92453123331945));
#20995=CARTESIAN_POINT('Ctrl Pts',(5.7299307791557,-40.7617511126202,9.92453123330913));
#20996=CARTESIAN_POINT('Ctrl Pts',(8.59489616871569,-40.5867511126202,4.96226561664425));
#20997=CARTESIAN_POINT('Ctrl Pts',(11.4598615582757,-40.4117511126202,-2.06354052510241E-11));
#20998=CARTESIAN_POINT('Ctrl Pts',(8.59489616869782,-40.2367511126202,-4.9622656166752));
#20999=CARTESIAN_POINT('Ctrl Pts',(5.72993077911996,-40.0617511126202,-9.92453123332976));
#21000=CARTESIAN_POINT('Ctrl Pts',(-1.78726082715848E-11,-39.8867511126202,
-9.92453123331945));
#21001=CARTESIAN_POINT('Ctrl Pts',(-5.7299307791557,-39.7117511126202,-9.92453123330913));
#21002=CARTESIAN_POINT('Ctrl Pts',(-8.59489616871569,-39.5367511126202,
-4.96226561664425));
#21003=CARTESIAN_POINT('Ctrl Pts',(-11.4598615582757,-39.3617511126202,
2.06368086793017E-11));
#21004=CARTESIAN_POINT('Ctrl Pts',(-8.59489616869782,-39.1867511126202,
4.9622656166752));
#21005=CARTESIAN_POINT('Ctrl Pts',(-5.72993077911996,-39.0117511126202,
9.92453123332977));
#21006=CARTESIAN_POINT('Ctrl Pts',(1.7871392867044E-11,-38.8367511126202,
9.92453123331945));
#21007=CARTESIAN_POINT('Ctrl Pts',(5.7299307791557,-38.6617511126202,9.92453123330913));
#21008=CARTESIAN_POINT('Ctrl Pts',(8.59489616871569,-38.4867511126202,4.96226561664425));
#21009=CARTESIAN_POINT('Ctrl Pts',(11.4598615582757,-38.3117511126202,-2.06354052510241E-11));
#21010=CARTESIAN_POINT('Ctrl Pts',(8.59489616869782,-38.1367511126202,-4.9622656166752));
#21011=CARTESIAN_POINT('Ctrl Pts',(5.72993077911996,-37.9617511126202,-9.92453123332976));
#21012=CARTESIAN_POINT('Ctrl Pts',(-1.78726082715848E-11,-37.7867511126202,
-9.92453123331945));
#21013=CARTESIAN_POINT('Ctrl Pts',(-5.7299307791557,-37.6117511126202,-9.92453123330913));
#21014=CARTESIAN_POINT('Ctrl Pts',(-8.59489616871569,-37.4367511126202,
-4.96226561664425));
#21015=CARTESIAN_POINT('Ctrl Pts',(-11.4598615582757,-37.2617511126202,
2.06368086793017E-11));
#21016=CARTESIAN_POINT('Ctrl Pts',(-8.59489616869782,-37.0867511126202,
4.9622656166752));
#21017=CARTESIAN_POINT('Ctrl Pts',(-5.72993077911996,-36.9117511126202,
9.92453123332977));
#21018=CARTESIAN_POINT('Ctrl Pts',(1.7871392867044E-11,-36.7367511126202,
9.92453123331945));
#21019=CARTESIAN_POINT('Ctrl Pts',(5.7299307791557,-36.5617511126202,9.92453123330913));
#21020=CARTESIAN_POINT('Ctrl Pts',(8.59489616871569,-36.3867511126202,4.96226561664425));
#21021=CARTESIAN_POINT('Ctrl Pts',(11.4598615582757,-36.2117511126202,-2.06354052510241E-11));
#21022=CARTESIAN_POINT('Ctrl Pts',(8.59489616869782,-36.0367511126202,-4.9622656166752));
#21023=CARTESIAN_POINT('Ctrl Pts',(5.72993077911996,-35.8617511126202,-9.92453123332976));
#21024=CARTESIAN_POINT('Ctrl Pts',(-1.78726082715848E-11,-35.6867511126202,
-9.92453123331945));
#21025=CARTESIAN_POINT('Ctrl Pts',(-5.7299307791557,-35.5117511126202,-9.92453123330913));
#21026=CARTESIAN_POINT('Ctrl Pts',(-8.59489616871569,-35.3367511126202,
-4.96226561664425));
#21027=CARTESIAN_POINT('Ctrl Pts',(-11.4598615582757,-35.1617511126202,
2.06368086793017E-11));
#21028=CARTESIAN_POINT('Ctrl Pts',(-8.59489616869782,-34.9867511126202,
4.9622656166752));
#21029=CARTESIAN_POINT('Ctrl Pts',(-5.72993077911996,-34.8117511126202,
9.92453123332977));
#21030=CARTESIAN_POINT('Ctrl Pts',(1.7871392867044E-11,-34.6367511126202,
9.92453123331945));
#21031=CARTESIAN_POINT('Ctrl Pts',(5.7299307791557,-34.4617511126202,9.92453123330913));
#21032=CARTESIAN_POINT('Ctrl Pts',(8.59489616871569,-34.2867511126202,4.96226561664425));
#21033=CARTESIAN_POINT('Ctrl Pts',(11.4598615582757,-34.1117511126202,-2.06354052510241E-11));
#21034=CARTESIAN_POINT('Ctrl Pts',(8.59489616869782,-33.9367511126202,-4.9622656166752));
#21035=CARTESIAN_POINT('Ctrl Pts',(5.72993077911996,-33.7617511126202,-9.92453123332976));
#21036=CARTESIAN_POINT('Ctrl Pts',(-1.78726082715848E-11,-33.5867511126202,
-9.92453123331945));
#21037=CARTESIAN_POINT('Ctrl Pts',(-5.7299307791557,-33.4117511126202,-9.92453123330913));
#21038=CARTESIAN_POINT('Ctrl Pts',(-8.59489616871569,-33.2367511126202,
-4.96226561664425));
#21039=CARTESIAN_POINT('Ctrl Pts',(-11.4598615582757,-33.0617511126202,
2.06368086793017E-11));
#21040=CARTESIAN_POINT('Ctrl Pts',(-8.59489616869782,-32.8867511126202,
4.9622656166752));
#21041=CARTESIAN_POINT('Ctrl Pts',(-5.72993077911996,-32.7117511126202,
9.92453123332977));
#21042=CARTESIAN_POINT('Ctrl Pts',(1.7871392867044E-11,-32.5367511126202,
9.92453123331945));
#21043=CARTESIAN_POINT('Ctrl Pts',(5.7299307791557,-32.3617511126202,9.92453123330913));
#21044=CARTESIAN_POINT('Ctrl Pts',(8.59489616871569,-32.1867511126202,4.96226561664425));
#21045=CARTESIAN_POINT('Ctrl Pts',(11.4598615582757,-32.0117511126202,-2.06354052510241E-11));
#21046=CARTESIAN_POINT('Ctrl Pts',(8.59489616869782,-31.8367511126202,-4.9622656166752));
#21047=CARTESIAN_POINT('Ctrl Pts',(5.72993077911996,-31.6617511126202,-9.92453123332976));
#21048=CARTESIAN_POINT('Ctrl Pts',(-1.78726082715848E-11,-31.4867511126202,
-9.92453123331945));
#21049=CARTESIAN_POINT('Ctrl Pts',(-5.7299307791557,-31.3117511126202,-9.92453123330913));
#21050=CARTESIAN_POINT('Ctrl Pts',(-8.59489616871569,-31.1367511126202,
-4.96226561664425));
#21051=CARTESIAN_POINT('Ctrl Pts',(-11.4598615582757,-30.9617511126202,
2.06368086793017E-11));
#21052=CARTESIAN_POINT('Ctrl Pts',(-8.59489616869782,-30.7867511126202,
4.9622656166752));
#21053=CARTESIAN_POINT('Ctrl Pts',(-5.72993077911996,-30.6117511126202,
9.92453123332977));
#21054=CARTESIAN_POINT('Ctrl Pts',(1.7871392867044E-11,-30.4367511126202,
9.92453123331945));
#21055=CARTESIAN_POINT('Ctrl Pts',(5.7299307791557,-30.2617511126202,9.92453123330913));
#21056=CARTESIAN_POINT('Ctrl Pts',(8.59489616871569,-30.0867511126202,4.96226561664425));
#21057=CARTESIAN_POINT('Ctrl Pts',(11.4598615582757,-29.9117511126202,-2.06354052510241E-11));
#21058=CARTESIAN_POINT('Ctrl Pts',(8.59489616869782,-29.7367511126202,-4.9622656166752));
#21059=CARTESIAN_POINT('Ctrl Pts',(5.72993077911996,-29.5617511126202,-9.92453123332976));
#21060=CARTESIAN_POINT('Ctrl Pts',(-1.78726082715848E-11,-29.3867511126202,
-9.92453123331945));
#21061=CARTESIAN_POINT('Ctrl Pts',(-5.7299307791557,-29.2117511126202,-9.92453123330913));
#21062=CARTESIAN_POINT('Ctrl Pts',(-8.59489616871569,-29.0367511126202,
-4.96226561664425));
#21063=CARTESIAN_POINT('Ctrl Pts',(-11.4598615582757,-28.8617511126202,
2.06368086793017E-11));
#21064=CARTESIAN_POINT('Ctrl Pts',(-8.59489616869782,-28.6867511126202,
4.9622656166752));
#21065=CARTESIAN_POINT('Ctrl Pts',(-5.72993077911996,-28.5117511126202,
9.92453123332977));
#21066=CARTESIAN_POINT('Ctrl Pts',(1.7871392867044E-11,-28.3367511126202,
9.92453123331945));
#21067=CARTESIAN_POINT('Ctrl Pts',(5.7299307791557,-28.1617511126202,9.92453123330913));
#21068=CARTESIAN_POINT('Ctrl Pts',(8.59489616871569,-27.9867511126202,4.96226561664425));
#21069=CARTESIAN_POINT('Ctrl Pts',(11.4598615582757,-27.8117511126202,-2.06354052510241E-11));
#21070=CARTESIAN_POINT('Ctrl Pts',(8.59489616869782,-27.6367511126202,-4.9622656166752));
#21071=CARTESIAN_POINT('Ctrl Pts',(5.72993077911996,-27.4617511126202,-9.92453123332976));
#21072=CARTESIAN_POINT('Ctrl Pts',(-1.78726082715848E-11,-27.2867511126202,
-9.92453123331945));
#21073=CARTESIAN_POINT('Ctrl Pts',(-5.7299307791557,-27.1117511126202,-9.92453123330913));
#21074=CARTESIAN_POINT('Ctrl Pts',(-8.59489616871569,-26.9367511126202,
-4.96226561664425));
#21075=CARTESIAN_POINT('Ctrl Pts',(-11.4598615582757,-26.7617511126202,
2.06368086793017E-11));
#21076=CARTESIAN_POINT('Ctrl Pts',(-8.59489616869782,-26.5867511126202,
4.9622656166752));
#21077=CARTESIAN_POINT('Ctrl Pts',(-5.72993077911996,-26.4117511126202,
9.92453123332977));
#21078=CARTESIAN_POINT('Ctrl Pts',(1.7871392867044E-11,-26.2367511126202,
9.92453123331945));
#21079=CARTESIAN_POINT('Ctrl Pts',(5.7299307791557,-26.0617511126202,9.92453123330913));
#21080=CARTESIAN_POINT('Ctrl Pts',(8.59489616871569,-25.8867511126202,4.96226561664425));
#21081=CARTESIAN_POINT('Ctrl Pts',(11.4598615582757,-25.7117511126202,-2.06354052510241E-11));
#21082=CARTESIAN_POINT('Ctrl Pts',(8.59489616869782,-25.5367511126202,-4.9622656166752));
#21083=CARTESIAN_POINT('Ctrl Pts',(5.72993077911996,-25.3617511126202,-9.92453123332976));
#21084=CARTESIAN_POINT('Ctrl Pts',(-1.78726082715848E-11,-25.1867511126202,
-9.92453123331945));
#21085=CARTESIAN_POINT('Ctrl Pts',(-5.7299307791557,-25.0117511126202,-9.92453123330913));
#21086=CARTESIAN_POINT('Ctrl Pts',(-8.59489616871569,-24.8367511126202,
-4.96226561664425));
#21087=CARTESIAN_POINT('Ctrl Pts',(-11.4598615582757,-24.6617511126202,
2.06368086793017E-11));
#21088=CARTESIAN_POINT('Ctrl Pts',(-8.59489616869782,-24.4867511126202,
4.9622656166752));
#21089=CARTESIAN_POINT('Ctrl Pts',(-5.72993077911996,-24.3117511126202,
9.92453123332977));
#21090=CARTESIAN_POINT('Ctrl Pts',(1.7871392867044E-11,-24.1367511126202,
9.92453123331945));
#21091=CARTESIAN_POINT('Ctrl Pts',(5.7299307791557,-23.9617511126202,9.92453123330913));
#21092=CARTESIAN_POINT('Ctrl Pts',(8.59489616871569,-23.7867511126202,4.96226561664425));
#21093=CARTESIAN_POINT('Ctrl Pts',(11.4598615582757,-23.6117511126202,-2.06354052510241E-11));
#21094=CARTESIAN_POINT('Ctrl Pts',(8.59489616869782,-23.4367511126202,-4.9622656166752));
#21095=CARTESIAN_POINT('Ctrl Pts',(5.72993077911996,-23.2617511126202,-9.92453123332976));
#21096=CARTESIAN_POINT('Ctrl Pts',(-1.78726082715848E-11,-23.0867511126202,
-9.92453123331945));
#21097=CARTESIAN_POINT('Ctrl Pts',(-5.7299307791557,-22.9117511126202,-9.92453123330913));
#21098=CARTESIAN_POINT('Ctrl Pts',(-8.59489616871569,-22.7367511126202,
-4.96226561664425));
#21099=CARTESIAN_POINT('Ctrl Pts',(-11.4598615582757,-22.5617511126203,
2.06368086793017E-11));
#21100=CARTESIAN_POINT('Ctrl Pts',(-8.59489616869782,-22.3867511126202,
4.9622656166752));
#21101=CARTESIAN_POINT('Ctrl Pts',(-5.72993077911996,-22.2117511126202,
9.92453123332977));
#21102=CARTESIAN_POINT('Ctrl Pts',(1.7871392867044E-11,-22.0367511126202,
9.92453123331945));
#21103=CARTESIAN_POINT('Ctrl Pts',(5.7299307791557,-21.8617511126203,9.92453123330913));
#21104=CARTESIAN_POINT('Ctrl Pts',(8.59489616871569,-21.6867511126202,4.96226561664425));
#21105=CARTESIAN_POINT('Ctrl Pts',(11.4598615582757,-21.5117511126203,-2.06354052510241E-11));
#21106=CARTESIAN_POINT('Ctrl Pts',(8.59489616869782,-21.3367511126203,-4.9622656166752));
#21107=CARTESIAN_POINT('Ctrl Pts',(5.72993077911996,-21.1617511126202,-9.92453123332976));
#21108=CARTESIAN_POINT('Ctrl Pts',(-1.78726082715848E-11,-20.9867511126202,
-9.92453123331945));
#21109=CARTESIAN_POINT('Ctrl Pts',(-5.7299307791557,-20.8117511126203,-9.92453123330913));
#21110=CARTESIAN_POINT('Ctrl Pts',(-8.59489616871569,-20.6367511126202,
-4.96226561664425));
#21111=CARTESIAN_POINT('Ctrl Pts',(-11.4598615582757,-20.4617511126203,
2.06368086793017E-11));
#21112=CARTESIAN_POINT('Ctrl Pts',(-8.59489616869782,-20.2867511126202,
4.9622656166752));
#21113=CARTESIAN_POINT('Ctrl Pts',(-5.72993077911996,-20.1117511126202,
9.92453123332977));
#21114=CARTESIAN_POINT('Ctrl Pts',(1.7871392867044E-11,-19.9367511126203,
9.92453123331945));
#21115=CARTESIAN_POINT('Ctrl Pts',(5.7299307791557,-19.7617511126202,9.92453123330913));
#21116=CARTESIAN_POINT('Ctrl Pts',(8.59489616871569,-19.5867511126202,4.96226561664425));
#21117=CARTESIAN_POINT('Ctrl Pts',(11.4598615582757,-19.4117511126203,-2.06354052510241E-11));
#21118=CARTESIAN_POINT('Ctrl Pts',(8.59489616869782,-19.2367511126202,-4.9622656166752));
#21119=CARTESIAN_POINT('Ctrl Pts',(5.72993077911996,-19.0617511126203,-9.92453123332976));
#21120=CARTESIAN_POINT('Ctrl Pts',(-1.78726082715848E-11,-18.8867511126203,
-9.92453123331945));
#21121=CARTESIAN_POINT('Ctrl Pts',(-5.7299307791557,-18.7117511126203,-9.92453123330913));
#21122=CARTESIAN_POINT('Ctrl Pts',(-8.59489616871569,-18.5367511126203,
-4.96226561664425));
#21123=CARTESIAN_POINT('Ctrl Pts',(-11.4598615582757,-18.3617511126203,
2.06368086793017E-11));
#21124=CARTESIAN_POINT('Ctrl Pts',(-8.59489616869782,-18.1867511126202,
4.9622656166752));
#21125=CARTESIAN_POINT('Ctrl Pts',(-5.72993077911996,-18.0117511126203,
9.92453123332977));
#21126=CARTESIAN_POINT('Ctrl Pts',(1.7871392867044E-11,-17.8367511126202,
9.92453123331945));
#21127=CARTESIAN_POINT('Ctrl Pts',(5.7299307791557,-17.6617511126203,9.92453123330913));
#21128=CARTESIAN_POINT('Ctrl Pts',(8.59489616871569,-17.4867511126202,4.96226561664425));
#21129=CARTESIAN_POINT('Ctrl Pts',(11.4598615582757,-17.3117511126203,-2.06354052510241E-11));
#21130=CARTESIAN_POINT('Ctrl Pts',(8.59489616869782,-17.1367511126203,-4.9622656166752));
#21131=CARTESIAN_POINT('Ctrl Pts',(5.72993077911996,-16.9617511126202,-9.92453123332976));
#21132=CARTESIAN_POINT('Ctrl Pts',(-1.78726082715848E-11,-16.7867511126203,
-9.92453123331945));
#21133=CARTESIAN_POINT('Ctrl Pts',(-5.7299307791557,-16.6117511126203,-9.92453123330913));
#21134=CARTESIAN_POINT('Ctrl Pts',(-8.59489616871569,-16.4367511126202,
-4.96226561664425));
#21135=CARTESIAN_POINT('Ctrl Pts',(-11.4598615582757,-16.2617511126203,
2.06368086793017E-11));
#21136=CARTESIAN_POINT('Ctrl Pts',(-8.59489616869782,-16.0867511126203,
4.9622656166752));
#21137=CARTESIAN_POINT('Ctrl Pts',(-5.72993077911996,-15.9117511126202,
9.92453123332977));
#21138=CARTESIAN_POINT('Ctrl Pts',(1.7871392867044E-11,-15.7367511126203,
9.92453123331945));
#21139=CARTESIAN_POINT('Ctrl Pts',(5.7299307791557,-15.5617511126203,9.92453123330913));
#21140=CARTESIAN_POINT('Ctrl Pts',(8.59489616871569,-15.3867511126203,4.96226561664425));
#21141=CARTESIAN_POINT('Ctrl Pts',(11.4598615582757,-15.2117511126203,-2.06354052510241E-11));
#21142=CARTESIAN_POINT('Ctrl Pts',(8.59489616869782,-15.0367511126203,-4.9622656166752));
#21143=CARTESIAN_POINT('Ctrl Pts',(5.72993077911996,-14.8617511126203,-9.92453123332976));
#21144=CARTESIAN_POINT('Ctrl Pts',(-1.78726082715848E-11,-14.6867511126202,
-9.92453123331945));
#21145=CARTESIAN_POINT('Ctrl Pts',(-5.7299307791557,-14.5117511126203,-9.92453123330913));
#21146=CARTESIAN_POINT('Ctrl Pts',(-8.59489616871569,-14.3367511126203,
-4.96226561664425));
#21147=CARTESIAN_POINT('Ctrl Pts',(-11.4598615582757,-14.1617511126203,
2.06368086793017E-11));
#21148=CARTESIAN_POINT('Ctrl Pts',(-8.59489616869782,-13.9867511126203,
4.9622656166752));
#21149=CARTESIAN_POINT('Ctrl Pts',(-5.72993077911996,-13.8117511126203,
9.92453123332977));
#21150=CARTESIAN_POINT('Ctrl Pts',(1.7871392867044E-11,-13.6367511126203,
9.92453123331945));
#21151=CARTESIAN_POINT('Ctrl Pts',(5.7299307791557,-13.4617511126203,9.92453123330913));
#21152=CARTESIAN_POINT('Ctrl Pts',(8.59489616871569,-13.2867511126203,4.96226561664425));
#21153=CARTESIAN_POINT('Ctrl Pts',(11.4598615582757,-13.1117511126203,-2.06354052510241E-11));
#21154=CARTESIAN_POINT('Ctrl Pts',(8.59489616869782,-12.9367511126203,-4.9622656166752));
#21155=CARTESIAN_POINT('Ctrl Pts',(5.72993077911996,-12.7617511126203,-9.92453123332976));
#21156=CARTESIAN_POINT('Ctrl Pts',(-1.78726082715848E-11,-12.5867511126203,
-9.92453123331945));
#21157=CARTESIAN_POINT('Ctrl Pts',(-5.7299307791557,-12.4117511126203,-9.92453123330913));
#21158=CARTESIAN_POINT('Ctrl Pts',(-8.59489616871569,-12.2367511126203,
-4.96226561664425));
#21159=CARTESIAN_POINT('Ctrl Pts',(-11.4598615582757,-12.0617511126203,
2.06368086793017E-11));
#21160=CARTESIAN_POINT('Ctrl Pts',(-8.59489616869782,-11.8867511126203,
4.9622656166752));
#21161=CARTESIAN_POINT('Ctrl Pts',(-5.72993077911996,-11.7117511126203,
9.92453123332977));
#21162=CARTESIAN_POINT('Ctrl Pts',(1.7871392867044E-11,-11.5367511126203,
9.92453123331945));
#21163=CARTESIAN_POINT('Ctrl Pts',(5.7299307791557,-11.3617511126203,9.92453123330913));
#21164=CARTESIAN_POINT('Ctrl Pts',(8.59489616871569,-11.1867511126203,4.96226561664425));
#21165=CARTESIAN_POINT('Ctrl Pts',(11.4598615582757,-11.0117511126203,-2.06354052510241E-11));
#21166=CARTESIAN_POINT('Ctrl Pts',(8.59489616869782,-10.8367511126203,-4.9622656166752));
#21167=CARTESIAN_POINT('Ctrl Pts',(5.72993077911996,-10.6617511126203,-9.92453123332976));
#21168=CARTESIAN_POINT('Ctrl Pts',(-1.78726082715848E-11,-10.4867511126203,
-9.92453123331945));
#21169=CARTESIAN_POINT('Ctrl Pts',(-5.7299307791557,-10.3117511126203,-9.92453123330913));
#21170=CARTESIAN_POINT('Ctrl Pts',(-8.59489616871569,-10.1367511126203,
-4.96226561664425));
#21171=CARTESIAN_POINT('Ctrl Pts',(-11.4598615582757,-9.96175111262027,
2.06368086793017E-11));
#21172=CARTESIAN_POINT('Ctrl Pts',(-8.59489616869782,-9.78675111262026,
4.9622656166752));
#21173=CARTESIAN_POINT('Ctrl Pts',(-5.72993077911996,-9.61175111262028,
9.92453123332977));
#21174=CARTESIAN_POINT('Ctrl Pts',(1.7871392867044E-11,-9.43675111262027,
9.92453123331945));
#21175=CARTESIAN_POINT('Ctrl Pts',(5.7299307791557,-9.26175111262026,9.92453123330913));
#21176=CARTESIAN_POINT('Ctrl Pts',(8.59489616871569,-9.08675111262028,4.96226561664425));
#21177=CARTESIAN_POINT('Ctrl Pts',(11.4598615582757,-8.91175111262028,-2.06354052510241E-11));
#21178=CARTESIAN_POINT('Ctrl Pts',(8.59489616869782,-8.73675111262026,-4.9622656166752));
#21179=CARTESIAN_POINT('Ctrl Pts',(5.72993077911996,-8.56175111262028,-9.92453123332976));
#21180=CARTESIAN_POINT('Ctrl Pts',(-1.78726082715848E-11,-8.38675111262027,
-9.92453123331945));
#21181=CARTESIAN_POINT('Ctrl Pts',(-5.7299307791557,-8.21175111262026,-9.92453123330913));
#21182=CARTESIAN_POINT('Ctrl Pts',(-8.59489616871569,-8.03675111262028,
-4.96226561664425));
#21183=CARTESIAN_POINT('Ctrl Pts',(-11.4598615582757,-7.86175111262028,
2.06368086793017E-11));
#21184=CARTESIAN_POINT('Ctrl Pts',(-8.59489616869782,-7.68675111262027,
4.9622656166752));
#21185=CARTESIAN_POINT('Ctrl Pts',(-5.72993077911996,-7.51175111262028,
9.92453123332977));
#21186=CARTESIAN_POINT('Ctrl Pts',(1.7871392867044E-11,-7.33675111262028,
9.92453123331945));
#21187=CARTESIAN_POINT('Ctrl Pts',(5.7299307791557,-7.16175111262027,9.92453123330913));
#21188=CARTESIAN_POINT('Ctrl Pts',(8.59489616871569,-6.98675111262029,4.96226561664425));
#21189=CARTESIAN_POINT('Ctrl Pts',(11.4598615582757,-6.81175111262029,-2.06354052510241E-11));
#21190=CARTESIAN_POINT('Ctrl Pts',(8.59489616869782,-6.63675111262027,-4.9622656166752));
#21191=CARTESIAN_POINT('Ctrl Pts',(5.72993077911996,-6.46175111262029,-9.92453123332976));
#21192=CARTESIAN_POINT('Ctrl Pts',(-1.78726082715848E-11,-6.28675111262028,
-9.92453123331945));
#21193=CARTESIAN_POINT('Ctrl Pts',(-5.7299307791557,-6.11175111262027,-9.92453123330913));
#21194=CARTESIAN_POINT('Ctrl Pts',(-8.59489616871569,-5.93675111262026,
-4.96226561664425));
#21195=CARTESIAN_POINT('Ctrl Pts',(-11.4598615582757,-5.76175111262029,
2.06368086793017E-11));
#21196=CARTESIAN_POINT('Ctrl Pts',(-8.59489616869782,-5.58675111262028,
4.9622656166752));
#21197=CARTESIAN_POINT('Ctrl Pts',(-5.72993077911996,-5.41175111262028,
9.92453123332977));
#21198=CARTESIAN_POINT('Ctrl Pts',(1.7871392867044E-11,-5.23675111262029,
9.92453123331945));
#21199=CARTESIAN_POINT('Ctrl Pts',(5.7299307791557,-5.06175111262028,9.92453123330913));
#21200=CARTESIAN_POINT('Ctrl Pts',(8.59489616871569,-4.88675111262027,4.96226561664425));
#21201=CARTESIAN_POINT('Ctrl Pts',(11.4598615582757,-4.7117511126203,-2.06354052510241E-11));
#21202=CARTESIAN_POINT('Ctrl Pts',(8.59489616869782,-4.53675111262028,-4.9622656166752));
#21203=CARTESIAN_POINT('Ctrl Pts',(5.72993077911996,-4.36175111262028,-9.92453123332976));
#21204=CARTESIAN_POINT('Ctrl Pts',(-1.78726082715848E-11,-4.18675111262029,
-9.92453123331945));
#21205=CARTESIAN_POINT('Ctrl Pts',(-5.7299307791557,-4.01175111262028,-9.92453123330913));
#21206=CARTESIAN_POINT('Ctrl Pts',(-8.59489616871569,-3.83675111262027,
-4.96226561664425));
#21207=CARTESIAN_POINT('Ctrl Pts',(-11.4598615582757,-3.6617511126203,2.06368086793017E-11));
#21208=CARTESIAN_POINT('Ctrl Pts',(-8.59489616869782,-3.48675111262029,
4.9622656166752));
#21209=CARTESIAN_POINT('Ctrl Pts',(-5.72993077911996,-3.31175111262029,
9.92453123332977));
#21210=CARTESIAN_POINT('Ctrl Pts',(1.7871392867044E-11,-3.1367511126203,
9.92453123331945));
#21211=CARTESIAN_POINT('Ctrl Pts',(5.7299307791557,-2.96175111262029,9.92453123330913));
#21212=CARTESIAN_POINT('Ctrl Pts',(8.59489616871569,-2.78675111262028,4.96226561664425));
#21213=CARTESIAN_POINT('Ctrl Pts',(11.4598615582757,-2.61175111262031,-2.06354052510241E-11));
#21214=CARTESIAN_POINT('Ctrl Pts',(8.59489616869782,-2.43675111262029,-4.9622656166752));
#21215=CARTESIAN_POINT('Ctrl Pts',(5.72993077911996,-2.26175111262028,-9.92453123332976));
#21216=CARTESIAN_POINT('Ctrl Pts',(-1.78726082715848E-11,-2.0867511126203,
-9.92453123331945));
#21217=CARTESIAN_POINT('Ctrl Pts',(-5.7299307791557,-1.91175111262029,-9.92453123330913));
#21218=CARTESIAN_POINT('Ctrl Pts',(-8.59489616871569,-1.73675111262028,
-4.96226561664425));
#21219=CARTESIAN_POINT('Ctrl Pts',(-11.4598615582757,-1.56175111262028,
2.06368086793017E-11));
#21220=CARTESIAN_POINT('Ctrl Pts',(-8.59489616869782,-1.38675111262029,
4.9622656166752));
#21221=CARTESIAN_POINT('Ctrl Pts',(-5.72993077911996,-1.21175111262029,
9.92453123332977));
#21222=CARTESIAN_POINT('Ctrl Pts',(1.7871392867044E-11,-1.03675111262028,
9.92453123331945));
#21223=CARTESIAN_POINT('Ctrl Pts',(5.7299307791557,-0.861751112620297,9.92453123330913));
#21224=CARTESIAN_POINT('Ctrl Pts',(8.59489616871569,-0.686751112620287,
4.96226561664425));
#21225=CARTESIAN_POINT('Ctrl Pts',(11.4598615582757,-0.511751112620282,
-2.06354052510241E-11));
#21226=CARTESIAN_POINT('Ctrl Pts',(8.59489616869782,-0.336751112620298,
-4.9622656166752));
#21227=CARTESIAN_POINT('Ctrl Pts',(5.72993077911996,-0.161751112620292,
-9.92453123332976));
#21228=CARTESIAN_POINT('Ctrl Pts',(-1.78726082715848E-11,0.0132488873797187,
-9.92453123331945));
#21229=CARTESIAN_POINT('Ctrl Pts',(-5.7299307791557,0.188248887379698,-9.92453123330913));
#21230=CARTESIAN_POINT('Ctrl Pts',(-8.59489616871569,0.363248887379708,
-4.96226561664425));
#21231=CARTESIAN_POINT('Ctrl Pts',(-11.4598615582757,0.538248887379713,
2.06368086793017E-11));
#21232=CARTESIAN_POINT('Ctrl Pts',(-8.59489616869782,0.713248887379697,
4.9622656166752));
#21233=CARTESIAN_POINT('Ctrl Pts',(-5.72993077911996,0.888248887379703,
9.92453123332977));
#21234=CARTESIAN_POINT('Ctrl Pts',(1.7871392867044E-11,1.06324888737971,
9.92453123331945));
#21235=CARTESIAN_POINT('Ctrl Pts',(5.7299307791557,1.23824888737969,9.92453123330913));
#21236=CARTESIAN_POINT('Ctrl Pts',(8.59489616871569,1.4132488873797,4.96226561664425));
#21237=CARTESIAN_POINT('Ctrl Pts',(11.4598615582757,1.58824888737971,-2.06354052510241E-11));
#21238=CARTESIAN_POINT('Ctrl Pts',(8.59489616869782,1.76324888737969,-4.9622656166752));
#21239=CARTESIAN_POINT('Ctrl Pts',(5.72993077911996,1.9382488873797,-9.92453123332976));
#21240=CARTESIAN_POINT('Ctrl Pts',(-1.78726082715848E-11,2.11324888737971,
-9.92453123331945));
#21241=CARTESIAN_POINT('Ctrl Pts',(-5.7299307791557,2.28824888737969,-9.92453123330913));
#21242=CARTESIAN_POINT('Ctrl Pts',(-8.59489616871569,2.4632488873797,-4.96226561664425));
#21243=CARTESIAN_POINT('Ctrl Pts',(-11.4598615582757,2.6382488873797,2.06368086793017E-11));
#21244=CARTESIAN_POINT('Ctrl Pts',(-8.59489616869782,2.81324888737972,4.9622656166752));
#21245=CARTESIAN_POINT('Ctrl Pts',(-5.72993077911996,2.98824888737969,9.92453123332977));
#21246=CARTESIAN_POINT('Ctrl Pts',(1.7871392867044E-11,3.16324888737971,
9.92453123331945));
#21247=CARTESIAN_POINT('Ctrl Pts',(5.7299307791557,3.33824888737971,9.92453123330913));
#21248=CARTESIAN_POINT('Ctrl Pts',(8.59489616871569,3.51324888737969,4.96226561664425));
#21249=CARTESIAN_POINT('Ctrl Pts',(11.4598615582757,3.6882488873797,-2.06354052510241E-11));
#21250=CARTESIAN_POINT('Ctrl Pts',(8.59489616869782,3.86324888737971,-4.9622656166752));
#21251=CARTESIAN_POINT('Ctrl Pts',(5.72993077911996,4.03824888737969,-9.92453123332976));
#21252=CARTESIAN_POINT('Ctrl Pts',(-1.78726082715848E-11,4.2132488873797,
-9.92453123331945));
#21253=CARTESIAN_POINT('Ctrl Pts',(-5.7299307791557,4.3882488873797,-9.92453123330913));
#21254=CARTESIAN_POINT('Ctrl Pts',(-8.59489616871569,4.56324888737969,-4.96226561664425));
#21255=CARTESIAN_POINT('Ctrl Pts',(-11.4598615582757,4.73824888737969,2.06368086793017E-11));
#21256=CARTESIAN_POINT('Ctrl Pts',(-8.59489616869782,4.91324888737971,4.9622656166752));
#21257=CARTESIAN_POINT('Ctrl Pts',(-5.72993077911996,5.08824888737969,9.92453123332977));
#21258=CARTESIAN_POINT('Ctrl Pts',(1.7871392867044E-11,5.2632488873797,
9.92453123331945));
#21259=CARTESIAN_POINT('Ctrl Pts',(5.7299307791557,5.4382488873797,9.92453123330913));
#21260=CARTESIAN_POINT('Ctrl Pts',(8.59489616871569,5.61324888737968,4.96226561664425));
#21261=CARTESIAN_POINT('Ctrl Pts',(11.4598615582757,5.78824888737969,-2.06354052510241E-11));
#21262=CARTESIAN_POINT('Ctrl Pts',(8.59489616869782,5.9632488873797,-4.9622656166752));
#21263=CARTESIAN_POINT('Ctrl Pts',(5.72993077911996,6.13824888737968,-9.92453123332976));
#21264=CARTESIAN_POINT('Ctrl Pts',(-1.78726082715848E-11,6.31324888737969,
-9.92453123331945));
#21265=CARTESIAN_POINT('Ctrl Pts',(-5.7299307791557,6.4882488873797,-9.92453123330913));
#21266=CARTESIAN_POINT('Ctrl Pts',(-8.59489616871569,6.66324888737968,-4.96226561664425));
#21267=CARTESIAN_POINT('Ctrl Pts',(-11.4598615582757,6.83824888737969,2.06368086793017E-11));
#21268=CARTESIAN_POINT('Ctrl Pts',(-8.59489616869782,7.0132488873797,4.9622656166752));
#21269=CARTESIAN_POINT('Ctrl Pts',(-5.72993077911996,7.18824888737968,9.92453123332977));
#21270=CARTESIAN_POINT('Ctrl Pts',(1.7871392867044E-11,7.36324888737969,
9.92453123331945));
#21271=CARTESIAN_POINT('Ctrl Pts',(5.7299307791557,7.53824888737969,9.92453123330913));
#21272=CARTESIAN_POINT('Ctrl Pts',(8.59489616871569,7.7132488873797,4.96226561664425));
#21273=CARTESIAN_POINT('Ctrl Pts',(11.4598615582757,7.88824888737968,-2.06354052510241E-11));
#21274=CARTESIAN_POINT('Ctrl Pts',(8.59489616869782,8.06324888737969,-4.9622656166752));
#21275=CARTESIAN_POINT('Ctrl Pts',(5.72993077911996,8.2382488873797,-9.92453123332976));
#21276=CARTESIAN_POINT('Ctrl Pts',(-1.78726082715848E-11,8.41324888737968,
-9.92453123331945));
#21277=CARTESIAN_POINT('Ctrl Pts',(-5.7299307791557,8.58824888737968,-9.92453123330913));
#21278=CARTESIAN_POINT('Ctrl Pts',(-8.59489616871569,8.7632488873797,-4.96226561664425));
#21279=CARTESIAN_POINT('Ctrl Pts',(-11.4598615582757,8.93824888737968,2.06368086793017E-11));
#21280=CARTESIAN_POINT('Ctrl Pts',(-8.59489616869782,9.11324888737969,4.9622656166752));
#21281=CARTESIAN_POINT('Ctrl Pts',(-5.72993077911996,9.28824888737969,9.92453123332977));
#21282=CARTESIAN_POINT('Ctrl Pts',(1.7871392867044E-11,9.46324888737968,
9.92453123331945));
#21283=CARTESIAN_POINT('Ctrl Pts',(5.7299307791557,9.63824888737968,9.92453123330913));
#21284=CARTESIAN_POINT('Ctrl Pts',(8.59489616871569,9.81324888737969,4.96226561664425));
#21285=CARTESIAN_POINT('Ctrl Pts',(11.4598615582757,9.98824888737967,-2.06354052510241E-11));
#21286=CARTESIAN_POINT('Ctrl Pts',(8.59489616869782,10.1632488873797,-4.9622656166752));
#21287=CARTESIAN_POINT('Ctrl Pts',(5.72993077911996,10.3382488873797,-9.92453123332976));
#21288=CARTESIAN_POINT('Ctrl Pts',(-1.78726082715848E-11,10.5132488873797,
-9.92453123331945));
#21289=CARTESIAN_POINT('Ctrl Pts',(-5.7299307791557,10.6882488873797,-9.92453123330913));
#21290=CARTESIAN_POINT('Ctrl Pts',(-8.59489616871569,10.8632488873797,-4.96226561664425));
#21291=CARTESIAN_POINT('Ctrl Pts',(-11.4598615582757,11.0382488873797,2.06368086793017E-11));
#21292=CARTESIAN_POINT('Ctrl Pts',(-8.59489616869782,11.2132488873797,4.9622656166752));
#21293=CARTESIAN_POINT('Ctrl Pts',(-5.72993077911996,11.3882488873797,9.92453123332977));
#21294=CARTESIAN_POINT('Ctrl Pts',(1.7871392867044E-11,11.5632488873797,
9.92453123331945));
#21295=CARTESIAN_POINT('Ctrl Pts',(5.7299307791557,11.7382488873797,9.92453123330913));
#21296=CARTESIAN_POINT('Ctrl Pts',(8.59489616871569,11.9132488873797,4.96226561664425));
#21297=CARTESIAN_POINT('Ctrl Pts',(11.4598615582757,12.0882488873797,-2.06354052510241E-11));
#21298=CARTESIAN_POINT('Ctrl Pts',(8.59489616869782,12.2632488873797,-4.9622656166752));
#21299=CARTESIAN_POINT('Ctrl Pts',(5.72993077911996,12.4382488873797,-9.92453123332976));
#21300=CARTESIAN_POINT('Ctrl Pts',(-1.78726082715848E-11,12.6132488873797,
-9.92453123331945));
#21301=CARTESIAN_POINT('Ctrl Pts',(-5.7299307791557,12.7882488873797,-9.92453123330913));
#21302=CARTESIAN_POINT('Ctrl Pts',(-8.59489616871569,12.9632488873797,-4.96226561664425));
#21303=CARTESIAN_POINT('Ctrl Pts',(-11.4598615582757,13.1382488873797,2.06368086793017E-11));
#21304=CARTESIAN_POINT('Ctrl Pts',(-8.59489616869782,13.3132488873797,4.9622656166752));
#21305=CARTESIAN_POINT('Ctrl Pts',(-5.72993077911996,13.4882488873797,9.92453123332977));
#21306=CARTESIAN_POINT('Ctrl Pts',(1.7871392867044E-11,13.6632488873797,
9.92453123331945));
#21307=CARTESIAN_POINT('Ctrl Pts',(5.7299307791557,13.8382488873797,9.92453123330913));
#21308=CARTESIAN_POINT('Ctrl Pts',(8.59489616871569,14.0132488873797,4.96226561664425));
#21309=CARTESIAN_POINT('Ctrl Pts',(11.4598615582757,14.1882488873797,-2.06354052510241E-11));
#21310=CARTESIAN_POINT('Ctrl Pts',(8.59489616869782,14.3632488873797,-4.9622656166752));
#21311=CARTESIAN_POINT('Ctrl Pts',(5.72993077911996,14.5382488873797,-9.92453123332976));
#21312=CARTESIAN_POINT('Ctrl Pts',(-1.78726082715848E-11,14.7132488873797,
-9.92453123331945));
#21313=CARTESIAN_POINT('Ctrl Pts',(-5.7299307791557,14.8882488873797,-9.92453123330913));
#21314=CARTESIAN_POINT('Ctrl Pts',(-8.59489616871569,15.0632488873797,-4.96226561664425));
#21315=CARTESIAN_POINT('Ctrl Pts',(-11.4598615582757,15.2382488873797,2.06368086793017E-11));
#21316=CARTESIAN_POINT('Ctrl Pts',(-8.59489616869782,15.4132488873797,4.9622656166752));
#21317=CARTESIAN_POINT('Ctrl Pts',(-5.72993077911996,15.5882488873797,9.92453123332977));
#21318=CARTESIAN_POINT('Ctrl Pts',(1.7871392867044E-11,15.7632488873797,
9.92453123331945));
#21319=CARTESIAN_POINT('Ctrl Pts',(5.7299307791557,15.9382488873797,9.92453123330913));
#21320=CARTESIAN_POINT('Ctrl Pts',(8.59489616871569,16.1132488873797,4.96226561664425));
#21321=CARTESIAN_POINT('Ctrl Pts',(11.4598615582757,16.2882488873797,-2.06354052510241E-11));
#21322=CARTESIAN_POINT('Ctrl Pts',(8.59489616869782,16.4632488873797,-4.9622656166752));
#21323=CARTESIAN_POINT('Ctrl Pts',(5.72993077911996,16.6382488873797,-9.92453123332976));
#21324=CARTESIAN_POINT('Ctrl Pts',(-1.78726082715848E-11,16.8132488873797,
-9.92453123331945));
#21325=CARTESIAN_POINT('Ctrl Pts',(-5.7299307791557,16.9882488873797,-9.92453123330913));
#21326=CARTESIAN_POINT('Ctrl Pts',(-8.59489616871569,17.1632488873797,-4.96226561664425));
#21327=CARTESIAN_POINT('Ctrl Pts',(-11.4598615582757,17.3382488873797,2.06368086793017E-11));
#21328=CARTESIAN_POINT('Ctrl Pts',(-8.59489616869782,17.5132488873797,4.9622656166752));
#21329=CARTESIAN_POINT('Ctrl Pts',(-5.72993077911996,17.6882488873797,9.92453123332977));
#21330=CARTESIAN_POINT('Ctrl Pts',(1.7871392867044E-11,17.8632488873797,
9.92453123331945));
#21331=CARTESIAN_POINT('Ctrl Pts',(5.7299307791557,18.0382488873797,9.92453123330913));
#21332=CARTESIAN_POINT('Ctrl Pts',(8.59489616871569,18.2132488873797,4.96226561664425));
#21333=CARTESIAN_POINT('Ctrl Pts',(11.4598615582757,18.3882488873797,-2.06354052510241E-11));
#21334=CARTESIAN_POINT('Ctrl Pts',(8.59489616869782,18.5632488873797,-4.9622656166752));
#21335=CARTESIAN_POINT('Ctrl Pts',(5.72993077911996,18.7382488873796,-9.92453123332976));
#21336=CARTESIAN_POINT('Ctrl Pts',(-1.78726082715848E-11,18.9132488873797,
-9.92453123331945));
#21337=CARTESIAN_POINT('Ctrl Pts',(-5.7299307791557,19.0882488873797,-9.92453123330913));
#21338=CARTESIAN_POINT('Ctrl Pts',(-8.59489616871569,19.2632488873797,-4.96226561664425));
#21339=CARTESIAN_POINT('Ctrl Pts',(-11.4598615582757,19.4382488873797,2.06368086793017E-11));
#21340=CARTESIAN_POINT('Ctrl Pts',(-8.59489616869782,19.6132488873797,4.9622656166752));
#21341=CARTESIAN_POINT('Ctrl Pts',(-5.72993077911996,19.7882488873796,9.92453123332977));
#21342=CARTESIAN_POINT('Ctrl Pts',(1.7871392867044E-11,19.9632488873797,
9.92453123331945));
#21343=CARTESIAN_POINT('Ctrl Pts',(5.7299307791557,20.1382488873797,9.92453123330913));
#21344=CARTESIAN_POINT('Ctrl Pts',(8.59489616871569,20.3132488873796,4.96226561664425));
#21345=CARTESIAN_POINT('Ctrl Pts',(11.4598615582757,20.4882488873796,-2.06354052510241E-11));
#21346=CARTESIAN_POINT('Ctrl Pts',(8.59489616869782,20.6632488873797,-4.9622656166752));
#21347=CARTESIAN_POINT('Ctrl Pts',(5.72993077911996,20.8382488873797,-9.92453123332976));
#21348=CARTESIAN_POINT('Ctrl Pts',(-1.78726082715848E-11,21.0132488873797,
-9.92453123331945));
#21349=CARTESIAN_POINT('Ctrl Pts',(-5.7299307791557,21.1882488873797,-9.92453123330913));
#21350=CARTESIAN_POINT('Ctrl Pts',(-8.59489616871569,21.3632488873797,-4.96226561664425));
#21351=CARTESIAN_POINT('Ctrl Pts',(-11.4598615582757,21.5382488873796,2.06368086793017E-11));
#21352=CARTESIAN_POINT('Ctrl Pts',(-8.59489616869782,21.7132488873797,4.9622656166752));
#21353=CARTESIAN_POINT('Ctrl Pts',(-5.72993077911996,21.8882488873797,9.92453123332977));
#21354=CARTESIAN_POINT('Ctrl Pts',(1.7871392867044E-11,22.0632488873797,
9.92453123331945));
#21355=CARTESIAN_POINT('Ctrl Pts',(5.7299307791557,22.2382488873797,9.92453123330913));
#21356=CARTESIAN_POINT('Ctrl Pts',(8.59489616871569,22.4132488873797,4.96226561664425));
#21357=CARTESIAN_POINT('Ctrl Pts',(11.4598615582757,22.5882488873796,-2.06354052510241E-11));
#21358=CARTESIAN_POINT('Ctrl Pts',(8.59489616869782,22.7632488873797,-4.9622656166752));
#21359=CARTESIAN_POINT('Ctrl Pts',(5.72993077911996,22.9382488873797,-9.92453123332976));
#21360=CARTESIAN_POINT('Ctrl Pts',(-1.78726082715848E-11,23.1132488873796,
-9.92453123331945));
#21361=CARTESIAN_POINT('Ctrl Pts',(-5.7299307791557,23.2882488873797,-9.92453123330913));
#21362=CARTESIAN_POINT('Ctrl Pts',(-8.59489616871569,23.4632488873797,-4.96226561664425));
#21363=CARTESIAN_POINT('Ctrl Pts',(-11.4598615582757,23.6382488873796,2.06368086793017E-11));
#21364=CARTESIAN_POINT('Ctrl Pts',(-8.59489616869782,23.8132488873797,4.9622656166752));
#21365=CARTESIAN_POINT('Ctrl Pts',(-5.72993077911996,23.9882488873797,9.92453123332977));
#21366=CARTESIAN_POINT('Ctrl Pts',(1.7871392867044E-11,24.1632488873796,
9.92453123331945));
#21367=CARTESIAN_POINT('Ctrl Pts',(5.7299307791557,24.3382488873796,9.92453123330913));
#21368=CARTESIAN_POINT('Ctrl Pts',(8.59489616871569,24.5132488873797,4.96226561664425));
#21369=CARTESIAN_POINT('Ctrl Pts',(11.4598615582757,24.6882488873796,-2.06354052510241E-11));
#21370=CARTESIAN_POINT('Ctrl Pts',(8.59489616869782,24.8632488873796,-4.9622656166752));
#21371=CARTESIAN_POINT('Ctrl Pts',(5.72993077911996,25.0382488873797,-9.92453123332976));
#21372=CARTESIAN_POINT('Ctrl Pts',(-1.78726082715848E-11,25.2132488873796,
-9.92453123331945));
#21373=CARTESIAN_POINT('Ctrl Pts',(-5.7299307791557,25.3882488873796,-9.92453123330913));
#21374=CARTESIAN_POINT('Ctrl Pts',(-8.59489616871569,25.5632488873797,-4.96226561664425));
#21375=CARTESIAN_POINT('Ctrl Pts',(-11.4598615582757,25.7382488873797,2.06368086793017E-11));
#21376=CARTESIAN_POINT('Ctrl Pts',(-8.59489616869782,25.9132488873796,4.9622656166752));
#21377=CARTESIAN_POINT('Ctrl Pts',(-5.72993077911996,26.0882488873797,9.92453123332977));
#21378=CARTESIAN_POINT('Ctrl Pts',(1.7871392867044E-11,26.2632488873797,
9.92453123331945));
#21379=CARTESIAN_POINT('Ctrl Pts',(5.7299307791557,26.4382488873796,9.92453123330913));
#21380=CARTESIAN_POINT('Ctrl Pts',(8.59489616871569,26.6132488873797,4.96226561664425));
#21381=CARTESIAN_POINT('Ctrl Pts',(11.4598615582757,26.7882488873797,-2.06354052510241E-11));
#21382=CARTESIAN_POINT('Ctrl Pts',(8.59489616869782,26.9632488873796,-4.9622656166752));
#21383=CARTESIAN_POINT('Ctrl Pts',(5.72993077911996,27.1382488873796,-9.92453123332976));
#21384=CARTESIAN_POINT('Ctrl Pts',(-1.78726082715848E-11,27.3132488873797,
-9.92453123331945));
#21385=CARTESIAN_POINT('Ctrl Pts',(-1.22646583495775,-24.9756402675196,
8.31163887211714));
#21386=CARTESIAN_POINT('Ctrl Pts',(-0.616535190940158,-24.9517609250221,
8.40164026752071));
#21387=CARTESIAN_POINT('Ctrl Pts',(1.49242955500311E-11,-24.9295179709985,
8.40164026751963));
#21388=CARTESIAN_POINT('Ctrl Pts',(4.85068927010145,-24.7545179709985,8.40164026751121));
#21389=CARTESIAN_POINT('Ctrl Pts',(7.27603390513766,-24.5795179709986,4.20082013374705));
#21390=CARTESIAN_POINT('Ctrl Pts',(9.70137854017372,-24.4045179709986,-1.71807987380788E-11));
#21391=CARTESIAN_POINT('Ctrl Pts',(7.27603390512277,-24.2295179709986,-4.20082013377283));
#21392=CARTESIAN_POINT('Ctrl Pts',(4.85068927007217,-24.0545179709986,-8.40164026752811));
#21393=CARTESIAN_POINT('Ctrl Pts',(-1.48337207789367E-11,-23.8795179709986,
-8.40164026751963));
#21394=CARTESIAN_POINT('Ctrl Pts',(-4.85068927010184,-23.7045179709986,
-8.40164026751098));
#21395=CARTESIAN_POINT('Ctrl Pts',(-7.27603390513761,-23.5295179709985,
-4.20082013374713));
#21396=CARTESIAN_POINT('Ctrl Pts',(-9.70137854017372,-23.3545179709986,
1.70762120011325E-11));
#21397=CARTESIAN_POINT('Ctrl Pts',(-7.27603390512282,-23.1795179709986,
4.20082013377275));
#21398=CARTESIAN_POINT('Ctrl Pts',(-4.85068927007226,-23.0045179709986,
8.40164026752806));
#21399=CARTESIAN_POINT('Ctrl Pts',(1.47431460078422E-11,-22.8295179709986,
8.40164026751963));
#21400=CARTESIAN_POINT('Ctrl Pts',(4.85068927010175,-22.6545179709986,8.40164026751103));
#21401=CARTESIAN_POINT('Ctrl Pts',(7.2760339051378,-22.4795179709986,4.2008201337468));
#21402=CARTESIAN_POINT('Ctrl Pts',(9.70137854017372,-22.3045179709986,-1.69716252641861E-11));
#21403=CARTESIAN_POINT('Ctrl Pts',(7.27603390512287,-22.1295179709986,-4.20082013377267));
#21404=CARTESIAN_POINT('Ctrl Pts',(4.85068927007187,-21.9545179709986,-8.40164026752828));
#21405=CARTESIAN_POINT('Ctrl Pts',(-1.46525712367478E-11,-21.7795179709986,
-8.40164026751963));
#21406=CARTESIAN_POINT('Ctrl Pts',(-4.85068927010165,-21.6045179709986,
-8.40164026751109));
#21407=CARTESIAN_POINT('Ctrl Pts',(-7.27603390513776,-21.4295179709986,
-4.20082013374688));
#21408=CARTESIAN_POINT('Ctrl Pts',(-9.70137854017372,-21.2545179709986,
1.68670385272398E-11));
#21409=CARTESIAN_POINT('Ctrl Pts',(-7.27603390512291,-21.0795179709986,
4.20082013377259));
#21410=CARTESIAN_POINT('Ctrl Pts',(-4.85068927007196,-20.9045179709986,
8.40164026752823));
#21411=CARTESIAN_POINT('Ctrl Pts',(1.45619964656533E-11,-20.7295179709986,
8.40164026751963));
#21412=CARTESIAN_POINT('Ctrl Pts',(4.85068927010157,-20.5545179709986,8.40164026751114));
#21413=CARTESIAN_POINT('Ctrl Pts',(7.27603390513771,-20.3795179709986,4.20082013374695));
#21414=CARTESIAN_POINT('Ctrl Pts',(9.70137854017372,-20.2045179709986,-1.73139113141798E-11));
#21415=CARTESIAN_POINT('Ctrl Pts',(7.27603390512296,-20.0295179709986,-4.20082013377251));
#21416=CARTESIAN_POINT('Ctrl Pts',(4.85068927007205,-19.8545179709986,-8.40164026752818));
#21417=CARTESIAN_POINT('Ctrl Pts',(-1.49489996514033E-11,-19.6795179709986,
-8.40164026751963));
#21418=CARTESIAN_POINT('Ctrl Pts',(-4.85068927010147,-19.5045179709986,
-8.40164026751119));
#21419=CARTESIAN_POINT('Ctrl Pts',(-7.27603390513767,-19.3295179709986,
-4.20082013374703));
#21420=CARTESIAN_POINT('Ctrl Pts',(-9.70137854017372,-19.1545179709986,
1.72093245772335E-11));
#21421=CARTESIAN_POINT('Ctrl Pts',(-7.276033905123,-18.9795179709986,4.20082013377243));
#21422=CARTESIAN_POINT('Ctrl Pts',(-4.85068927007214,-18.8045179709986,
8.40164026752813));
#21423=CARTESIAN_POINT('Ctrl Pts',(1.48584248803088E-11,-18.6295179709986,
8.40164026751963));
#21424=CARTESIAN_POINT('Ctrl Pts',(4.85068927010186,-18.4545179709986,8.40164026751097));
#21425=CARTESIAN_POINT('Ctrl Pts',(7.27603390513762,-18.2795179709986,4.20082013374711));
#21426=CARTESIAN_POINT('Ctrl Pts',(9.70137854017372,-18.1045179709986,-1.71047378402871E-11));
#21427=CARTESIAN_POINT('Ctrl Pts',(7.27603390512281,-17.9295179709986,-4.20082013377277));
#21428=CARTESIAN_POINT('Ctrl Pts',(4.85068927007223,-17.7545179709986,-8.40164026752807));
#21429=CARTESIAN_POINT('Ctrl Pts',(-1.47678501092144E-11,-17.5795179709986,
-8.40164026751963));
#21430=CARTESIAN_POINT('Ctrl Pts',(-4.85068927010177,-17.4045179709986,
-8.40164026751102));
#21431=CARTESIAN_POINT('Ctrl Pts',(-7.27603390513758,-17.2295179709986,
-4.20082013374719));
#21432=CARTESIAN_POINT('Ctrl Pts',(-9.70137854017372,-17.0545179709986,
1.70001511033408E-11));
#21433=CARTESIAN_POINT('Ctrl Pts',(-7.27603390512285,-16.8795179709986,
4.20082013377269));
#21434=CARTESIAN_POINT('Ctrl Pts',(-4.85068927007185,-16.7045179709986,
8.4016402675283));
#21435=CARTESIAN_POINT('Ctrl Pts',(1.46772753381199E-11,-16.5295179709986,
8.40164026751963));
#21436=CARTESIAN_POINT('Ctrl Pts',(4.85068927010168,-16.3545179709986,8.40164026751107));
#21437=CARTESIAN_POINT('Ctrl Pts',(7.27603390513777,-16.1795179709986,4.20082013374685));
#21438=CARTESIAN_POINT('Ctrl Pts',(9.70137854017372,-16.0045179709986,-1.68955643663944E-11));
#21439=CARTESIAN_POINT('Ctrl Pts',(7.2760339051229,-15.8295179709986,-4.20082013377261));
#21440=CARTESIAN_POINT('Ctrl Pts',(4.85068927007194,-15.6545179709986,-8.40164026752825));
#21441=CARTESIAN_POINT('Ctrl Pts',(-1.45867005670255E-11,-15.4795179709986,
-8.40164026751963));
#21442=CARTESIAN_POINT('Ctrl Pts',(-4.85068927010159,-15.3045179709986,
-8.40164026751112));
#21443=CARTESIAN_POINT('Ctrl Pts',(-7.27603390513773,-15.1295179709986,
-4.20082013374693));
#21444=CARTESIAN_POINT('Ctrl Pts',(-9.70137854017372,-14.9545179709986,
1.67909776294481E-11));
#21445=CARTESIAN_POINT('Ctrl Pts',(-7.27603390512294,-14.7795179709986,
4.20082013377253));
#21446=CARTESIAN_POINT('Ctrl Pts',(-4.85068927007203,-14.6045179709986,
8.40164026752819));
#21447=CARTESIAN_POINT('Ctrl Pts',(1.49737037527755E-11,-14.4295179709986,
8.40164026751963));
#21448=CARTESIAN_POINT('Ctrl Pts',(4.8506892701015,-14.2545179709986,8.40164026751117));
#21449=CARTESIAN_POINT('Ctrl Pts',(7.27603390513768,-14.0795179709986,4.20082013374701));
#21450=CARTESIAN_POINT('Ctrl Pts',(9.70137854017372,-13.9045179709986,-1.72378504163881E-11));
#21451=CARTESIAN_POINT('Ctrl Pts',(7.27603390512299,-13.7295179709986,-4.20082013377245));
#21452=CARTESIAN_POINT('Ctrl Pts',(4.85068927007212,-13.5545179709986,-8.40164026752814));
#21453=CARTESIAN_POINT('Ctrl Pts',(-1.4883128981681E-11,-13.3795179709986,
-8.40164026751963));
#21454=CARTESIAN_POINT('Ctrl Pts',(-4.85068927010141,-13.2045179709986,
-8.40164026751123));
#21455=CARTESIAN_POINT('Ctrl Pts',(-7.27603390513763,-13.0295179709986,
-4.20082013374709));
#21456=CARTESIAN_POINT('Ctrl Pts',(-9.70137854017372,-12.8545179709986,
1.71332636794417E-11));
#21457=CARTESIAN_POINT('Ctrl Pts',(-7.2760339051228,-12.6795179709986,4.20082013377279));
#21458=CARTESIAN_POINT('Ctrl Pts',(-4.85068927007221,-12.5045179709986,
8.40164026752809));
#21459=CARTESIAN_POINT('Ctrl Pts',(1.47925542105866E-11,-12.3295179709986,
8.40164026751963));
#21460=CARTESIAN_POINT('Ctrl Pts',(4.85068927010179,-12.1545179709986,8.401640267511));
#21461=CARTESIAN_POINT('Ctrl Pts',(7.27603390513759,-11.9795179709986,4.20082013374717));
#21462=CARTESIAN_POINT('Ctrl Pts',(9.70137854017372,-11.8045179709986,-1.70286769424954E-11));
#21463=CARTESIAN_POINT('Ctrl Pts',(7.27603390512284,-11.6295179709986,-4.20082013377271));
#21464=CARTESIAN_POINT('Ctrl Pts',(4.8506892700723,-11.4545179709986,-8.40164026752804));
#21465=CARTESIAN_POINT('Ctrl Pts',(-1.47019794394921E-11,-11.2795179709986,
-8.40164026751963));
#21466=CARTESIAN_POINT('Ctrl Pts',(-4.8506892701017,-11.1045179709986,-8.40164026751106));
#21467=CARTESIAN_POINT('Ctrl Pts',(-7.27603390513778,-10.9295179709986,
-4.20082013374683));
#21468=CARTESIAN_POINT('Ctrl Pts',(-9.70137854017372,-10.7545179709986,
1.69240902055491E-11));
#21469=CARTESIAN_POINT('Ctrl Pts',(-7.27603390512289,-10.5795179709986,
4.20082013377263));
#21470=CARTESIAN_POINT('Ctrl Pts',(-4.85068927007191,-10.4045179709986,
8.40164026752826));
#21471=CARTESIAN_POINT('Ctrl Pts',(1.46114046683977E-11,-10.2295179709986,
8.40164026751963));
#21472=CARTESIAN_POINT('Ctrl Pts',(4.85068927010161,-10.0545179709986,8.40164026751111));
#21473=CARTESIAN_POINT('Ctrl Pts',(7.27603390513774,-9.87951797099859,4.20082013374691));
#21474=CARTESIAN_POINT('Ctrl Pts',(9.70137854017372,-9.70451797099858,-1.68195034686027E-11));
#21475=CARTESIAN_POINT('Ctrl Pts',(7.27603390512293,-9.52951797099857,-4.20082013377256));
#21476=CARTESIAN_POINT('Ctrl Pts',(4.850689270072,-9.3545179709986,-8.40164026752821));
#21477=CARTESIAN_POINT('Ctrl Pts',(-1.49984078541476E-11,-9.17951797099859,
-8.40164026751963));
#21478=CARTESIAN_POINT('Ctrl Pts',(-4.85068927010152,-9.00451797099859,
-8.40164026751116));
#21479=CARTESIAN_POINT('Ctrl Pts',(-7.27603390513769,-8.8295179709986,-4.20082013374699));
#21480=CARTESIAN_POINT('Ctrl Pts',(-9.70137854017372,-8.65451797099859,
1.72663762555427E-11));
#21481=CARTESIAN_POINT('Ctrl Pts',(-7.27603390512298,-8.47951797099858,
4.20082013377248));
#21482=CARTESIAN_POINT('Ctrl Pts',(-4.85068927007209,-8.3045179709986,8.40164026752815));
#21483=CARTESIAN_POINT('Ctrl Pts',(1.49078330830532E-11,-8.12951797099859,
8.40164026751963));
#21484=CARTESIAN_POINT('Ctrl Pts',(4.85068927010143,-7.95451797099859,8.40164026751122));
#21485=CARTESIAN_POINT('Ctrl Pts',(7.27603390513765,-7.7795179709986,4.20082013374707));
#21486=CARTESIAN_POINT('Ctrl Pts',(9.70137854017372,-7.60451797099859,-1.71617895185964E-11));
#21487=CARTESIAN_POINT('Ctrl Pts',(7.27603390512302,-7.42951797099858,-4.2008201337724));
#21488=CARTESIAN_POINT('Ctrl Pts',(4.85068927007219,-7.25451797099861,-8.4016402675281));
#21489=CARTESIAN_POINT('Ctrl Pts',(-1.48172583119587E-11,-7.07951797099859,
-8.40164026751963));
#21490=CARTESIAN_POINT('Ctrl Pts',(-4.85068927010182,-6.90451797099859,
-8.40164026751099));
#21491=CARTESIAN_POINT('Ctrl Pts',(-7.2760339051376,-6.72951797099858,-4.20082013374715));
#21492=CARTESIAN_POINT('Ctrl Pts',(-9.70137854017372,-6.5545179709986,1.705720278165E-11));
#21493=CARTESIAN_POINT('Ctrl Pts',(-7.27603390512283,-6.37951797099859,
4.20082013377273));
#21494=CARTESIAN_POINT('Ctrl Pts',(-4.85068927007227,-6.20451797099858,
8.40164026752805));
#21495=CARTESIAN_POINT('Ctrl Pts',(1.47266835408643E-11,-6.0295179709986,
8.40164026751963));
#21496=CARTESIAN_POINT('Ctrl Pts',(4.85068927010173,-5.8545179709986,8.40164026751104));
#21497=CARTESIAN_POINT('Ctrl Pts',(7.27603390513756,-5.67951797099858,4.20082013374722));
#21498=CARTESIAN_POINT('Ctrl Pts',(9.70137854017372,-5.5045179709986,-1.69526160447037E-11));
#21499=CARTESIAN_POINT('Ctrl Pts',(7.27603390512287,-5.32951797099859,-4.20082013377265));
#21500=CARTESIAN_POINT('Ctrl Pts',(4.85068927007189,-5.15451797099859,-8.40164026752827));
#21501=CARTESIAN_POINT('Ctrl Pts',(-1.46361087697698E-11,-4.9795179709986,
-8.40164026751963));
#21502=CARTESIAN_POINT('Ctrl Pts',(-4.85068927010164,-4.8045179709986,-8.40164026751109));
#21503=CARTESIAN_POINT('Ctrl Pts',(-7.27603390513775,-4.62951797099859,
-4.20082013374689));
#21504=CARTESIAN_POINT('Ctrl Pts',(-9.70137854017372,-4.45451797099861,
1.68480293077573E-11));
#21505=CARTESIAN_POINT('Ctrl Pts',(-7.27603390512292,-4.2795179709986,4.20082013377258));
#21506=CARTESIAN_POINT('Ctrl Pts',(-4.85068927007198,-4.10451797099859,
8.40164026752822));
#21507=CARTESIAN_POINT('Ctrl Pts',(1.45455339986754E-11,-3.92951797099861,
8.40164026751963));
#21508=CARTESIAN_POINT('Ctrl Pts',(4.85068927010155,-3.75451797099861,8.40164026751115));
#21509=CARTESIAN_POINT('Ctrl Pts',(7.2760339051377,-3.57951797099859,4.20082013374697));
#21510=CARTESIAN_POINT('Ctrl Pts',(9.70137854017372,-3.40451797099861,-1.72949020946973E-11));
#21511=CARTESIAN_POINT('Ctrl Pts',(7.27603390512296,-3.2295179709986,-4.2008201337725));
#21512=CARTESIAN_POINT('Ctrl Pts',(4.85068927007207,-3.0545179709986,-8.40164026752817));
#21513=CARTESIAN_POINT('Ctrl Pts',(-1.49325371844254E-11,-2.87951797099861,
-8.40164026751963));
#21514=CARTESIAN_POINT('Ctrl Pts',(-4.85068927010146,-2.70451797099861,
-8.4016402675112));
#21515=CARTESIAN_POINT('Ctrl Pts',(-7.27603390513766,-2.5295179709986,-4.20082013374705));
#21516=CARTESIAN_POINT('Ctrl Pts',(-9.70137854017372,-2.3545179709986,1.7190315357751E-11));
#21517=CARTESIAN_POINT('Ctrl Pts',(-7.27603390512301,-2.17951797099861,
4.20082013377242));
#21518=CARTESIAN_POINT('Ctrl Pts',(-4.85068927007216,-2.0045179709986,8.40164026752812));
#21519=CARTESIAN_POINT('Ctrl Pts',(1.48419624133309E-11,-1.82951797099859,
8.40164026751963));
#21520=CARTESIAN_POINT('Ctrl Pts',(4.85068927010137,-1.65451797099861,8.40164026751125));
#21521=CARTESIAN_POINT('Ctrl Pts',(7.27603390513761,-1.4795179709986,4.20082013374713));
#21522=CARTESIAN_POINT('Ctrl Pts',(9.70137854017372,-1.3045179709986,-1.70857286208046E-11));
#21523=CARTESIAN_POINT('Ctrl Pts',(7.27603390512282,-1.12951797099861,-4.20082013377275));
#21524=CARTESIAN_POINT('Ctrl Pts',(4.85068927007225,-0.954517970998605,
-8.40164026752806));
#21525=CARTESIAN_POINT('Ctrl Pts',(-1.47513876422365E-11,-0.779517970998594,
-8.40164026751963));
#21526=CARTESIAN_POINT('Ctrl Pts',(-4.85068927010175,-0.604517970998614,
-8.40164026751103));
#21527=CARTESIAN_POINT('Ctrl Pts',(-7.27603390513757,-0.429517970998605,
-4.2008201337472));
#21528=CARTESIAN_POINT('Ctrl Pts',(-9.70137854017372,-0.2545179709986,1.69811418838583E-11));
#21529=CARTESIAN_POINT('Ctrl Pts',(-7.27603390512286,-0.079517970998616,
4.20082013377267));
#21530=CARTESIAN_POINT('Ctrl Pts',(-4.85068927007234,0.0954820290013905,
8.40164026752801));
#21531=CARTESIAN_POINT('Ctrl Pts',(1.4660812871142E-11,0.270482029001401,
8.40164026751963));
#21532=CARTESIAN_POINT('Ctrl Pts',(4.85068927010166,0.445482029001381,8.40164026751108));
#21533=CARTESIAN_POINT('Ctrl Pts',(7.27603390513776,0.62048202900139,4.20082013374687));
#21534=CARTESIAN_POINT('Ctrl Pts',(9.70137854017372,0.795482029001396,-1.6876555146912E-11));
#21535=CARTESIAN_POINT('Ctrl Pts',(7.27603390512291,0.970482029001379,-4.2008201337726));
#21536=CARTESIAN_POINT('Ctrl Pts',(4.85068927007195,1.14548202900139,-8.40164026752823));
#21537=CARTESIAN_POINT('Ctrl Pts',(-1.45702381000475E-11,1.3204820290014,
-8.40164026751963));
#21538=CARTESIAN_POINT('Ctrl Pts',(-4.85068927010157,1.49548202900138,-8.40164026751113));
#21539=CARTESIAN_POINT('Ctrl Pts',(-7.27603390513772,1.67048202900139,-4.20082013374695));
#21540=CARTESIAN_POINT('Ctrl Pts',(-9.70137854017372,1.84548202900139,1.67719684099656E-11));
#21541=CARTESIAN_POINT('Ctrl Pts',(-7.27603390512295,2.0204820290014,4.20082013377252));
#21542=CARTESIAN_POINT('Ctrl Pts',(-4.85068927007204,2.19548202900138,8.40164026752818));
#21543=CARTESIAN_POINT('Ctrl Pts',(1.49572412857975E-11,2.37048202900139,
8.40164026751963));
#21544=CARTESIAN_POINT('Ctrl Pts',(4.85068927010148,2.5454820290014,8.40164026751119));
#21545=CARTESIAN_POINT('Ctrl Pts',(7.27603390513767,2.72048202900138,4.20082013374703));
#21546=CARTESIAN_POINT('Ctrl Pts',(9.70137854017372,2.89548202900139,-1.72188411969056E-11));
#21547=CARTESIAN_POINT('Ctrl Pts',(7.276033905123,3.0704820290014,-4.20082013377244));
#21548=CARTESIAN_POINT('Ctrl Pts',(4.85068927007213,3.24548202900138,-8.40164026752813));
#21549=CARTESIAN_POINT('Ctrl Pts',(-1.48666665147031E-11,3.42048202900139,
-8.40164026751963));
#21550=CARTESIAN_POINT('Ctrl Pts',(-4.85068927010139,3.59548202900139,-8.40164026751124));
#21551=CARTESIAN_POINT('Ctrl Pts',(-7.27603390513763,3.77048202900138,-4.2008201337471));
#21552=CARTESIAN_POINT('Ctrl Pts',(-9.70137854017372,3.94548202900138,1.71142544599593E-11));
#21553=CARTESIAN_POINT('Ctrl Pts',(-7.27603390512304,4.12048202900139,4.20082013377236));
#21554=CARTESIAN_POINT('Ctrl Pts',(-4.85068927007222,4.29548202900137,8.40164026752808));
#21555=CARTESIAN_POINT('Ctrl Pts',(1.47760917436086E-11,4.47048202900138,
8.40164026751963));
#21556=CARTESIAN_POINT('Ctrl Pts',(4.85068927010178,4.64548202900139,8.40164026751101));
#21557=CARTESIAN_POINT('Ctrl Pts',(7.27603390513758,4.82048202900137,4.20082013374718));
#21558=CARTESIAN_POINT('Ctrl Pts',(9.70137854017372,4.99548202900138,-1.70096677230129E-11));
#21559=CARTESIAN_POINT('Ctrl Pts',(7.27603390512285,5.17048202900139,-4.2008201337727));
#21560=CARTESIAN_POINT('Ctrl Pts',(4.85068927007232,5.34548202900137,-8.40164026752803));
#21561=CARTESIAN_POINT('Ctrl Pts',(-1.46855169725142E-11,5.52048202900138,
-8.40164026751963));
#21562=CARTESIAN_POINT('Ctrl Pts',(-4.85068927010169,5.69548202900138,-8.40164026751107));
#21563=CARTESIAN_POINT('Ctrl Pts',(-7.27603390513754,5.87048202900137,-4.20082013374726));
#21564=CARTESIAN_POINT('Ctrl Pts',(-9.70137854017372,6.04548202900137,1.69050809860666E-11));
#21565=CARTESIAN_POINT('Ctrl Pts',(-7.27603390512289,6.22048202900138,4.20082013377262));
#21566=CARTESIAN_POINT('Ctrl Pts',(-4.85068927007193,6.39548202900136,8.40164026752825));
#21567=CARTESIAN_POINT('Ctrl Pts',(1.45949422014197E-11,6.57048202900137,
8.40164026751963));
#21568=CARTESIAN_POINT('Ctrl Pts',(4.8506892701016,6.74548202900138,8.40164026751112));
#21569=CARTESIAN_POINT('Ctrl Pts',(7.27603390513773,6.92048202900139,4.20082013374692));
#21570=CARTESIAN_POINT('Ctrl Pts',(9.70137854017372,7.09548202900137,-1.68004942491202E-11));
#21571=CARTESIAN_POINT('Ctrl Pts',(7.27603390512294,7.27048202900138,-4.20082013377254));
#21572=CARTESIAN_POINT('Ctrl Pts',(4.85068927007202,7.44548202900138,-8.4016402675282));
#21573=CARTESIAN_POINT('Ctrl Pts',(-1.45043674303253E-11,7.62048202900137,
-8.40164026751963));
#21574=CARTESIAN_POINT('Ctrl Pts',(-4.85068927010151,7.79548202900137,-8.40164026751117));
#21575=CARTESIAN_POINT('Ctrl Pts',(-7.27603390513768,7.97048202900139,-4.200820133747));
#21576=CARTESIAN_POINT('Ctrl Pts',(-9.70137854017372,8.14548202900136,1.72473670360602E-11));
#21577=CARTESIAN_POINT('Ctrl Pts',(-7.27603390512298,8.32048202900138,4.20082013377246));
#21578=CARTESIAN_POINT('Ctrl Pts',(-4.85068927007211,8.49548202900138,8.40164026752814));
#21579=CARTESIAN_POINT('Ctrl Pts',(1.48913706160753E-11,8.67048202900136,
8.40164026751963));
#21580=CARTESIAN_POINT('Ctrl Pts',(4.85068927010141,8.84548202900137,8.40164026751122));
#21581=CARTESIAN_POINT('Ctrl Pts',(7.27603390513764,9.02048202900138,4.20082013374708));
#21582=CARTESIAN_POINT('Ctrl Pts',(9.70137854017372,9.19548202900136,-1.71427802991139E-11));
#21583=CARTESIAN_POINT('Ctrl Pts',(7.27603390512303,9.37048202900137,-4.20082013377238));
#21584=CARTESIAN_POINT('Ctrl Pts',(4.8506892700722,9.54548202900137,-8.40164026752809));
#21585=CARTESIAN_POINT('Ctrl Pts',(-1.48007958449808E-11,9.72048202900136,
-8.40164026751963));
#21586=CARTESIAN_POINT('Ctrl Pts',(-4.8506892701018,9.89548202900136,-8.401640267511));
#21587=CARTESIAN_POINT('Ctrl Pts',(-7.27603390513759,10.0704820290014,-4.20082013374716));
#21588=CARTESIAN_POINT('Ctrl Pts',(-9.70137854017372,10.2454820290014,1.70381935621676E-11));
#21589=CARTESIAN_POINT('Ctrl Pts',(-7.27603390512284,10.4204820290014,4.20082013377272));
#21590=CARTESIAN_POINT('Ctrl Pts',(-4.85068927007229,10.5954820290014,8.40164026752804));
#21591=CARTESIAN_POINT('Ctrl Pts',(1.47102210738864E-11,10.7704820290014,
8.40164026751963));
#21592=CARTESIAN_POINT('Ctrl Pts',(4.85068927010171,10.9454820290014,8.40164026751105));
#21593=CARTESIAN_POINT('Ctrl Pts',(7.27603390513755,11.1204820290014,4.20082013374724));
#21594=CARTESIAN_POINT('Ctrl Pts',(9.70137854017372,11.2954820290014,-1.69336068252212E-11));
#21595=CARTESIAN_POINT('Ctrl Pts',(7.27603390512288,11.4704820290014,-4.20082013377264));
#21596=CARTESIAN_POINT('Ctrl Pts',(4.85068927007238,11.6454820290014,-8.40164026752799));
#21597=CARTESIAN_POINT('Ctrl Pts',(-1.46196463027919E-11,11.8204820290014,
-8.40164026751963));
#21598=CARTESIAN_POINT('Ctrl Pts',(-4.85068927010162,11.9954820290014,-8.40164026751111));
#21599=CARTESIAN_POINT('Ctrl Pts',(-7.27603390513774,12.1704820290014,-4.2008201337469));
#21600=CARTESIAN_POINT('Ctrl Pts',(-9.70137854017372,12.3454820290014,1.68290200882749E-11));
#21601=CARTESIAN_POINT('Ctrl Pts',(-7.27603390512293,12.5204820290014,4.20082013377256));
#21602=CARTESIAN_POINT('Ctrl Pts',(-4.85068927007199,12.6954820290014,8.40164026752821));
#21603=CARTESIAN_POINT('Ctrl Pts',(1.45290715316974E-11,12.8704820290014,
8.40164026751963));
#21604=CARTESIAN_POINT('Ctrl Pts',(4.85068927010153,13.0454820290013,8.40164026751116));
#21605=CARTESIAN_POINT('Ctrl Pts',(7.2760339051377,13.2204820290014,4.20082013374698));
#21606=CARTESIAN_POINT('Ctrl Pts',(9.70137854017372,13.3954820290014,-1.67244333513285E-11));
#21607=CARTESIAN_POINT('Ctrl Pts',(7.27603390512297,13.5704820290014,-4.20082013377248));
#21608=CARTESIAN_POINT('Ctrl Pts',(4.85068927007208,13.7454820290014,-8.40164026752816));
#21609=CARTESIAN_POINT('Ctrl Pts',(-1.49160747174474E-11,13.9204820290014,
-8.40164026751963));
#21610=CARTESIAN_POINT('Ctrl Pts',(-4.85068927010144,14.0954820290013,-8.40164026751121));
#21611=CARTESIAN_POINT('Ctrl Pts',(-7.27603390513765,14.2704820290014,-4.20082013374706));
#21612=CARTESIAN_POINT('Ctrl Pts',(-9.70137854017372,14.4454820290014,1.71713061382685E-11));
#21613=CARTESIAN_POINT('Ctrl Pts',(-7.27603390512302,14.6204820290013,4.2008201337724));
#21614=CARTESIAN_POINT('Ctrl Pts',(-4.85068927007218,14.7954820290014,8.40164026752811));
#21615=CARTESIAN_POINT('Ctrl Pts',(1.4825499946353E-11,14.9704820290014,
8.40164026751963));
#21616=CARTESIAN_POINT('Ctrl Pts',(4.85068927010135,15.1454820290013,8.40164026751126));
#21617=CARTESIAN_POINT('Ctrl Pts',(7.27603390513761,15.3204820290014,4.20082013374714));
#21618=CARTESIAN_POINT('Ctrl Pts',(9.70137854017372,15.4954820290014,-1.70667194013222E-11));
#21619=CARTESIAN_POINT('Ctrl Pts',(7.27603390512282,15.6704820290014,-4.20082013377274));
#21620=CARTESIAN_POINT('Ctrl Pts',(4.85068927007227,15.8454820290013,-8.40164026752806));
#21621=CARTESIAN_POINT('Ctrl Pts',(-1.47349251752585E-11,16.0204820290014,
-8.40164026751963));
#21622=CARTESIAN_POINT('Ctrl Pts',(-4.85068927010174,16.1954820290014,-8.40164026751104));
#21623=CARTESIAN_POINT('Ctrl Pts',(-7.27603390513756,16.3704820290014,-4.20082013374722));
#21624=CARTESIAN_POINT('Ctrl Pts',(-9.70137854017372,16.5454820290013,1.69621326643758E-11));
#21625=CARTESIAN_POINT('Ctrl Pts',(-7.27603390512287,16.7204820290014,4.20082013377266));
#21626=CARTESIAN_POINT('Ctrl Pts',(-4.85068927007236,16.8954820290013,8.401640267528));
#21627=CARTESIAN_POINT('Ctrl Pts',(1.46443504041641E-11,17.0704820290014,
8.40164026751963));
#21628=CARTESIAN_POINT('Ctrl Pts',(4.85068927010165,17.2454820290014,8.40164026751109));
#21629=CARTESIAN_POINT('Ctrl Pts',(7.27603390513752,17.4204820290013,4.2008201337473));
#21630=CARTESIAN_POINT('Ctrl Pts',(9.70137854017372,17.5954820290013,-1.68575459274295E-11));
#21631=CARTESIAN_POINT('Ctrl Pts',(7.27603390512292,17.7704820290014,-4.20082013377258));
#21632=CARTESIAN_POINT('Ctrl Pts',(4.85068927007197,17.9454820290013,-8.40164026752823));
#21633=CARTESIAN_POINT('Ctrl Pts',(-1.45537756330696E-11,18.1204820290014,
-8.40164026751963));
#21634=CARTESIAN_POINT('Ctrl Pts',(-4.85068927010155,18.2954820290014,-8.40164026751114));
#21635=CARTESIAN_POINT('Ctrl Pts',(-7.27603390513771,18.4704820290013,-4.20082013374696));
#21636=CARTESIAN_POINT('Ctrl Pts',(-9.70137854017372,18.6454820290013,1.67529591904832E-11));
#21637=CARTESIAN_POINT('Ctrl Pts',(-7.27603390512296,18.8204820290014,4.2008201337725));
#21638=CARTESIAN_POINT('Ctrl Pts',(-4.85068927007206,18.9954820290013,8.40164026752817));
#21639=CARTESIAN_POINT('Ctrl Pts',(1.44632008619752E-11,19.1704820290013,
8.40164026751963));
#21640=CARTESIAN_POINT('Ctrl Pts',(4.85068927010146,19.3454820290013,8.4016402675112));
#21641=CARTESIAN_POINT('Ctrl Pts',(7.27603390513766,19.5204820290013,4.20082013374704));
#21642=CARTESIAN_POINT('Ctrl Pts',(9.70137854017372,19.6954820290013,-1.71998319774232E-11));
#21643=CARTESIAN_POINT('Ctrl Pts',(7.27603390512301,19.8704820290014,-4.20082013377243));
#21644=CARTESIAN_POINT('Ctrl Pts',(4.85068927007215,20.0454820290014,-8.40164026752812));
#21645=CARTESIAN_POINT('Ctrl Pts',(-1.48502040477252E-11,20.2204820290013,
-8.40164026751963));
#21646=CARTESIAN_POINT('Ctrl Pts',(-4.85068927010137,20.3954820290014,-8.40164026751125));
#21647=CARTESIAN_POINT('Ctrl Pts',(-7.27603390513762,20.5704820290014,-4.20082013374712));
#21648=CARTESIAN_POINT('Ctrl Pts',(-9.70137854017372,20.7454820290013,1.70952452404768E-11));
#21649=CARTESIAN_POINT('Ctrl Pts',(-7.27603390512305,20.9204820290013,4.20082013377235));
#21650=CARTESIAN_POINT('Ctrl Pts',(-4.85068927007224,21.0954820290014,8.40164026752807));
#21651=CARTESIAN_POINT('Ctrl Pts',(1.47596292766307E-11,21.2704820290013,
8.40164026751963));
#21652=CARTESIAN_POINT('Ctrl Pts',(4.85068927010176,21.4454820290013,8.40164026751102));
#21653=CARTESIAN_POINT('Ctrl Pts',(7.27603390513757,21.6204820290014,4.2008201337472));
#21654=CARTESIAN_POINT('Ctrl Pts',(9.70137854017372,21.7954820290013,-1.69906585035305E-11));
#21655=CARTESIAN_POINT('Ctrl Pts',(7.27603390512286,21.9704820290013,-4.20082013377268));
#21656=CARTESIAN_POINT('Ctrl Pts',(5.65116042235429,22.0877242779482,-7.015183561788));
#21657=CARTESIAN_POINT('Ctrl Pts',(2.55537495509676,22.22,-8.00360031633711));
#21658=CARTESIAN_POINT('Ctrl Pts',(-1.51301075899711E-11,-144.093984254242,
-8.40164026751963));
#21659=CARTESIAN_POINT('Ctrl Pts',(-4.85068927010199,-143.918984254242,
-8.4016402675109));
#21660=CARTESIAN_POINT('Ctrl Pts',(-7.27603390513785,-143.743984254242,
-4.20082013374671));
#21661=CARTESIAN_POINT('Ctrl Pts',(-9.70137854017372,-143.568984254242,
1.74701493417668E-11));
#21662=CARTESIAN_POINT('Ctrl Pts',(-7.27603390512272,-143.393984254242,
4.20082013377292));
#21663=CARTESIAN_POINT('Ctrl Pts',(-4.85068927007173,-143.218984254242,
8.40164026752836));
#21664=CARTESIAN_POINT('Ctrl Pts',(1.5129078685785E-11,-143.043984254242,
8.40164026751963));
#21665=CARTESIAN_POINT('Ctrl Pts',(4.85068927010198,-142.868984254242,8.4016402675109));
#21666=CARTESIAN_POINT('Ctrl Pts',(7.27603390513785,-142.693984254242,4.20082013374672));
#21667=CARTESIAN_POINT('Ctrl Pts',(9.70137854017372,-142.518984254242,-1.74689612655491E-11));
#21668=CARTESIAN_POINT('Ctrl Pts',(7.27603390512273,-142.343984254242,-4.20082013377291));
#21669=CARTESIAN_POINT('Ctrl Pts',(4.85068927007173,-142.168984254242,-8.40164026752836));
#21670=CARTESIAN_POINT('Ctrl Pts',(-1.51301075899711E-11,-141.993984254242,
-8.40164026751963));
#21671=CARTESIAN_POINT('Ctrl Pts',(-4.85068927010199,-141.818984254242,
-8.4016402675109));
#21672=CARTESIAN_POINT('Ctrl Pts',(-7.27603390513785,-141.643984254242,
-4.20082013374671));
#21673=CARTESIAN_POINT('Ctrl Pts',(-9.70137854017372,-141.468984254242,
1.74701493417668E-11));
#21674=CARTESIAN_POINT('Ctrl Pts',(-7.27603390512272,-141.293984254242,
4.20082013377292));
#21675=CARTESIAN_POINT('Ctrl Pts',(-4.85068927007173,-141.118984254242,
8.40164026752836));
#21676=CARTESIAN_POINT('Ctrl Pts',(1.5129078685785E-11,-140.943984254242,
8.40164026751963));
#21677=CARTESIAN_POINT('Ctrl Pts',(4.85068927010198,-140.768984254242,8.4016402675109));
#21678=CARTESIAN_POINT('Ctrl Pts',(7.27603390513785,-140.593984254242,4.20082013374672));
#21679=CARTESIAN_POINT('Ctrl Pts',(9.70137854017372,-140.418984254242,-1.74689612655491E-11));
#21680=CARTESIAN_POINT('Ctrl Pts',(7.27603390512273,-140.243984254242,-4.20082013377291));
#21681=CARTESIAN_POINT('Ctrl Pts',(4.85068927007173,-140.068984254242,-8.40164026752836));
#21682=CARTESIAN_POINT('Ctrl Pts',(-1.51301075899711E-11,-139.893984254242,
-8.40164026751963));
#21683=CARTESIAN_POINT('Ctrl Pts',(-4.85068927010199,-139.718984254242,
-8.4016402675109));
#21684=CARTESIAN_POINT('Ctrl Pts',(-7.27603390513785,-139.543984254242,
-4.20082013374671));
#21685=CARTESIAN_POINT('Ctrl Pts',(-9.70137854017372,-139.368984254242,
1.74701493417668E-11));
#21686=CARTESIAN_POINT('Ctrl Pts',(-7.27603390512272,-139.193984254242,
4.20082013377292));
#21687=CARTESIAN_POINT('Ctrl Pts',(-4.85068927007173,-139.018984254242,
8.40164026752836));
#21688=CARTESIAN_POINT('Ctrl Pts',(1.5129078685785E-11,-138.843984254242,
8.40164026751963));
#21689=CARTESIAN_POINT('Ctrl Pts',(4.85068927010198,-138.668984254242,8.4016402675109));
#21690=CARTESIAN_POINT('Ctrl Pts',(7.27603390513785,-138.493984254242,4.20082013374672));
#21691=CARTESIAN_POINT('Ctrl Pts',(9.70137854017372,-138.318984254242,-1.74689612655491E-11));
#21692=CARTESIAN_POINT('Ctrl Pts',(7.27603390512273,-138.143984254242,-4.20082013377291));
#21693=CARTESIAN_POINT('Ctrl Pts',(4.85068927007173,-137.968984254242,-8.40164026752836));
#21694=CARTESIAN_POINT('Ctrl Pts',(-1.51301075899711E-11,-137.793984254242,
-8.40164026751963));
#21695=CARTESIAN_POINT('Ctrl Pts',(-4.85068927010199,-137.618984254242,
-8.4016402675109));
#21696=CARTESIAN_POINT('Ctrl Pts',(-7.27603390513785,-137.443984254242,
-4.20082013374671));
#21697=CARTESIAN_POINT('Ctrl Pts',(-9.70137854017372,-137.268984254242,
1.74701493417668E-11));
#21698=CARTESIAN_POINT('Ctrl Pts',(-7.27603390512272,-137.093984254242,
4.20082013377292));
#21699=CARTESIAN_POINT('Ctrl Pts',(-4.85068927007173,-136.918984254242,
8.40164026752836));
#21700=CARTESIAN_POINT('Ctrl Pts',(1.5129078685785E-11,-136.743984254242,
8.40164026751963));
#21701=CARTESIAN_POINT('Ctrl Pts',(4.85068927010198,-136.568984254242,8.4016402675109));
#21702=CARTESIAN_POINT('Ctrl Pts',(7.27603390513785,-136.393984254242,4.20082013374672));
#21703=CARTESIAN_POINT('Ctrl Pts',(9.70137854017372,-136.218984254242,-1.74689612655491E-11));
#21704=CARTESIAN_POINT('Ctrl Pts',(7.27603390512273,-136.043984254242,-4.20082013377291));
#21705=CARTESIAN_POINT('Ctrl Pts',(4.85068927007173,-135.868984254242,-8.40164026752836));
#21706=CARTESIAN_POINT('Ctrl Pts',(-1.51301075899711E-11,-135.693984254242,
-8.40164026751963));
#21707=CARTESIAN_POINT('Ctrl Pts',(-4.85068927010199,-135.518984254242,
-8.4016402675109));
#21708=CARTESIAN_POINT('Ctrl Pts',(-7.27603390513785,-135.343984254242,
-4.20082013374671));
#21709=CARTESIAN_POINT('Ctrl Pts',(-9.70137854017372,-135.168984254242,
1.74701493417668E-11));
#21710=CARTESIAN_POINT('Ctrl Pts',(-7.27603390512272,-134.993984254242,
4.20082013377292));
#21711=CARTESIAN_POINT('Ctrl Pts',(-4.85068927007173,-134.818984254242,
8.40164026752836));
#21712=CARTESIAN_POINT('Ctrl Pts',(1.5129078685785E-11,-134.643984254242,
8.40164026751963));
#21713=CARTESIAN_POINT('Ctrl Pts',(4.85068927010198,-134.468984254242,8.4016402675109));
#21714=CARTESIAN_POINT('Ctrl Pts',(7.27603390513785,-134.293984254242,4.20082013374672));
#21715=CARTESIAN_POINT('Ctrl Pts',(9.70137854017372,-134.118984254242,-1.74689612655491E-11));
#21716=CARTESIAN_POINT('Ctrl Pts',(7.27603390512273,-133.943984254242,-4.20082013377291));
#21717=CARTESIAN_POINT('Ctrl Pts',(4.85068927007173,-133.768984254242,-8.40164026752836));
#21718=CARTESIAN_POINT('Ctrl Pts',(-1.51301075899711E-11,-133.593984254242,
-8.40164026751963));
#21719=CARTESIAN_POINT('Ctrl Pts',(-4.85068927010199,-133.418984254242,
-8.4016402675109));
#21720=CARTESIAN_POINT('Ctrl Pts',(-7.27603390513785,-133.243984254242,
-4.20082013374671));
#21721=CARTESIAN_POINT('Ctrl Pts',(-9.70137854017372,-133.068984254242,
1.74701493417668E-11));
#21722=CARTESIAN_POINT('Ctrl Pts',(-7.27603390512272,-132.893984254242,
4.20082013377292));
#21723=CARTESIAN_POINT('Ctrl Pts',(-4.85068927007173,-132.718984254242,
8.40164026752836));
#21724=CARTESIAN_POINT('Ctrl Pts',(1.5129078685785E-11,-132.543984254242,
8.40164026751963));
#21725=CARTESIAN_POINT('Ctrl Pts',(4.85068927010198,-132.368984254242,8.4016402675109));
#21726=CARTESIAN_POINT('Ctrl Pts',(7.27603390513785,-132.193984254242,4.20082013374672));
#21727=CARTESIAN_POINT('Ctrl Pts',(9.70137854017372,-132.018984254242,-1.74689612655491E-11));
#21728=CARTESIAN_POINT('Ctrl Pts',(7.27603390512273,-131.843984254242,-4.20082013377291));
#21729=CARTESIAN_POINT('Ctrl Pts',(4.85068927007173,-131.668984254242,-8.40164026752836));
#21730=CARTESIAN_POINT('Ctrl Pts',(-1.51301075899711E-11,-131.493984254242,
-8.40164026751963));
#21731=CARTESIAN_POINT('Ctrl Pts',(-4.85068927010199,-131.318984254242,
-8.4016402675109));
#21732=CARTESIAN_POINT('Ctrl Pts',(-7.27603390513785,-131.143984254242,
-4.20082013374671));
#21733=CARTESIAN_POINT('Ctrl Pts',(-9.70137854017372,-130.968984254242,
1.74701493417668E-11));
#21734=CARTESIAN_POINT('Ctrl Pts',(-7.27603390512272,-130.793984254242,
4.20082013377292));
#21735=CARTESIAN_POINT('Ctrl Pts',(-4.85068927007173,-130.618984254242,
8.40164026752836));
#21736=CARTESIAN_POINT('Ctrl Pts',(1.5129078685785E-11,-130.443984254242,
8.40164026751963));
#21737=CARTESIAN_POINT('Ctrl Pts',(4.85068927010198,-130.268984254242,8.4016402675109));
#21738=CARTESIAN_POINT('Ctrl Pts',(7.27603390513785,-130.093984254242,4.20082013374672));
#21739=CARTESIAN_POINT('Ctrl Pts',(9.70137854017372,-129.918984254242,-1.74689612655491E-11));
#21740=CARTESIAN_POINT('Ctrl Pts',(7.27603390512273,-129.743984254242,-4.20082013377291));
#21741=CARTESIAN_POINT('Ctrl Pts',(4.85068927007173,-129.568984254242,-8.40164026752836));
#21742=CARTESIAN_POINT('Ctrl Pts',(-1.51301075899711E-11,-129.393984254242,
-8.40164026751963));
#21743=CARTESIAN_POINT('Ctrl Pts',(-4.85068927010199,-129.218984254242,
-8.4016402675109));
#21744=CARTESIAN_POINT('Ctrl Pts',(-7.27603390513785,-129.043984254242,
-4.20082013374671));
#21745=CARTESIAN_POINT('Ctrl Pts',(-9.70137854017372,-128.868984254242,
1.74701493417668E-11));
#21746=CARTESIAN_POINT('Ctrl Pts',(-7.27603390512272,-128.693984254242,
4.20082013377292));
#21747=CARTESIAN_POINT('Ctrl Pts',(-4.85068927007173,-128.518984254242,
8.40164026752836));
#21748=CARTESIAN_POINT('Ctrl Pts',(1.5129078685785E-11,-128.343984254242,
8.40164026751963));
#21749=CARTESIAN_POINT('Ctrl Pts',(4.85068927010198,-128.168984254242,8.4016402675109));
#21750=CARTESIAN_POINT('Ctrl Pts',(7.27603390513785,-127.993984254242,4.20082013374672));
#21751=CARTESIAN_POINT('Ctrl Pts',(9.70137854017372,-127.818984254242,-1.74689612655491E-11));
#21752=CARTESIAN_POINT('Ctrl Pts',(7.27603390512273,-127.643984254242,-4.20082013377291));
#21753=CARTESIAN_POINT('Ctrl Pts',(4.85068927007173,-127.468984254242,-8.40164026752836));
#21754=CARTESIAN_POINT('Ctrl Pts',(-1.51301075899711E-11,-127.293984254242,
-8.40164026751963));
#21755=CARTESIAN_POINT('Ctrl Pts',(-4.85068927010199,-127.118984254242,
-8.4016402675109));
#21756=CARTESIAN_POINT('Ctrl Pts',(-7.27603390513785,-126.943984254242,
-4.20082013374671));
#21757=CARTESIAN_POINT('Ctrl Pts',(-9.70137854017372,-126.768984254242,
1.74701493417668E-11));
#21758=CARTESIAN_POINT('Ctrl Pts',(-7.27603390512272,-126.593984254242,
4.20082013377292));
#21759=CARTESIAN_POINT('Ctrl Pts',(-4.85068927007173,-126.418984254242,
8.40164026752836));
#21760=CARTESIAN_POINT('Ctrl Pts',(1.5129078685785E-11,-126.243984254242,
8.40164026751963));
#21761=CARTESIAN_POINT('Ctrl Pts',(4.85068927010198,-126.068984254242,8.4016402675109));
#21762=CARTESIAN_POINT('Ctrl Pts',(7.27603390513785,-125.893984254242,4.20082013374672));
#21763=CARTESIAN_POINT('Ctrl Pts',(9.70137854017372,-125.718984254242,-1.74689612655491E-11));
#21764=CARTESIAN_POINT('Ctrl Pts',(7.27603390512273,-125.543984254242,-4.20082013377291));
#21765=CARTESIAN_POINT('Ctrl Pts',(4.85068927007173,-125.368984254242,-8.40164026752836));
#21766=CARTESIAN_POINT('Ctrl Pts',(-1.51301075899711E-11,-125.193984254242,
-8.40164026751963));
#21767=CARTESIAN_POINT('Ctrl Pts',(-4.85068927010199,-125.018984254242,
-8.4016402675109));
#21768=CARTESIAN_POINT('Ctrl Pts',(-7.27603390513785,-124.843984254242,
-4.20082013374671));
#21769=CARTESIAN_POINT('Ctrl Pts',(-9.70137854017372,-124.668984254242,
1.74701493417668E-11));
#21770=CARTESIAN_POINT('Ctrl Pts',(-7.27603390512272,-124.493984254242,
4.20082013377292));
#21771=CARTESIAN_POINT('Ctrl Pts',(-4.85068927007173,-124.318984254242,
8.40164026752836));
#21772=CARTESIAN_POINT('Ctrl Pts',(1.5129078685785E-11,-124.143984254242,
8.40164026751963));
#21773=CARTESIAN_POINT('Ctrl Pts',(4.85068927010198,-123.968984254242,8.4016402675109));
#21774=CARTESIAN_POINT('Ctrl Pts',(7.27603390513785,-123.793984254242,4.20082013374672));
#21775=CARTESIAN_POINT('Ctrl Pts',(9.70137854017372,-123.618984254242,-1.74689612655491E-11));
#21776=CARTESIAN_POINT('Ctrl Pts',(7.27603390512273,-123.443984254242,-4.20082013377291));
#21777=CARTESIAN_POINT('Ctrl Pts',(4.85068927007173,-123.268984254242,-8.40164026752836));
#21778=CARTESIAN_POINT('Ctrl Pts',(-1.51301075899711E-11,-123.093984254242,
-8.40164026751963));
#21779=CARTESIAN_POINT('Ctrl Pts',(-4.85068927010199,-122.918984254242,
-8.4016402675109));
#21780=CARTESIAN_POINT('Ctrl Pts',(-7.27603390513785,-122.743984254242,
-4.20082013374671));
#21781=CARTESIAN_POINT('Ctrl Pts',(-9.70137854017372,-122.568984254242,
1.74701493417668E-11));
#21782=CARTESIAN_POINT('Ctrl Pts',(-7.27603390512272,-122.393984254242,
4.20082013377292));
#21783=CARTESIAN_POINT('Ctrl Pts',(-4.85068927007173,-122.218984254242,
8.40164026752836));
#21784=CARTESIAN_POINT('Ctrl Pts',(1.5129078685785E-11,-122.043984254242,
8.40164026751963));
#21785=CARTESIAN_POINT('Ctrl Pts',(4.85068927010198,-121.868984254242,8.4016402675109));
#21786=CARTESIAN_POINT('Ctrl Pts',(7.27603390513785,-121.693984254242,4.20082013374672));
#21787=CARTESIAN_POINT('Ctrl Pts',(9.70137854017372,-121.518984254242,-1.74689612655491E-11));
#21788=CARTESIAN_POINT('Ctrl Pts',(7.27603390512273,-121.343984254242,-4.20082013377291));
#21789=CARTESIAN_POINT('Ctrl Pts',(4.85068927007173,-121.168984254242,-8.40164026752836));
#21790=CARTESIAN_POINT('Ctrl Pts',(-1.51301075899711E-11,-120.993984254242,
-8.40164026751963));
#21791=CARTESIAN_POINT('Ctrl Pts',(-4.85068927010199,-120.818984254242,
-8.4016402675109));
#21792=CARTESIAN_POINT('Ctrl Pts',(-7.27603390513785,-120.643984254242,
-4.20082013374671));
#21793=CARTESIAN_POINT('Ctrl Pts',(-9.70137854017372,-120.468984254242,
1.74701493417668E-11));
#21794=CARTESIAN_POINT('Ctrl Pts',(-7.27603390512272,-120.293984254242,
4.20082013377292));
#21795=CARTESIAN_POINT('Ctrl Pts',(-4.85068927007173,-120.118984254242,
8.40164026752836));
#21796=CARTESIAN_POINT('Ctrl Pts',(1.5129078685785E-11,-119.943984254242,
8.40164026751963));
#21797=CARTESIAN_POINT('Ctrl Pts',(4.85068927010198,-119.768984254242,8.4016402675109));
#21798=CARTESIAN_POINT('Ctrl Pts',(7.27603390513785,-119.593984254242,4.20082013374672));
#21799=CARTESIAN_POINT('Ctrl Pts',(9.70137854017372,-119.418984254242,-1.74689612655491E-11));
#21800=CARTESIAN_POINT('Ctrl Pts',(7.27603390512273,-119.243984254242,-4.20082013377291));
#21801=CARTESIAN_POINT('Ctrl Pts',(4.85068927007173,-119.068984254242,-8.40164026752836));
#21802=CARTESIAN_POINT('Ctrl Pts',(-1.51301075899711E-11,-118.893984254242,
-8.40164026751963));
#21803=CARTESIAN_POINT('Ctrl Pts',(-4.85068927010199,-118.718984254242,
-8.4016402675109));
#21804=CARTESIAN_POINT('Ctrl Pts',(-7.27603390513785,-118.543984254242,
-4.20082013374671));
#21805=CARTESIAN_POINT('Ctrl Pts',(-9.70137854017372,-118.368984254242,
1.74701493417668E-11));
#21806=CARTESIAN_POINT('Ctrl Pts',(-7.27603390512272,-118.193984254242,
4.20082013377292));
#21807=CARTESIAN_POINT('Ctrl Pts',(-4.85068927007173,-118.018984254242,
8.40164026752836));
#21808=CARTESIAN_POINT('Ctrl Pts',(1.5129078685785E-11,-117.843984254242,
8.40164026751963));
#21809=CARTESIAN_POINT('Ctrl Pts',(4.85068927010198,-117.668984254242,8.4016402675109));
#21810=CARTESIAN_POINT('Ctrl Pts',(7.27603390513785,-117.493984254242,4.20082013374672));
#21811=CARTESIAN_POINT('Ctrl Pts',(9.70137854017372,-117.318984254242,-1.74689612655491E-11));
#21812=CARTESIAN_POINT('Ctrl Pts',(7.27603390512273,-117.143984254242,-4.20082013377291));
#21813=CARTESIAN_POINT('Ctrl Pts',(4.85068927007173,-116.968984254242,-8.40164026752836));
#21814=CARTESIAN_POINT('Ctrl Pts',(-1.51301075899711E-11,-116.793984254242,
-8.40164026751963));
#21815=CARTESIAN_POINT('Ctrl Pts',(-4.85068927010199,-116.618984254242,
-8.4016402675109));
#21816=CARTESIAN_POINT('Ctrl Pts',(-7.27603390513785,-116.443984254242,
-4.20082013374671));
#21817=CARTESIAN_POINT('Ctrl Pts',(-9.70137854017372,-116.268984254242,
1.74701493417668E-11));
#21818=CARTESIAN_POINT('Ctrl Pts',(-7.27603390512272,-116.093984254242,
4.20082013377292));
#21819=CARTESIAN_POINT('Ctrl Pts',(-4.85068927007173,-115.918984254242,
8.40164026752836));
#21820=CARTESIAN_POINT('Ctrl Pts',(1.5129078685785E-11,-115.743984254242,
8.40164026751963));
#21821=CARTESIAN_POINT('Ctrl Pts',(4.85068927010198,-115.568984254242,8.4016402675109));
#21822=CARTESIAN_POINT('Ctrl Pts',(7.27603390513785,-115.393984254242,4.20082013374672));
#21823=CARTESIAN_POINT('Ctrl Pts',(9.70137854017372,-115.218984254242,-1.74689612655491E-11));
#21824=CARTESIAN_POINT('Ctrl Pts',(7.27603390512273,-115.043984254242,-4.20082013377291));
#21825=CARTESIAN_POINT('Ctrl Pts',(4.85068927007173,-114.868984254242,-8.40164026752836));
#21826=CARTESIAN_POINT('Ctrl Pts',(-1.51301075899711E-11,-114.693984254242,
-8.40164026751963));
#21827=CARTESIAN_POINT('Ctrl Pts',(-4.85068927010199,-114.518984254242,
-8.4016402675109));
#21828=CARTESIAN_POINT('Ctrl Pts',(-7.27603390513785,-114.343984254242,
-4.20082013374671));
#21829=CARTESIAN_POINT('Ctrl Pts',(-9.70137854017372,-114.168984254242,
1.74701493417668E-11));
#21830=CARTESIAN_POINT('Ctrl Pts',(-7.27603390512272,-113.993984254242,
4.20082013377292));
#21831=CARTESIAN_POINT('Ctrl Pts',(-4.85068927007173,-113.818984254242,
8.40164026752836));
#21832=CARTESIAN_POINT('Ctrl Pts',(1.5129078685785E-11,-113.643984254242,
8.40164026751963));
#21833=CARTESIAN_POINT('Ctrl Pts',(4.85068927010198,-113.468984254242,8.4016402675109));
#21834=CARTESIAN_POINT('Ctrl Pts',(7.27603390513785,-113.293984254242,4.20082013374672));
#21835=CARTESIAN_POINT('Ctrl Pts',(9.70137854017372,-113.118984254242,-1.74689612655491E-11));
#21836=CARTESIAN_POINT('Ctrl Pts',(7.27603390512273,-112.943984254242,-4.20082013377291));
#21837=CARTESIAN_POINT('Ctrl Pts',(4.85068927007173,-112.768984254242,-8.40164026752836));
#21838=CARTESIAN_POINT('Ctrl Pts',(-1.51301075899711E-11,-112.593984254242,
-8.40164026751963));
#21839=CARTESIAN_POINT('Ctrl Pts',(-4.85068927010199,-112.418984254242,
-8.4016402675109));
#21840=CARTESIAN_POINT('Ctrl Pts',(-7.27603390513785,-112.243984254242,
-4.20082013374671));
#21841=CARTESIAN_POINT('Ctrl Pts',(-9.70137854017372,-112.068984254242,
1.74701493417668E-11));
#21842=CARTESIAN_POINT('Ctrl Pts',(-7.27603390512272,-111.893984254242,
4.20082013377292));
#21843=CARTESIAN_POINT('Ctrl Pts',(-4.85068927007173,-111.718984254242,
8.40164026752836));
#21844=CARTESIAN_POINT('Ctrl Pts',(1.5129078685785E-11,-111.543984254242,
8.40164026751963));
#21845=CARTESIAN_POINT('Ctrl Pts',(4.85068927010198,-111.368984254242,8.4016402675109));
#21846=CARTESIAN_POINT('Ctrl Pts',(7.27603390513785,-111.193984254242,4.20082013374672));
#21847=CARTESIAN_POINT('Ctrl Pts',(9.70137854017372,-111.018984254242,-1.74689612655491E-11));
#21848=CARTESIAN_POINT('Ctrl Pts',(7.27603390512273,-110.843984254242,-4.20082013377291));
#21849=CARTESIAN_POINT('Ctrl Pts',(4.85068927007173,-110.668984254242,-8.40164026752836));
#21850=CARTESIAN_POINT('Ctrl Pts',(-1.51301075899711E-11,-110.493984254242,
-8.40164026751963));
#21851=CARTESIAN_POINT('Ctrl Pts',(-4.85068927010199,-110.318984254242,
-8.4016402675109));
#21852=CARTESIAN_POINT('Ctrl Pts',(-7.27603390513785,-110.143984254242,
-4.20082013374671));
#21853=CARTESIAN_POINT('Ctrl Pts',(-9.70137854017372,-109.968984254242,
1.74701493417668E-11));
#21854=CARTESIAN_POINT('Ctrl Pts',(-7.27603390512272,-109.793984254242,
4.20082013377292));
#21855=CARTESIAN_POINT('Ctrl Pts',(-4.85068927007173,-109.618984254242,
8.40164026752836));
#21856=CARTESIAN_POINT('Ctrl Pts',(1.5129078685785E-11,-109.443984254242,
8.40164026751963));
#21857=CARTESIAN_POINT('Ctrl Pts',(4.85068927010198,-109.268984254242,8.4016402675109));
#21858=CARTESIAN_POINT('Ctrl Pts',(7.27603390513785,-109.093984254242,4.20082013374672));
#21859=CARTESIAN_POINT('Ctrl Pts',(9.70137854017372,-108.918984254242,-1.74689612655491E-11));
#21860=CARTESIAN_POINT('Ctrl Pts',(7.27603390512273,-108.743984254242,-4.20082013377291));
#21861=CARTESIAN_POINT('Ctrl Pts',(4.85068927007173,-108.568984254242,-8.40164026752836));
#21862=CARTESIAN_POINT('Ctrl Pts',(-1.51301075899711E-11,-108.393984254242,
-8.40164026751963));
#21863=CARTESIAN_POINT('Ctrl Pts',(-4.85068927010199,-108.218984254242,
-8.4016402675109));
#21864=CARTESIAN_POINT('Ctrl Pts',(-7.27603390513785,-108.043984254242,
-4.20082013374671));
#21865=CARTESIAN_POINT('Ctrl Pts',(-9.70137854017372,-107.868984254242,
1.74701493417668E-11));
#21866=CARTESIAN_POINT('Ctrl Pts',(-7.27603390512272,-107.693984254242,
4.20082013377292));
#21867=CARTESIAN_POINT('Ctrl Pts',(-4.85068927007173,-107.518984254242,
8.40164026752836));
#21868=CARTESIAN_POINT('Ctrl Pts',(1.5129078685785E-11,-107.343984254242,
8.40164026751963));
#21869=CARTESIAN_POINT('Ctrl Pts',(4.85068927010198,-107.168984254242,8.4016402675109));
#21870=CARTESIAN_POINT('Ctrl Pts',(7.27603390513785,-106.993984254242,4.20082013374672));
#21871=CARTESIAN_POINT('Ctrl Pts',(9.70137854017372,-106.818984254242,-1.74689612655491E-11));
#21872=CARTESIAN_POINT('Ctrl Pts',(7.27603390512273,-106.643984254242,-4.20082013377291));
#21873=CARTESIAN_POINT('Ctrl Pts',(4.85068927007173,-106.468984254242,-8.40164026752836));
#21874=CARTESIAN_POINT('Ctrl Pts',(-1.51301075899711E-11,-106.293984254242,
-8.40164026751963));
#21875=CARTESIAN_POINT('Ctrl Pts',(-4.85068927010199,-106.118984254242,
-8.4016402675109));
#21876=CARTESIAN_POINT('Ctrl Pts',(-7.27603390513785,-105.943984254242,
-4.20082013374671));
#21877=CARTESIAN_POINT('Ctrl Pts',(-9.70137854017372,-105.768984254242,
1.74701493417668E-11));
#21878=CARTESIAN_POINT('Ctrl Pts',(-7.27603390512272,-105.593984254242,
4.20082013377292));
#21879=CARTESIAN_POINT('Ctrl Pts',(-4.85068927007173,-105.418984254242,
8.40164026752836));
#21880=CARTESIAN_POINT('Ctrl Pts',(1.5129078685785E-11,-105.243984254242,
8.40164026751963));
#21881=CARTESIAN_POINT('Ctrl Pts',(4.85068927010198,-105.068984254242,8.4016402675109));
#21882=CARTESIAN_POINT('Ctrl Pts',(7.27603390513785,-104.893984254242,4.20082013374672));
#21883=CARTESIAN_POINT('Ctrl Pts',(9.70137854017372,-104.718984254242,-1.74689612655491E-11));
#21884=CARTESIAN_POINT('Ctrl Pts',(7.27603390512273,-104.543984254242,-4.20082013377291));
#21885=CARTESIAN_POINT('Ctrl Pts',(4.85068927007173,-104.368984254242,-8.40164026752836));
#21886=CARTESIAN_POINT('Ctrl Pts',(-1.51301075899711E-11,-104.193984254242,
-8.40164026751963));
#21887=CARTESIAN_POINT('Ctrl Pts',(-4.85068927010199,-104.018984254242,
-8.4016402675109));
#21888=CARTESIAN_POINT('Ctrl Pts',(-7.27603390513785,-103.843984254242,
-4.20082013374671));
#21889=CARTESIAN_POINT('Ctrl Pts',(-9.70137854017372,-103.668984254242,
1.74701493417668E-11));
#21890=CARTESIAN_POINT('Ctrl Pts',(-7.27603390512272,-103.493984254242,
4.20082013377292));
#21891=CARTESIAN_POINT('Ctrl Pts',(-4.85068927007173,-103.318984254242,
8.40164026752836));
#21892=CARTESIAN_POINT('Ctrl Pts',(1.5129078685785E-11,-103.143984254242,
8.40164026751963));
#21893=CARTESIAN_POINT('Ctrl Pts',(4.85068927010198,-102.968984254242,8.4016402675109));
#21894=CARTESIAN_POINT('Ctrl Pts',(7.27603390513785,-102.793984254242,4.20082013374672));
#21895=CARTESIAN_POINT('Ctrl Pts',(9.70137854017372,-102.618984254242,-1.74689612655491E-11));
#21896=CARTESIAN_POINT('Ctrl Pts',(7.27603390512273,-102.443984254242,-4.20082013377291));
#21897=CARTESIAN_POINT('Ctrl Pts',(4.85068927007173,-102.268984254242,-8.40164026752836));
#21898=CARTESIAN_POINT('Ctrl Pts',(-1.51301075899711E-11,-102.093984254242,
-8.40164026751963));
#21899=CARTESIAN_POINT('Ctrl Pts',(-4.85068927010199,-101.918984254242,
-8.4016402675109));
#21900=CARTESIAN_POINT('Ctrl Pts',(-7.27603390513785,-101.743984254242,
-4.20082013374671));
#21901=CARTESIAN_POINT('Ctrl Pts',(-9.70137854017372,-101.568984254242,
1.74701493417668E-11));
#21902=CARTESIAN_POINT('Ctrl Pts',(-7.27603390512272,-101.393984254242,
4.20082013377292));
#21903=CARTESIAN_POINT('Ctrl Pts',(-4.85068927007173,-101.218984254242,
8.40164026752836));
#21904=CARTESIAN_POINT('Ctrl Pts',(1.5129078685785E-11,-101.043984254242,
8.40164026751963));
#21905=CARTESIAN_POINT('Ctrl Pts',(4.85068927010198,-100.868984254242,8.4016402675109));
#21906=CARTESIAN_POINT('Ctrl Pts',(7.27603390513785,-100.693984254242,4.20082013374672));
#21907=CARTESIAN_POINT('Ctrl Pts',(9.70137854017372,-100.518984254242,-1.74689612655491E-11));
#21908=CARTESIAN_POINT('Ctrl Pts',(7.27603390512273,-100.343984254242,-4.20082013377291));
#21909=CARTESIAN_POINT('Ctrl Pts',(4.85068927007173,-100.168984254242,-8.40164026752836));
#21910=CARTESIAN_POINT('Ctrl Pts',(-1.51301075899711E-11,-99.9939842542418,
-8.40164026751963));
#21911=CARTESIAN_POINT('Ctrl Pts',(-4.85068927010199,-99.8189842542418,
-8.4016402675109));
#21912=CARTESIAN_POINT('Ctrl Pts',(-7.27603390513785,-99.6439842542417,
-4.20082013374671));
#21913=CARTESIAN_POINT('Ctrl Pts',(-9.70137854017372,-99.4689842542418,
1.74701493417668E-11));
#21914=CARTESIAN_POINT('Ctrl Pts',(-7.27603390512272,-99.2939842542417,
4.20082013377292));
#21915=CARTESIAN_POINT('Ctrl Pts',(-4.85068927007173,-99.1189842542418,
8.40164026752836));
#21916=CARTESIAN_POINT('Ctrl Pts',(1.5129078685785E-11,-98.9439842542418,
8.40164026751963));
#21917=CARTESIAN_POINT('Ctrl Pts',(4.85068927010198,-98.7689842542417,8.4016402675109));
#21918=CARTESIAN_POINT('Ctrl Pts',(7.27603390513785,-98.5939842542417,4.20082013374672));
#21919=CARTESIAN_POINT('Ctrl Pts',(9.70137854017372,-98.4189842542418,-1.74689612655491E-11));
#21920=CARTESIAN_POINT('Ctrl Pts',(7.27603390512273,-98.2439842542418,-4.20082013377291));
#21921=CARTESIAN_POINT('Ctrl Pts',(4.85068927007173,-98.0689842542417,-8.40164026752836));
#21922=CARTESIAN_POINT('Ctrl Pts',(-1.51301075899711E-11,-97.8939842542418,
-8.40164026751963));
#21923=CARTESIAN_POINT('Ctrl Pts',(-4.85068927010199,-97.7189842542418,
-8.4016402675109));
#21924=CARTESIAN_POINT('Ctrl Pts',(-7.27603390513785,-97.5439842542417,
-4.20082013374671));
#21925=CARTESIAN_POINT('Ctrl Pts',(-9.70137854017372,-97.3689842542418,
1.74701493417668E-11));
#21926=CARTESIAN_POINT('Ctrl Pts',(-7.27603390512272,-97.1939842542418,
4.20082013377292));
#21927=CARTESIAN_POINT('Ctrl Pts',(-4.85068927007173,-97.0189842542418,
8.40164026752836));
#21928=CARTESIAN_POINT('Ctrl Pts',(1.5129078685785E-11,-96.8439842542418,
8.40164026751963));
#21929=CARTESIAN_POINT('Ctrl Pts',(4.85068927010198,-96.6689842542418,8.4016402675109));
#21930=CARTESIAN_POINT('Ctrl Pts',(7.27603390513785,-96.4939842542417,4.20082013374672));
#21931=CARTESIAN_POINT('Ctrl Pts',(9.70137854017372,-96.3189842542418,-1.74689612655491E-11));
#21932=CARTESIAN_POINT('Ctrl Pts',(7.27603390512273,-96.1439842542418,-4.20082013377291));
#21933=CARTESIAN_POINT('Ctrl Pts',(4.85068927007173,-95.9689842542417,-8.40164026752836));
#21934=CARTESIAN_POINT('Ctrl Pts',(-1.51301075899711E-11,-95.7939842542418,
-8.40164026751963));
#21935=CARTESIAN_POINT('Ctrl Pts',(-4.85068927010199,-95.6189842542418,
-8.4016402675109));
#21936=CARTESIAN_POINT('Ctrl Pts',(-7.27603390513785,-95.4439842542418,
-4.20082013374671));
#21937=CARTESIAN_POINT('Ctrl Pts',(-9.70137854017372,-95.2689842542418,
1.74701493417668E-11));
#21938=CARTESIAN_POINT('Ctrl Pts',(-7.27603390512272,-95.0939842542418,
4.20082013377292));
#21939=CARTESIAN_POINT('Ctrl Pts',(-4.85068927007173,-94.9189842542418,
8.40164026752836));
#21940=CARTESIAN_POINT('Ctrl Pts',(1.5129078685785E-11,-94.7439842542418,
8.40164026751963));
#21941=CARTESIAN_POINT('Ctrl Pts',(4.85068927010198,-94.5689842542417,8.4016402675109));
#21942=CARTESIAN_POINT('Ctrl Pts',(7.27603390513785,-94.3939842542418,4.20082013374672));
#21943=CARTESIAN_POINT('Ctrl Pts',(9.70137854017372,-94.2189842542417,-1.74689612655491E-11));
#21944=CARTESIAN_POINT('Ctrl Pts',(7.27603390512273,-94.0439842542417,-4.20082013377291));
#21945=CARTESIAN_POINT('Ctrl Pts',(4.85068927007173,-93.8689842542418,-8.40164026752836));
#21946=CARTESIAN_POINT('Ctrl Pts',(-1.51301075899711E-11,-93.6939842542417,
-8.40164026751963));
#21947=CARTESIAN_POINT('Ctrl Pts',(-4.85068927010199,-93.5189842542417,
-8.4016402675109));
#21948=CARTESIAN_POINT('Ctrl Pts',(-7.27603390513785,-93.3439842542418,
-4.20082013374671));
#21949=CARTESIAN_POINT('Ctrl Pts',(-9.70137854017372,-93.1689842542418,
1.74701493417668E-11));
#21950=CARTESIAN_POINT('Ctrl Pts',(-7.27603390512272,-92.9939842542417,
4.20082013377292));
#21951=CARTESIAN_POINT('Ctrl Pts',(-4.85068927007173,-92.8189842542418,
8.40164026752836));
#21952=CARTESIAN_POINT('Ctrl Pts',(1.5129078685785E-11,-92.6439842542418,
8.40164026751963));
#21953=CARTESIAN_POINT('Ctrl Pts',(4.85068927010198,-92.4689842542418,8.4016402675109));
#21954=CARTESIAN_POINT('Ctrl Pts',(7.27603390513785,-92.2939842542418,4.20082013374672));
#21955=CARTESIAN_POINT('Ctrl Pts',(9.70137854017372,-92.1189842542418,-1.74689612655491E-11));
#21956=CARTESIAN_POINT('Ctrl Pts',(7.27603390512273,-91.9439842542417,-4.20082013377291));
#21957=CARTESIAN_POINT('Ctrl Pts',(4.85068927007173,-91.7689842542418,-8.40164026752836));
#21958=CARTESIAN_POINT('Ctrl Pts',(-1.51301075899711E-11,-91.5939842542418,
-8.40164026751963));
#21959=CARTESIAN_POINT('Ctrl Pts',(-4.85068927010199,-91.4189842542417,
-8.4016402675109));
#21960=CARTESIAN_POINT('Ctrl Pts',(-7.27603390513785,-91.2439842542418,
-4.20082013374671));
#21961=CARTESIAN_POINT('Ctrl Pts',(-9.70137854017372,-91.0689842542418,
1.74701493417668E-11));
#21962=CARTESIAN_POINT('Ctrl Pts',(-7.27603390512272,-90.8939842542418,
4.20082013377292));
#21963=CARTESIAN_POINT('Ctrl Pts',(-4.85068927007173,-90.7189842542418,
8.40164026752836));
#21964=CARTESIAN_POINT('Ctrl Pts',(1.5129078685785E-11,-90.5439842542418,
8.40164026751963));
#21965=CARTESIAN_POINT('Ctrl Pts',(4.85068927010198,-90.3689842542418,8.4016402675109));
#21966=CARTESIAN_POINT('Ctrl Pts',(7.27603390513785,-90.1939842542418,4.20082013374672));
#21967=CARTESIAN_POINT('Ctrl Pts',(9.70137854017372,-90.0189842542418,-1.74689612655491E-11));
#21968=CARTESIAN_POINT('Ctrl Pts',(7.27603390512273,-89.8439842542418,-4.20082013377291));
#21969=CARTESIAN_POINT('Ctrl Pts',(4.85068927007173,-89.6689842542418,-8.40164026752836));
#21970=CARTESIAN_POINT('Ctrl Pts',(-1.51301075899711E-11,-89.4939842542418,
-8.40164026751963));
#21971=CARTESIAN_POINT('Ctrl Pts',(-4.85068927010199,-89.3189842542418,
-8.4016402675109));
#21972=CARTESIAN_POINT('Ctrl Pts',(-7.27603390513785,-89.1439842542418,
-4.20082013374671));
#21973=CARTESIAN_POINT('Ctrl Pts',(-9.70137854017372,-88.9689842542418,
1.74701493417668E-11));
#21974=CARTESIAN_POINT('Ctrl Pts',(-7.27603390512272,-88.7939842542418,
4.20082013377292));
#21975=CARTESIAN_POINT('Ctrl Pts',(-4.85068927007173,-88.6189842542418,
8.40164026752836));
#21976=CARTESIAN_POINT('Ctrl Pts',(1.5129078685785E-11,-88.4439842542418,
8.40164026751963));
#21977=CARTESIAN_POINT('Ctrl Pts',(4.85068927010198,-88.2689842542418,8.4016402675109));
#21978=CARTESIAN_POINT('Ctrl Pts',(7.27603390513785,-88.0939842542418,4.20082013374672));
#21979=CARTESIAN_POINT('Ctrl Pts',(9.70137854017372,-87.9189842542418,-1.74689612655491E-11));
#21980=CARTESIAN_POINT('Ctrl Pts',(7.27603390512273,-87.7439842542418,-4.20082013377291));
#21981=CARTESIAN_POINT('Ctrl Pts',(4.85068927007173,-87.5689842542418,-8.40164026752836));
#21982=CARTESIAN_POINT('Ctrl Pts',(-1.51301075899711E-11,-87.3939842542418,
-8.40164026751963));
#21983=CARTESIAN_POINT('Ctrl Pts',(-4.85068927010199,-87.2189842542418,
-8.4016402675109));
#21984=CARTESIAN_POINT('Ctrl Pts',(-7.27603390513785,-87.0439842542418,
-4.20082013374671));
#21985=CARTESIAN_POINT('Ctrl Pts',(-9.70137854017372,-86.8689842542418,
1.74701493417668E-11));
#21986=CARTESIAN_POINT('Ctrl Pts',(-7.27603390512272,-86.6939842542418,
4.20082013377292));
#21987=CARTESIAN_POINT('Ctrl Pts',(-4.85068927007173,-86.5189842542418,
8.40164026752836));
#21988=CARTESIAN_POINT('Ctrl Pts',(1.5129078685785E-11,-86.3439842542418,
8.40164026751963));
#21989=CARTESIAN_POINT('Ctrl Pts',(4.85068927010198,-86.1689842542418,8.4016402675109));
#21990=CARTESIAN_POINT('Ctrl Pts',(7.27603390513785,-85.9939842542418,4.20082013374672));
#21991=CARTESIAN_POINT('Ctrl Pts',(9.70137854017372,-85.8189842542418,-1.74689612655491E-11));
#21992=CARTESIAN_POINT('Ctrl Pts',(7.27603390512273,-85.6439842542418,-4.20082013377291));
#21993=CARTESIAN_POINT('Ctrl Pts',(4.85068927007173,-85.4689842542418,-8.40164026752836));
#21994=CARTESIAN_POINT('Ctrl Pts',(-1.51301075899711E-11,-85.2939842542417,
-8.40164026751963));
#21995=CARTESIAN_POINT('Ctrl Pts',(-4.85068927010199,-85.1189842542418,
-8.4016402675109));
#21996=CARTESIAN_POINT('Ctrl Pts',(-7.27603390513785,-84.9439842542418,
-4.20082013374671));
#21997=CARTESIAN_POINT('Ctrl Pts',(-9.70137854017372,-84.7689842542418,
1.74701493417668E-11));
#21998=CARTESIAN_POINT('Ctrl Pts',(-7.27603390512272,-84.5939842542418,
4.20082013377292));
#21999=CARTESIAN_POINT('Ctrl Pts',(-4.85068927007173,-84.4189842542418,
8.40164026752836));
#22000=CARTESIAN_POINT('Ctrl Pts',(1.5129078685785E-11,-84.2439842542418,
8.40164026751963));
#22001=CARTESIAN_POINT('Ctrl Pts',(4.85068927010198,-84.0689842542418,8.4016402675109));
#22002=CARTESIAN_POINT('Ctrl Pts',(7.27603390513785,-83.8939842542418,4.20082013374672));
#22003=CARTESIAN_POINT('Ctrl Pts',(9.70137854017372,-83.7189842542418,-1.74689612655491E-11));
#22004=CARTESIAN_POINT('Ctrl Pts',(7.27603390512273,-83.5439842542418,-4.20082013377291));
#22005=CARTESIAN_POINT('Ctrl Pts',(4.85068927007173,-83.3689842542418,-8.40164026752836));
#22006=CARTESIAN_POINT('Ctrl Pts',(-1.51301075899711E-11,-83.1939842542418,
-8.40164026751963));
#22007=CARTESIAN_POINT('Ctrl Pts',(-4.85068927010199,-83.0189842542418,
-8.4016402675109));
#22008=CARTESIAN_POINT('Ctrl Pts',(-7.27603390513785,-82.8439842542418,
-4.20082013374671));
#22009=CARTESIAN_POINT('Ctrl Pts',(-9.70137854017372,-82.6689842542418,
1.74701493417668E-11));
#22010=CARTESIAN_POINT('Ctrl Pts',(-7.27603390512272,-82.4939842542418,
4.20082013377292));
#22011=CARTESIAN_POINT('Ctrl Pts',(-4.85068927007173,-82.3189842542418,
8.40164026752836));
#22012=CARTESIAN_POINT('Ctrl Pts',(1.5129078685785E-11,-82.1439842542418,
8.40164026751963));
#22013=CARTESIAN_POINT('Ctrl Pts',(4.85068927010198,-81.9689842542418,8.4016402675109));
#22014=CARTESIAN_POINT('Ctrl Pts',(7.27603390513785,-81.7939842542418,4.20082013374672));
#22015=CARTESIAN_POINT('Ctrl Pts',(9.70137854017372,-81.6189842542418,-1.74689612655491E-11));
#22016=CARTESIAN_POINT('Ctrl Pts',(7.27603390512273,-81.4439842542418,-4.20082013377291));
#22017=CARTESIAN_POINT('Ctrl Pts',(4.85068927007173,-81.2689842542418,-8.40164026752836));
#22018=CARTESIAN_POINT('Ctrl Pts',(-1.51301075899711E-11,-81.0939842542418,
-8.40164026751963));
#22019=CARTESIAN_POINT('Ctrl Pts',(-4.85068927010199,-80.9189842542418,
-8.4016402675109));
#22020=CARTESIAN_POINT('Ctrl Pts',(-7.27603390513785,-80.7439842542418,
-4.20082013374671));
#22021=CARTESIAN_POINT('Ctrl Pts',(-9.70137854017372,-80.5689842542418,
1.74701493417668E-11));
#22022=CARTESIAN_POINT('Ctrl Pts',(-7.27603390512272,-80.3939842542418,
4.20082013377292));
#22023=CARTESIAN_POINT('Ctrl Pts',(-4.85068927007173,-80.2189842542418,
8.40164026752836));
#22024=CARTESIAN_POINT('Ctrl Pts',(1.5129078685785E-11,-80.0439842542418,
8.40164026751963));
#22025=CARTESIAN_POINT('Ctrl Pts',(4.85068927010198,-79.8689842542418,8.4016402675109));
#22026=CARTESIAN_POINT('Ctrl Pts',(7.27603390513785,-79.6939842542418,4.20082013374672));
#22027=CARTESIAN_POINT('Ctrl Pts',(9.70137854017372,-79.5189842542418,-1.74689612655491E-11));
#22028=CARTESIAN_POINT('Ctrl Pts',(7.27603390512273,-79.3439842542418,-4.20082013377291));
#22029=CARTESIAN_POINT('Ctrl Pts',(4.85068927007173,-79.1689842542418,-8.40164026752836));
#22030=CARTESIAN_POINT('Ctrl Pts',(-1.51301075899711E-11,-78.9939842542418,
-8.40164026751963));
#22031=CARTESIAN_POINT('Ctrl Pts',(-4.85068927010199,-78.8189842542418,
-8.4016402675109));
#22032=CARTESIAN_POINT('Ctrl Pts',(-7.27603390513785,-78.6439842542418,
-4.20082013374671));
#22033=CARTESIAN_POINT('Ctrl Pts',(-9.70137854017372,-78.4689842542418,
1.74701493417668E-11));
#22034=CARTESIAN_POINT('Ctrl Pts',(-7.27603390512272,-78.2939842542418,
4.20082013377292));
#22035=CARTESIAN_POINT('Ctrl Pts',(-4.85068927007173,-78.1189842542418,
8.40164026752836));
#22036=CARTESIAN_POINT('Ctrl Pts',(1.5129078685785E-11,-77.9439842542418,
8.40164026751963));
#22037=CARTESIAN_POINT('Ctrl Pts',(4.85068927010198,-77.7689842542418,8.4016402675109));
#22038=CARTESIAN_POINT('Ctrl Pts',(7.27603390513785,-77.5939842542418,4.20082013374672));
#22039=CARTESIAN_POINT('Ctrl Pts',(9.70137854017372,-77.4189842542418,-1.74689612655491E-11));
#22040=CARTESIAN_POINT('Ctrl Pts',(7.27603390512273,-77.2439842542418,-4.20082013377291));
#22041=CARTESIAN_POINT('Ctrl Pts',(4.85068927007173,-77.0689842542418,-8.40164026752836));
#22042=CARTESIAN_POINT('Ctrl Pts',(-1.51301075899711E-11,-76.8939842542418,
-8.40164026751963));
#22043=CARTESIAN_POINT('Ctrl Pts',(-4.85068927010199,-76.7189842542418,
-8.4016402675109));
#22044=CARTESIAN_POINT('Ctrl Pts',(-7.27603390513785,-76.5439842542418,
-4.20082013374671));
#22045=CARTESIAN_POINT('Ctrl Pts',(-9.70137854017372,-76.3689842542418,
1.74701493417668E-11));
#22046=CARTESIAN_POINT('Ctrl Pts',(-7.27603390512272,-76.1939842542418,
4.20082013377292));
#22047=CARTESIAN_POINT('Ctrl Pts',(-4.85068927007173,-76.0189842542418,
8.40164026752836));
#22048=CARTESIAN_POINT('Ctrl Pts',(1.5129078685785E-11,-75.8439842542418,
8.40164026751963));
#22049=CARTESIAN_POINT('Ctrl Pts',(4.85068927010198,-75.6689842542418,8.4016402675109));
#22050=CARTESIAN_POINT('Ctrl Pts',(7.27603390513785,-75.4939842542418,4.20082013374672));
#22051=CARTESIAN_POINT('Ctrl Pts',(9.70137854017372,-75.3189842542418,-1.74689612655491E-11));
#22052=CARTESIAN_POINT('Ctrl Pts',(7.27603390512273,-75.1439842542418,-4.20082013377291));
#22053=CARTESIAN_POINT('Ctrl Pts',(4.85068927007173,-74.9689842542418,-8.40164026752836));
#22054=CARTESIAN_POINT('Ctrl Pts',(-1.51301075899711E-11,-74.7939842542418,
-8.40164026751963));
#22055=CARTESIAN_POINT('Ctrl Pts',(-4.85068927010199,-74.6189842542418,
-8.4016402675109));
#22056=CARTESIAN_POINT('Ctrl Pts',(-7.27603390513785,-74.4439842542418,
-4.20082013374671));
#22057=CARTESIAN_POINT('Ctrl Pts',(-9.70137854017372,-74.2689842542418,
1.74701493417668E-11));
#22058=CARTESIAN_POINT('Ctrl Pts',(-7.27603390512272,-74.0939842542418,
4.20082013377292));
#22059=CARTESIAN_POINT('Ctrl Pts',(-4.85068927007173,-73.9189842542418,
8.40164026752836));
#22060=CARTESIAN_POINT('Ctrl Pts',(1.5129078685785E-11,-73.7439842542418,
8.40164026751963));
#22061=CARTESIAN_POINT('Ctrl Pts',(4.85068927010198,-73.5689842542418,8.4016402675109));
#22062=CARTESIAN_POINT('Ctrl Pts',(7.27603390513785,-73.3939842542418,4.20082013374672));
#22063=CARTESIAN_POINT('Ctrl Pts',(9.70137854017372,-73.2189842542418,-1.74689612655491E-11));
#22064=CARTESIAN_POINT('Ctrl Pts',(7.27603390512273,-73.0439842542418,-4.20082013377291));
#22065=CARTESIAN_POINT('Ctrl Pts',(4.85068927007173,-72.8689842542418,-8.40164026752836));
#22066=CARTESIAN_POINT('Ctrl Pts',(-1.51301075899711E-11,-72.6939842542418,
-8.40164026751963));
#22067=CARTESIAN_POINT('Ctrl Pts',(-4.85068927010199,-72.5189842542418,
-8.4016402675109));
#22068=CARTESIAN_POINT('Ctrl Pts',(-7.27603390513785,-72.3439842542418,
-4.20082013374671));
#22069=CARTESIAN_POINT('Ctrl Pts',(-9.70137854017372,-72.1689842542418,
1.74701493417668E-11));
#22070=CARTESIAN_POINT('Ctrl Pts',(-7.27603390512272,-71.9939842542418,
4.20082013377292));
#22071=CARTESIAN_POINT('Ctrl Pts',(-4.85068927007173,-71.8189842542418,
8.40164026752836));
#22072=CARTESIAN_POINT('Ctrl Pts',(1.5129078685785E-11,-71.6439842542418,
8.40164026751963));
#22073=CARTESIAN_POINT('Ctrl Pts',(4.85068927010198,-71.4689842542418,8.4016402675109));
#22074=CARTESIAN_POINT('Ctrl Pts',(7.27603390513785,-71.2939842542418,4.20082013374672));
#22075=CARTESIAN_POINT('Ctrl Pts',(9.70137854017372,-71.1189842542418,-1.74689612655491E-11));
#22076=CARTESIAN_POINT('Ctrl Pts',(7.27603390512273,-70.9439842542418,-4.20082013377291));
#22077=CARTESIAN_POINT('Ctrl Pts',(4.85068927007173,-70.7689842542418,-8.40164026752836));
#22078=CARTESIAN_POINT('Ctrl Pts',(-1.51301075899711E-11,-70.5939842542418,
-8.40164026751963));
#22079=CARTESIAN_POINT('Ctrl Pts',(-4.85068927010199,-70.4189842542418,
-8.4016402675109));
#22080=CARTESIAN_POINT('Ctrl Pts',(-7.27603390513785,-70.2439842542418,
-4.20082013374671));
#22081=CARTESIAN_POINT('Ctrl Pts',(-9.70137854017372,-70.0689842542418,
1.74701493417668E-11));
#22082=CARTESIAN_POINT('Ctrl Pts',(-7.27603390512272,-69.8939842542418,
4.20082013377292));
#22083=CARTESIAN_POINT('Ctrl Pts',(-4.85068927007173,-69.7189842542418,
8.40164026752836));
#22084=CARTESIAN_POINT('Ctrl Pts',(1.5129078685785E-11,-69.5439842542418,
8.40164026751963));
#22085=CARTESIAN_POINT('Ctrl Pts',(4.85068927010198,-69.3689842542418,8.4016402675109));
#22086=CARTESIAN_POINT('Ctrl Pts',(7.27603390513785,-69.1939842542418,4.20082013374672));
#22087=CARTESIAN_POINT('Ctrl Pts',(9.70137854017372,-69.0189842542418,-1.74689612655491E-11));
#22088=CARTESIAN_POINT('Ctrl Pts',(7.27603390512273,-68.8439842542418,-4.20082013377291));
#22089=CARTESIAN_POINT('Ctrl Pts',(4.85068927007173,-68.6689842542418,-8.40164026752836));
#22090=CARTESIAN_POINT('Ctrl Pts',(-1.51301075899711E-11,-68.4939842542418,
-8.40164026751963));
#22091=CARTESIAN_POINT('Ctrl Pts',(-4.85068927010199,-68.3189842542418,
-8.4016402675109));
#22092=CARTESIAN_POINT('Ctrl Pts',(-7.27603390513785,-68.1439842542418,
-4.20082013374671));
#22093=CARTESIAN_POINT('Ctrl Pts',(-9.70137854017372,-67.9689842542418,
1.74701493417668E-11));
#22094=CARTESIAN_POINT('Ctrl Pts',(-7.27603390512272,-67.7939842542418,
4.20082013377292));
#22095=CARTESIAN_POINT('Ctrl Pts',(-4.85068927007173,-67.6189842542418,
8.40164026752836));
#22096=CARTESIAN_POINT('Ctrl Pts',(1.5129078685785E-11,-67.4439842542418,
8.40164026751963));
#22097=CARTESIAN_POINT('Ctrl Pts',(4.85068927010198,-67.2689842542418,8.4016402675109));
#22098=CARTESIAN_POINT('Ctrl Pts',(7.27603390513785,-67.0939842542418,4.20082013374672));
#22099=CARTESIAN_POINT('Ctrl Pts',(9.70137854017372,-66.9189842542418,-1.74689612655491E-11));
#22100=CARTESIAN_POINT('Ctrl Pts',(7.27603390512273,-66.7439842542418,-4.20082013377291));
#22101=CARTESIAN_POINT('Ctrl Pts',(4.85068927007173,-66.5689842542419,-8.40164026752836));
#22102=CARTESIAN_POINT('Ctrl Pts',(-1.51301075899711E-11,-66.3939842542418,
-8.40164026751963));
#22103=CARTESIAN_POINT('Ctrl Pts',(-4.85068927010199,-66.2189842542418,
-8.4016402675109));
#22104=CARTESIAN_POINT('Ctrl Pts',(-7.27603390513785,-66.0439842542418,
-4.20082013374671));
#22105=CARTESIAN_POINT('Ctrl Pts',(-9.70137854017372,-65.8689842542418,
1.74701493417668E-11));
#22106=CARTESIAN_POINT('Ctrl Pts',(-7.27603390512272,-65.6939842542418,
4.20082013377292));
#22107=CARTESIAN_POINT('Ctrl Pts',(-4.85068927007173,-65.5189842542418,
8.40164026752836));
#22108=CARTESIAN_POINT('Ctrl Pts',(1.5129078685785E-11,-65.3439842542418,
8.40164026751963));
#22109=CARTESIAN_POINT('Ctrl Pts',(4.85068927010198,-65.1689842542418,8.4016402675109));
#22110=CARTESIAN_POINT('Ctrl Pts',(7.27603390513785,-64.9939842542418,4.20082013374672));
#22111=CARTESIAN_POINT('Ctrl Pts',(9.70137854017372,-64.8189842542418,-1.74689612655491E-11));
#22112=CARTESIAN_POINT('Ctrl Pts',(7.27603390512273,-64.6439842542418,-4.20082013377291));
#22113=CARTESIAN_POINT('Ctrl Pts',(4.85068927007173,-64.4689842542418,-8.40164026752836));
#22114=CARTESIAN_POINT('Ctrl Pts',(-1.51301075899711E-11,-64.2939842542418,
-8.40164026751963));
#22115=CARTESIAN_POINT('Ctrl Pts',(-4.85068927010199,-64.1189842542418,
-8.4016402675109));
#22116=CARTESIAN_POINT('Ctrl Pts',(-7.27603390513785,-63.9439842542418,
-4.20082013374671));
#22117=CARTESIAN_POINT('Ctrl Pts',(-9.70137854017372,-63.7689842542418,
1.74701493417668E-11));
#22118=CARTESIAN_POINT('Ctrl Pts',(-7.27603390512272,-63.5939842542418,
4.20082013377292));
#22119=CARTESIAN_POINT('Ctrl Pts',(-4.85068927007173,-63.4189842542418,
8.40164026752836));
#22120=CARTESIAN_POINT('Ctrl Pts',(1.5129078685785E-11,-63.2439842542418,
8.40164026751963));
#22121=CARTESIAN_POINT('Ctrl Pts',(4.85068927010198,-63.0689842542418,8.4016402675109));
#22122=CARTESIAN_POINT('Ctrl Pts',(7.27603390513785,-62.8939842542418,4.20082013374672));
#22123=CARTESIAN_POINT('Ctrl Pts',(9.70137854017372,-62.7189842542418,-1.74689612655491E-11));
#22124=CARTESIAN_POINT('Ctrl Pts',(7.27603390512273,-62.5439842542418,-4.20082013377291));
#22125=CARTESIAN_POINT('Ctrl Pts',(4.85068927007173,-62.3689842542419,-8.40164026752836));
#22126=CARTESIAN_POINT('Ctrl Pts',(-1.51301075899711E-11,-62.1939842542418,
-8.40164026751963));
#22127=CARTESIAN_POINT('Ctrl Pts',(-4.85068927010199,-62.0189842542418,
-8.4016402675109));
#22128=CARTESIAN_POINT('Ctrl Pts',(-7.27603390513785,-61.8439842542418,
-4.20082013374671));
#22129=CARTESIAN_POINT('Ctrl Pts',(-9.70137854017372,-61.6689842542418,
1.74701493417668E-11));
#22130=CARTESIAN_POINT('Ctrl Pts',(-7.27603390512272,-61.4939842542418,
4.20082013377292));
#22131=CARTESIAN_POINT('Ctrl Pts',(-4.85068927007173,-61.3189842542419,
8.40164026752836));
#22132=CARTESIAN_POINT('Ctrl Pts',(1.5129078685785E-11,-61.1439842542418,
8.40164026751963));
#22133=CARTESIAN_POINT('Ctrl Pts',(4.85068927010198,-60.9689842542418,8.4016402675109));
#22134=CARTESIAN_POINT('Ctrl Pts',(7.27603390513785,-60.7939842542418,4.20082013374672));
#22135=CARTESIAN_POINT('Ctrl Pts',(9.70137854017372,-60.6189842542418,-1.74689612655491E-11));
#22136=CARTESIAN_POINT('Ctrl Pts',(7.27603390512273,-60.4439842542418,-4.20082013377291));
#22137=CARTESIAN_POINT('Ctrl Pts',(4.85068927007173,-60.2689842542419,-8.40164026752836));
#22138=CARTESIAN_POINT('Ctrl Pts',(-1.51301075899711E-11,-60.0939842542418,
-8.40164026751963));
#22139=CARTESIAN_POINT('Ctrl Pts',(-4.85068927010199,-59.9189842542418,
-8.4016402675109));
#22140=CARTESIAN_POINT('Ctrl Pts',(-7.27603390513785,-59.7439842542419,
-4.20082013374671));
#22141=CARTESIAN_POINT('Ctrl Pts',(-9.70137854017372,-59.5689842542418,
1.74701493417668E-11));
#22142=CARTESIAN_POINT('Ctrl Pts',(-7.27603390512272,-59.3939842542418,
4.20082013377292));
#22143=CARTESIAN_POINT('Ctrl Pts',(-4.85068927007173,-59.2189842542419,
8.40164026752836));
#22144=CARTESIAN_POINT('Ctrl Pts',(1.5129078685785E-11,-59.0439842542418,
8.40164026751963));
#22145=CARTESIAN_POINT('Ctrl Pts',(4.85068927010198,-58.8689842542419,8.4016402675109));
#22146=CARTESIAN_POINT('Ctrl Pts',(7.27603390513785,-58.6939842542419,4.20082013374672));
#22147=CARTESIAN_POINT('Ctrl Pts',(9.70137854017372,-58.5189842542418,-1.74689612655491E-11));
#22148=CARTESIAN_POINT('Ctrl Pts',(7.27603390512273,-58.3439842542418,-4.20082013377291));
#22149=CARTESIAN_POINT('Ctrl Pts',(4.85068927007173,-58.1689842542419,-8.40164026752836));
#22150=CARTESIAN_POINT('Ctrl Pts',(-1.51301075899711E-11,-57.9939842542418,
-8.40164026751963));
#22151=CARTESIAN_POINT('Ctrl Pts',(-4.85068927010199,-57.8189842542418,
-8.4016402675109));
#22152=CARTESIAN_POINT('Ctrl Pts',(-7.27603390513785,-57.6439842542418,
-4.20082013374671));
#22153=CARTESIAN_POINT('Ctrl Pts',(-9.70137854017372,-57.4689842542418,
1.74701493417668E-11));
#22154=CARTESIAN_POINT('Ctrl Pts',(-7.27603390512272,-57.2939842542418,
4.20082013377292));
#22155=CARTESIAN_POINT('Ctrl Pts',(-4.85068927007173,-57.1189842542418,
8.40164026752836));
#22156=CARTESIAN_POINT('Ctrl Pts',(1.5129078685785E-11,-56.9439842542418,
8.40164026751963));
#22157=CARTESIAN_POINT('Ctrl Pts',(4.85068927010198,-56.7689842542419,8.4016402675109));
#22158=CARTESIAN_POINT('Ctrl Pts',(7.27603390513785,-56.5939842542418,4.20082013374672));
#22159=CARTESIAN_POINT('Ctrl Pts',(9.70137854017372,-56.4189842542418,-1.74689612655491E-11));
#22160=CARTESIAN_POINT('Ctrl Pts',(7.27603390512273,-56.2439842542419,-4.20082013377291));
#22161=CARTESIAN_POINT('Ctrl Pts',(4.85068927007173,-56.0689842542418,-8.40164026752836));
#22162=CARTESIAN_POINT('Ctrl Pts',(-1.51301075899711E-11,-55.8939842542418,
-8.40164026751963));
#22163=CARTESIAN_POINT('Ctrl Pts',(-4.85068927010199,-55.7189842542419,
-8.4016402675109));
#22164=CARTESIAN_POINT('Ctrl Pts',(-7.27603390513785,-55.5439842542418,
-4.20082013374671));
#22165=CARTESIAN_POINT('Ctrl Pts',(-9.70137854017372,-55.3689842542418,
1.74701493417668E-11));
#22166=CARTESIAN_POINT('Ctrl Pts',(-7.27603390512272,-55.1939842542419,
4.20082013377292));
#22167=CARTESIAN_POINT('Ctrl Pts',(-4.85068927007173,-55.0189842542419,
8.40164026752836));
#22168=CARTESIAN_POINT('Ctrl Pts',(1.5129078685785E-11,-54.8439842542419,
8.40164026751963));
#22169=CARTESIAN_POINT('Ctrl Pts',(4.85068927010198,-54.6689842542418,8.4016402675109));
#22170=CARTESIAN_POINT('Ctrl Pts',(7.27603390513785,-54.4939842542419,4.20082013374672));
#22171=CARTESIAN_POINT('Ctrl Pts',(9.70137854017372,-54.3189842542419,-1.74689612655491E-11));
#22172=CARTESIAN_POINT('Ctrl Pts',(7.27603390512273,-54.1439842542419,-4.20082013377291));
#22173=CARTESIAN_POINT('Ctrl Pts',(4.85068927007173,-53.9689842542419,-8.40164026752836));
#22174=CARTESIAN_POINT('Ctrl Pts',(-1.51301075899711E-11,-53.7939842542419,
-8.40164026751963));
#22175=CARTESIAN_POINT('Ctrl Pts',(-4.85068927010199,-53.6189842542419,
-8.4016402675109));
#22176=CARTESIAN_POINT('Ctrl Pts',(-7.27603390513785,-53.4439842542418,
-4.20082013374671));
#22177=CARTESIAN_POINT('Ctrl Pts',(-9.70137854017372,-53.2689842542418,
1.74701493417668E-11));
#22178=CARTESIAN_POINT('Ctrl Pts',(-7.27603390512272,-53.0939842542418,
4.20082013377292));
#22179=CARTESIAN_POINT('Ctrl Pts',(-4.85068927007173,-52.9189842542419,
8.40164026752836));
#22180=CARTESIAN_POINT('Ctrl Pts',(1.5129078685785E-11,-52.7439842542418,
8.40164026751963));
#22181=CARTESIAN_POINT('Ctrl Pts',(4.85068927010198,-52.5689842542419,8.4016402675109));
#22182=CARTESIAN_POINT('Ctrl Pts',(7.27603390513785,-52.3939842542419,4.20082013374672));
#22183=CARTESIAN_POINT('Ctrl Pts',(9.70137854017372,-52.2189842542419,-1.74689612655491E-11));
#22184=CARTESIAN_POINT('Ctrl Pts',(7.27603390512273,-52.0439842542418,-4.20082013377291));
#22185=CARTESIAN_POINT('Ctrl Pts',(4.85068927007173,-51.8689842542419,-8.40164026752836));
#22186=CARTESIAN_POINT('Ctrl Pts',(-1.51301075899711E-11,-51.6939842542418,
-8.40164026751963));
#22187=CARTESIAN_POINT('Ctrl Pts',(-4.85068927010199,-51.5189842542419,
-8.4016402675109));
#22188=CARTESIAN_POINT('Ctrl Pts',(-7.27603390513785,-51.3439842542419,
-4.20082013374671));
#22189=CARTESIAN_POINT('Ctrl Pts',(-9.70137854017372,-51.1689842542419,
1.74701493417668E-11));
#22190=CARTESIAN_POINT('Ctrl Pts',(-7.27603390512272,-50.9939842542419,
4.20082013377292));
#22191=CARTESIAN_POINT('Ctrl Pts',(-4.85068927007173,-50.8189842542419,
8.40164026752836));
#22192=CARTESIAN_POINT('Ctrl Pts',(1.5129078685785E-11,-50.6439842542419,
8.40164026751963));
#22193=CARTESIAN_POINT('Ctrl Pts',(4.85068927010198,-50.4689842542419,8.4016402675109));
#22194=CARTESIAN_POINT('Ctrl Pts',(7.27603390513785,-50.2939842542418,4.20082013374672));
#22195=CARTESIAN_POINT('Ctrl Pts',(9.70137854017372,-50.1189842542419,-1.74689612655491E-11));
#22196=CARTESIAN_POINT('Ctrl Pts',(7.27603390512273,-49.9439842542419,-4.20082013377291));
#22197=CARTESIAN_POINT('Ctrl Pts',(4.85068927007173,-49.7689842542419,-8.40164026752836));
#22198=CARTESIAN_POINT('Ctrl Pts',(-1.51301075899711E-11,-49.5939842542419,
-8.40164026751963));
#22199=CARTESIAN_POINT('Ctrl Pts',(-4.85068927010199,-49.4189842542419,
-8.4016402675109));
#22200=CARTESIAN_POINT('Ctrl Pts',(-7.27603390513785,-49.2439842542419,
-4.20082013374671));
#22201=CARTESIAN_POINT('Ctrl Pts',(-9.70137854017372,-49.0689842542419,
1.74701493417668E-11));
#22202=CARTESIAN_POINT('Ctrl Pts',(-7.27603390512272,-48.8939842542419,
4.20082013377292));
#22203=CARTESIAN_POINT('Ctrl Pts',(-4.85068927007173,-48.7189842542419,
8.40164026752836));
#22204=CARTESIAN_POINT('Ctrl Pts',(1.5129078685785E-11,-48.5439842542419,
8.40164026751963));
#22205=CARTESIAN_POINT('Ctrl Pts',(4.85068927010198,-48.3689842542419,8.4016402675109));
#22206=CARTESIAN_POINT('Ctrl Pts',(7.27603390513785,-48.1939842542419,4.20082013374672));
#22207=CARTESIAN_POINT('Ctrl Pts',(9.70137854017372,-48.0189842542419,-1.74689612655491E-11));
#22208=CARTESIAN_POINT('Ctrl Pts',(7.27603390512273,-47.8439842542419,-4.20082013377291));
#22209=CARTESIAN_POINT('Ctrl Pts',(4.85068927007173,-47.6689842542419,-8.40164026752836));
#22210=CARTESIAN_POINT('Ctrl Pts',(-1.51301075899711E-11,-47.4939842542419,
-8.40164026751963));
#22211=CARTESIAN_POINT('Ctrl Pts',(-4.85068927010199,-47.3189842542419,
-8.4016402675109));
#22212=CARTESIAN_POINT('Ctrl Pts',(-7.27603390513785,-47.1439842542419,
-4.20082013374671));
#22213=CARTESIAN_POINT('Ctrl Pts',(-9.70137854017372,-46.9689842542419,
1.74701493417668E-11));
#22214=CARTESIAN_POINT('Ctrl Pts',(-7.27603390512272,-46.7939842542419,
4.20082013377292));
#22215=CARTESIAN_POINT('Ctrl Pts',(-4.85068927007173,-46.6189842542419,
8.40164026752836));
#22216=CARTESIAN_POINT('Ctrl Pts',(1.5129078685785E-11,-46.4439842542419,
8.40164026751963));
#22217=CARTESIAN_POINT('Ctrl Pts',(4.85068927010198,-46.2689842542419,8.4016402675109));
#22218=CARTESIAN_POINT('Ctrl Pts',(7.27603390513785,-46.0939842542419,4.20082013374672));
#22219=CARTESIAN_POINT('Ctrl Pts',(9.70137854017372,-45.9189842542419,-1.74689612655491E-11));
#22220=CARTESIAN_POINT('Ctrl Pts',(7.27603390512273,-45.7439842542419,-4.20082013377291));
#22221=CARTESIAN_POINT('Ctrl Pts',(4.85068927007173,-45.5689842542419,-8.40164026752836));
#22222=CARTESIAN_POINT('Ctrl Pts',(-1.51301075899711E-11,-45.3939842542419,
-8.40164026751963));
#22223=CARTESIAN_POINT('Ctrl Pts',(-4.85068927010199,-45.2189842542419,
-8.4016402675109));
#22224=CARTESIAN_POINT('Ctrl Pts',(-7.27603390513785,-45.0439842542419,
-4.20082013374671));
#22225=CARTESIAN_POINT('Ctrl Pts',(-9.70137854017372,-44.8689842542419,
1.74701493417668E-11));
#22226=CARTESIAN_POINT('Ctrl Pts',(-7.27603390512272,-44.6939842542419,
4.20082013377292));
#22227=CARTESIAN_POINT('Ctrl Pts',(-4.85068927007173,-44.5189842542419,
8.40164026752836));
#22228=CARTESIAN_POINT('Ctrl Pts',(1.5129078685785E-11,-44.3439842542419,
8.40164026751963));
#22229=CARTESIAN_POINT('Ctrl Pts',(4.85068927010198,-44.1689842542419,8.4016402675109));
#22230=CARTESIAN_POINT('Ctrl Pts',(7.27603390513785,-43.9939842542419,4.20082013374672));
#22231=CARTESIAN_POINT('Ctrl Pts',(9.70137854017372,-43.8189842542419,-1.74689612655491E-11));
#22232=CARTESIAN_POINT('Ctrl Pts',(7.27603390512273,-43.6439842542419,-4.20082013377291));
#22233=CARTESIAN_POINT('Ctrl Pts',(4.85068927007173,-43.4689842542419,-8.40164026752836));
#22234=CARTESIAN_POINT('Ctrl Pts',(-1.51301075899711E-11,-43.2939842542419,
-8.40164026751963));
#22235=CARTESIAN_POINT('Ctrl Pts',(-4.85068927010199,-43.1189842542419,
-8.4016402675109));
#22236=CARTESIAN_POINT('Ctrl Pts',(-7.27603390513785,-42.9439842542419,
-4.20082013374671));
#22237=CARTESIAN_POINT('Ctrl Pts',(-9.70137854017372,-42.7689842542419,
1.74701493417668E-11));
#22238=CARTESIAN_POINT('Ctrl Pts',(-7.27603390512272,-42.5939842542419,
4.20082013377292));
#22239=CARTESIAN_POINT('Ctrl Pts',(-4.85068927007173,-42.4189842542419,
8.40164026752836));
#22240=CARTESIAN_POINT('Ctrl Pts',(1.5129078685785E-11,-42.2439842542419,
8.40164026751963));
#22241=CARTESIAN_POINT('Ctrl Pts',(4.85068927010198,-42.0689842542419,8.4016402675109));
#22242=CARTESIAN_POINT('Ctrl Pts',(7.27603390513785,-41.8939842542419,4.20082013374672));
#22243=CARTESIAN_POINT('Ctrl Pts',(9.70137854017372,-41.7189842542419,-1.74689612655491E-11));
#22244=CARTESIAN_POINT('Ctrl Pts',(7.27603390512273,-41.5439842542419,-4.20082013377291));
#22245=CARTESIAN_POINT('Ctrl Pts',(4.85068927007173,-41.3689842542419,-8.40164026752836));
#22246=CARTESIAN_POINT('Ctrl Pts',(-1.51301075899711E-11,-41.1939842542419,
-8.40164026751963));
#22247=CARTESIAN_POINT('Ctrl Pts',(-4.85068927010199,-41.0189842542419,
-8.4016402675109));
#22248=CARTESIAN_POINT('Ctrl Pts',(-7.27603390513785,-40.8439842542419,
-4.20082013374671));
#22249=CARTESIAN_POINT('Ctrl Pts',(-9.70137854017372,-40.6689842542419,
1.74701493417668E-11));
#22250=CARTESIAN_POINT('Ctrl Pts',(-7.27603390512272,-40.4939842542419,
4.20082013377292));
#22251=CARTESIAN_POINT('Ctrl Pts',(-4.85068927007173,-40.3189842542419,
8.40164026752836));
#22252=CARTESIAN_POINT('Ctrl Pts',(1.5129078685785E-11,-40.1439842542419,
8.40164026751963));
#22253=CARTESIAN_POINT('Ctrl Pts',(4.85068927010198,-39.9689842542419,8.4016402675109));
#22254=CARTESIAN_POINT('Ctrl Pts',(7.27603390513785,-39.7939842542419,4.20082013374672));
#22255=CARTESIAN_POINT('Ctrl Pts',(9.70137854017372,-39.6189842542419,-1.74689612655491E-11));
#22256=CARTESIAN_POINT('Ctrl Pts',(7.27603390512273,-39.4439842542419,-4.20082013377291));
#22257=CARTESIAN_POINT('Ctrl Pts',(4.85068927007173,-39.2689842542419,-8.40164026752836));
#22258=CARTESIAN_POINT('Ctrl Pts',(-1.51301075899711E-11,-39.0939842542419,
-8.40164026751963));
#22259=CARTESIAN_POINT('Ctrl Pts',(-4.85068927010199,-38.9189842542419,
-8.4016402675109));
#22260=CARTESIAN_POINT('Ctrl Pts',(-7.27603390513785,-38.7439842542419,
-4.20082013374671));
#22261=CARTESIAN_POINT('Ctrl Pts',(-9.70137854017372,-38.5689842542419,
1.74701493417668E-11));
#22262=CARTESIAN_POINT('Ctrl Pts',(-7.27603390512272,-38.3939842542419,
4.20082013377292));
#22263=CARTESIAN_POINT('Ctrl Pts',(-4.85068927007173,-38.2189842542419,
8.40164026752836));
#22264=CARTESIAN_POINT('Ctrl Pts',(1.5129078685785E-11,-38.0439842542419,
8.40164026751963));
#22265=CARTESIAN_POINT('Ctrl Pts',(4.85068927010198,-37.8689842542419,8.4016402675109));
#22266=CARTESIAN_POINT('Ctrl Pts',(7.27603390513785,-37.6939842542419,4.20082013374672));
#22267=CARTESIAN_POINT('Ctrl Pts',(9.70137854017372,-37.5189842542419,-1.74689612655491E-11));
#22268=CARTESIAN_POINT('Ctrl Pts',(7.27603390512273,-37.3439842542419,-4.20082013377291));
#22269=CARTESIAN_POINT('Ctrl Pts',(4.85068927007173,-37.1689842542419,-8.40164026752836));
#22270=CARTESIAN_POINT('Ctrl Pts',(-1.51301075899711E-11,-36.9939842542419,
-8.40164026751963));
#22271=CARTESIAN_POINT('Ctrl Pts',(-4.85068927010199,-36.8189842542419,
-8.4016402675109));
#22272=CARTESIAN_POINT('Ctrl Pts',(-7.27603390513785,-36.6439842542419,
-4.20082013374671));
#22273=CARTESIAN_POINT('Ctrl Pts',(-9.70137854017372,-36.4689842542419,
1.74701493417668E-11));
#22274=CARTESIAN_POINT('Ctrl Pts',(-7.27603390512272,-36.2939842542419,
4.20082013377292));
#22275=CARTESIAN_POINT('Ctrl Pts',(-4.85068927007173,-36.1189842542419,
8.40164026752836));
#22276=CARTESIAN_POINT('Ctrl Pts',(1.5129078685785E-11,-35.9439842542419,
8.40164026751963));
#22277=CARTESIAN_POINT('Ctrl Pts',(4.85068927010198,-35.7689842542419,8.4016402675109));
#22278=CARTESIAN_POINT('Ctrl Pts',(7.27603390513785,-35.5939842542419,4.20082013374672));
#22279=CARTESIAN_POINT('Ctrl Pts',(9.70137854017372,-35.4189842542419,-1.74689612655491E-11));
#22280=CARTESIAN_POINT('Ctrl Pts',(7.27603390512273,-35.2439842542419,-4.20082013377291));
#22281=CARTESIAN_POINT('Ctrl Pts',(4.85068927007173,-35.0689842542419,-8.40164026752836));
#22282=CARTESIAN_POINT('Ctrl Pts',(-1.51301075899711E-11,-34.8939842542419,
-8.40164026751963));
#22283=CARTESIAN_POINT('Ctrl Pts',(-4.85068927010199,-34.7189842542419,
-8.4016402675109));
#22284=CARTESIAN_POINT('Ctrl Pts',(-7.27603390513785,-34.5439842542419,
-4.20082013374671));
#22285=CARTESIAN_POINT('Ctrl Pts',(-9.70137854017372,-34.3689842542419,
1.74701493417668E-11));
#22286=CARTESIAN_POINT('Ctrl Pts',(-7.27603390512272,-34.1939842542419,
4.20082013377292));
#22287=CARTESIAN_POINT('Ctrl Pts',(-4.85068927007173,-34.0189842542419,
8.40164026752836));
#22288=CARTESIAN_POINT('Ctrl Pts',(1.5129078685785E-11,-33.8439842542419,
8.40164026751963));
#22289=CARTESIAN_POINT('Ctrl Pts',(4.85068927010198,-33.6689842542419,8.4016402675109));
#22290=CARTESIAN_POINT('Ctrl Pts',(7.27603390513785,-33.4939842542419,4.20082013374672));
#22291=CARTESIAN_POINT('Ctrl Pts',(9.70137854017372,-33.3189842542419,-1.74689612655491E-11));
#22292=CARTESIAN_POINT('Ctrl Pts',(7.27603390512273,-33.1439842542419,-4.20082013377291));
#22293=CARTESIAN_POINT('Ctrl Pts',(4.85068927007173,-32.9689842542419,-8.40164026752836));
#22294=CARTESIAN_POINT('Ctrl Pts',(-1.51301075899711E-11,-32.7939842542419,
-8.40164026751963));
#22295=CARTESIAN_POINT('Ctrl Pts',(-4.85068927010199,-32.6189842542419,
-8.4016402675109));
#22296=CARTESIAN_POINT('Ctrl Pts',(-7.27603390513785,-32.4439842542419,
-4.20082013374671));
#22297=CARTESIAN_POINT('Ctrl Pts',(-9.70137854017372,-32.2689842542419,
1.74701493417668E-11));
#22298=CARTESIAN_POINT('Ctrl Pts',(-7.27603390512272,-32.0939842542419,
4.20082013377292));
#22299=CARTESIAN_POINT('Ctrl Pts',(-4.85068927007173,-31.9189842542419,
8.40164026752836));
#22300=CARTESIAN_POINT('Ctrl Pts',(1.5129078685785E-11,-31.7439842542419,
8.40164026751963));
#22301=CARTESIAN_POINT('Ctrl Pts',(4.85068927010198,-31.5689842542419,8.4016402675109));
#22302=CARTESIAN_POINT('Ctrl Pts',(7.27603390513785,-31.3939842542419,4.20082013374672));
#22303=CARTESIAN_POINT('Ctrl Pts',(9.70137854017372,-31.2189842542419,-1.74689612655491E-11));
#22304=CARTESIAN_POINT('Ctrl Pts',(7.27603390512273,-31.0439842542419,-4.20082013377291));
#22305=CARTESIAN_POINT('Ctrl Pts',(4.85068927007173,-30.8689842542419,-8.40164026752836));
#22306=CARTESIAN_POINT('Ctrl Pts',(-1.51301075899711E-11,-30.6939842542419,
-8.40164026751963));
#22307=CARTESIAN_POINT('Ctrl Pts',(-4.85068927010199,-30.5189842542419,
-8.4016402675109));
#22308=CARTESIAN_POINT('Ctrl Pts',(-7.27603390513785,-30.3439842542419,
-4.20082013374671));
#22309=CARTESIAN_POINT('Ctrl Pts',(-9.70137854017372,-30.1689842542419,
1.74701493417668E-11));
#22310=CARTESIAN_POINT('Ctrl Pts',(-7.27603390512272,-29.9939842542419,
4.20082013377292));
#22311=CARTESIAN_POINT('Ctrl Pts',(-4.85068927007173,-29.8189842542419,
8.40164026752836));
#22312=CARTESIAN_POINT('Ctrl Pts',(1.5129078685785E-11,-29.6439842542419,
8.40164026751963));
#22313=CARTESIAN_POINT('Ctrl Pts',(4.85068927010198,-29.4689842542419,8.4016402675109));
#22314=CARTESIAN_POINT('Ctrl Pts',(7.27603390513785,-29.2939842542419,4.20082013374672));
#22315=CARTESIAN_POINT('Ctrl Pts',(9.70137854017372,-29.1189842542419,-1.74689612655491E-11));
#22316=CARTESIAN_POINT('Ctrl Pts',(7.27603390512273,-28.9439842542419,-4.20082013377291));
#22317=CARTESIAN_POINT('Ctrl Pts',(4.85068927007173,-28.7689842542419,-8.40164026752836));
#22318=CARTESIAN_POINT('Ctrl Pts',(-1.51301075899711E-11,-28.5939842542419,
-8.40164026751963));
#22319=CARTESIAN_POINT('Ctrl Pts',(-4.85068927010199,-28.4189842542419,
-8.4016402675109));
#22320=CARTESIAN_POINT('Ctrl Pts',(-7.27603390513785,-28.2439842542419,
-4.20082013374671));
#22321=CARTESIAN_POINT('Ctrl Pts',(-9.70137854017372,-28.0689842542419,
1.74701493417668E-11));
#22322=CARTESIAN_POINT('Ctrl Pts',(-7.27603390512272,-27.8939842542419,
4.20082013377292));
#22323=CARTESIAN_POINT('Ctrl Pts',(-4.85068927007173,-27.7189842542419,
8.40164026752836));
#22324=CARTESIAN_POINT('Ctrl Pts',(1.5129078685785E-11,-27.5439842542419,
8.40164026751963));
#22325=CARTESIAN_POINT('Ctrl Pts',(4.85068927010198,-27.3689842542419,8.4016402675109));
#22326=CARTESIAN_POINT('Ctrl Pts',(7.27603390513785,-27.1939842542419,4.20082013374672));
#22327=CARTESIAN_POINT('Ctrl Pts',(9.70137854017372,-27.0189842542419,-1.74689612655491E-11));
#22328=CARTESIAN_POINT('Ctrl Pts',(7.27603390512273,-26.8439842542419,-4.20082013377291));
#22329=CARTESIAN_POINT('Ctrl Pts',(4.85068927007173,-26.6689842542419,-8.40164026752836));
#22330=CARTESIAN_POINT('Ctrl Pts',(-1.51301075899711E-11,-26.4939842542419,
-8.40164026751963));
#22331=CARTESIAN_POINT('Ctrl Pts',(-4.85068927010199,-26.3189842542419,
-8.4016402675109));
#22332=CARTESIAN_POINT('Ctrl Pts',(-7.27603390513785,-26.1439842542419,
-4.20082013374671));
#22333=CARTESIAN_POINT('Ctrl Pts',(-9.70137854017372,-25.9689842542419,
1.74701493417668E-11));
#22334=CARTESIAN_POINT('Ctrl Pts',(-7.27603390512272,-25.7939842542419,
4.20082013377292));
#22335=CARTESIAN_POINT('Ctrl Pts',(-4.85068927007173,-25.6189842542419,
8.40164026752836));
#22336=CARTESIAN_POINT('Ctrl Pts',(1.5129078685785E-11,-25.4439842542419,
8.40164026751963));
#22337=CARTESIAN_POINT('Ctrl Pts',(4.85068927010198,-25.2689842542419,8.4016402675109));
#22338=CARTESIAN_POINT('Ctrl Pts',(7.27603390513785,-25.0939842542419,4.20082013374672));
#22339=CARTESIAN_POINT('Ctrl Pts',(9.70137854017372,-24.9189842542419,-1.74689612655491E-11));
#22340=CARTESIAN_POINT('Ctrl Pts',(7.27603390512273,-24.7439842542419,-4.20082013377291));
#22341=CARTESIAN_POINT('Ctrl Pts',(4.85068927007173,-24.5689842542419,-8.40164026752836));
#22342=CARTESIAN_POINT('Ctrl Pts',(-1.51301075899711E-11,-24.3939842542419,
-8.40164026751963));
#22343=CARTESIAN_POINT('Ctrl Pts',(-4.85068927010199,-24.2189842542419,
-8.4016402675109));
#22344=CARTESIAN_POINT('Ctrl Pts',(-7.27603390513785,-24.0439842542419,
-4.20082013374671));
#22345=CARTESIAN_POINT('Ctrl Pts',(-9.70137854017372,-23.8689842542419,
1.74701493417668E-11));
#22346=CARTESIAN_POINT('Ctrl Pts',(-7.27603390512272,-23.6939842542419,
4.20082013377292));
#22347=CARTESIAN_POINT('Ctrl Pts',(-4.85068927007173,-23.5189842542419,
8.40164026752836));
#22348=CARTESIAN_POINT('Ctrl Pts',(1.5129078685785E-11,-23.3439842542419,
8.40164026751963));
#22349=CARTESIAN_POINT('Ctrl Pts',(4.85068927010198,-23.1689842542419,8.4016402675109));
#22350=CARTESIAN_POINT('Ctrl Pts',(7.27603390513785,-22.9939842542419,4.20082013374672));
#22351=CARTESIAN_POINT('Ctrl Pts',(9.70137854017372,-22.8189842542419,-1.74689612655491E-11));
#22352=CARTESIAN_POINT('Ctrl Pts',(7.27603390512273,-22.6439842542419,-4.20082013377291));
#22353=CARTESIAN_POINT('Ctrl Pts',(4.85068927007173,-22.4689842542419,-8.40164026752836));
#22354=CARTESIAN_POINT('Ctrl Pts',(-1.51301075899711E-11,-22.2939842542419,
-8.40164026751963));
#22355=CARTESIAN_POINT('Ctrl Pts',(-4.85068927010199,-22.1189842542419,
-8.4016402675109));
#22356=CARTESIAN_POINT('Ctrl Pts',(-7.27603390513785,-21.9439842542419,
-4.20082013374671));
#22357=CARTESIAN_POINT('Ctrl Pts',(-9.70137854017372,-21.7689842542419,
1.74701493417668E-11));
#22358=CARTESIAN_POINT('Ctrl Pts',(-7.27603390512272,-21.5939842542419,
4.20082013377292));
#22359=CARTESIAN_POINT('Ctrl Pts',(-4.85068927007173,-21.4189842542419,
8.40164026752836));
#22360=CARTESIAN_POINT('Ctrl Pts',(1.5129078685785E-11,-21.2439842542419,
8.40164026751963));
#22361=CARTESIAN_POINT('Ctrl Pts',(4.85068927010198,-21.0689842542419,8.4016402675109));
#22362=CARTESIAN_POINT('Ctrl Pts',(7.27603390513785,-20.8939842542419,4.20082013374672));
#22363=CARTESIAN_POINT('Ctrl Pts',(9.70137854017372,-20.7189842542419,-1.74689612655491E-11));
#22364=CARTESIAN_POINT('Ctrl Pts',(7.27603390512273,-20.5439842542419,-4.20082013377291));
#22365=CARTESIAN_POINT('Ctrl Pts',(4.85068927007173,-20.3689842542419,-8.40164026752836));
#22366=CARTESIAN_POINT('Ctrl Pts',(-1.51301075899711E-11,-20.1939842542419,
-8.40164026751963));
#22367=CARTESIAN_POINT('Ctrl Pts',(-4.85068927010199,-20.0189842542419,
-8.4016402675109));
#22368=CARTESIAN_POINT('Ctrl Pts',(-7.27603390513785,-19.8439842542419,
-4.20082013374671));
#22369=CARTESIAN_POINT('Ctrl Pts',(-9.70137854017372,-19.6689842542419,
1.74701493417668E-11));
#22370=CARTESIAN_POINT('Ctrl Pts',(-7.27603390512272,-19.4939842542419,
4.20082013377292));
#22371=CARTESIAN_POINT('Ctrl Pts',(-4.85068927007173,-19.3189842542419,
8.40164026752836));
#22372=CARTESIAN_POINT('Ctrl Pts',(1.5129078685785E-11,-19.1439842542419,
8.40164026751963));
#22373=CARTESIAN_POINT('Ctrl Pts',(4.85068927010198,-18.9689842542419,8.4016402675109));
#22374=CARTESIAN_POINT('Ctrl Pts',(7.27603390513785,-18.7939842542419,4.20082013374672));
#22375=CARTESIAN_POINT('Ctrl Pts',(9.70137854017372,-18.6189842542419,-1.74689612655491E-11));
#22376=CARTESIAN_POINT('Ctrl Pts',(7.27603390512273,-18.4439842542419,-4.20082013377291));
#22377=CARTESIAN_POINT('Ctrl Pts',(4.85068927007173,-18.2689842542419,-8.40164026752836));
#22378=CARTESIAN_POINT('Ctrl Pts',(-1.51301075899711E-11,-18.0939842542419,
-8.40164026751963));
#22379=CARTESIAN_POINT('Ctrl Pts',(-4.85068927010199,-17.9189842542419,
-8.4016402675109));
#22380=CARTESIAN_POINT('Ctrl Pts',(-7.27603390513785,-17.7439842542419,
-4.20082013374671));
#22381=CARTESIAN_POINT('Ctrl Pts',(-9.70137854017372,-17.5689842542419,
1.74701493417668E-11));
#22382=CARTESIAN_POINT('Ctrl Pts',(-7.27603390512272,-17.3939842542419,
4.20082013377292));
#22383=CARTESIAN_POINT('Ctrl Pts',(-4.85068927007173,-17.2189842542419,
8.40164026752836));
#22384=CARTESIAN_POINT('Ctrl Pts',(1.5129078685785E-11,-17.0439842542419,
8.40164026751963));
#22385=CARTESIAN_POINT('Ctrl Pts',(4.85068927010198,-16.8689842542419,8.4016402675109));
#22386=CARTESIAN_POINT('Ctrl Pts',(7.27603390513785,-16.6939842542419,4.20082013374672));
#22387=CARTESIAN_POINT('Ctrl Pts',(9.70137854017372,-16.518984254242,-1.74689612655491E-11));
#22388=CARTESIAN_POINT('Ctrl Pts',(7.27603390512273,-16.3439842542419,-4.20082013377291));
#22389=CARTESIAN_POINT('Ctrl Pts',(4.85068927007173,-16.1689842542419,-8.40164026752836));
#22390=CARTESIAN_POINT('Ctrl Pts',(-1.51301075899711E-11,-15.9939842542419,
-8.40164026751963));
#22391=CARTESIAN_POINT('Ctrl Pts',(-4.85068927010199,-15.8189842542419,
-8.4016402675109));
#22392=CARTESIAN_POINT('Ctrl Pts',(-7.27603390513785,-15.6439842542419,
-4.20082013374671));
#22393=CARTESIAN_POINT('Ctrl Pts',(-9.70137854017372,-15.4689842542419,
1.74701493417668E-11));
#22394=CARTESIAN_POINT('Ctrl Pts',(-7.27603390512272,-15.2939842542419,
4.20082013377292));
#22395=CARTESIAN_POINT('Ctrl Pts',(-4.85068927007173,-15.1189842542419,
8.40164026752836));
#22396=CARTESIAN_POINT('Ctrl Pts',(1.5129078685785E-11,-14.9439842542419,
8.40164026751963));
#22397=CARTESIAN_POINT('Ctrl Pts',(4.85068927010198,-14.7689842542419,8.4016402675109));
#22398=CARTESIAN_POINT('Ctrl Pts',(7.27603390513785,-14.5939842542419,4.20082013374672));
#22399=CARTESIAN_POINT('Ctrl Pts',(9.70137854017372,-14.4189842542419,-1.74689612655491E-11));
#22400=CARTESIAN_POINT('Ctrl Pts',(7.27603390512273,-14.2439842542419,-4.20082013377291));
#22401=CARTESIAN_POINT('Ctrl Pts',(4.85068927007173,-14.0689842542419,-8.40164026752836));
#22402=CARTESIAN_POINT('Ctrl Pts',(-1.51301075899711E-11,-13.8939842542419,
-8.40164026751963));
#22403=CARTESIAN_POINT('Ctrl Pts',(-4.85068927010199,-13.7189842542419,
-8.4016402675109));
#22404=CARTESIAN_POINT('Ctrl Pts',(-7.27603390513785,-13.5439842542419,
-4.20082013374671));
#22405=CARTESIAN_POINT('Ctrl Pts',(-9.70137854017372,-13.3689842542419,
1.74701493417668E-11));
#22406=CARTESIAN_POINT('Ctrl Pts',(-7.27603390512272,-13.193984254242,4.20082013377292));
#22407=CARTESIAN_POINT('Ctrl Pts',(-4.85068927007173,-13.018984254242,8.40164026752836));
#22408=CARTESIAN_POINT('Ctrl Pts',(1.5129078685785E-11,-12.8439842542419,
8.40164026751963));
#22409=CARTESIAN_POINT('Ctrl Pts',(4.85068927010198,-12.668984254242,8.4016402675109));
#22410=CARTESIAN_POINT('Ctrl Pts',(7.27603390513785,-12.4939842542419,4.20082013374672));
#22411=CARTESIAN_POINT('Ctrl Pts',(9.70137854017372,-12.3189842542419,-1.74689612655491E-11));
#22412=CARTESIAN_POINT('Ctrl Pts',(7.27603390512273,-12.143984254242,-4.20082013377291));
#22413=CARTESIAN_POINT('Ctrl Pts',(4.85068927007173,-11.968984254242,-8.40164026752836));
#22414=CARTESIAN_POINT('Ctrl Pts',(-1.51301075899711E-11,-11.7939842542419,
-8.40164026751963));
#22415=CARTESIAN_POINT('Ctrl Pts',(-4.85068927010199,-11.6189842542419,
-8.4016402675109));
#22416=CARTESIAN_POINT('Ctrl Pts',(-7.27603390513785,-11.443984254242,-4.20082013374671));
#22417=CARTESIAN_POINT('Ctrl Pts',(-9.70137854017372,-11.2689842542419,
1.74701493417668E-11));
#22418=CARTESIAN_POINT('Ctrl Pts',(-7.27603390512272,-11.0939842542419,
4.20082013377292));
#22419=CARTESIAN_POINT('Ctrl Pts',(-4.85068927007173,-10.918984254242,8.40164026752836));
#22420=CARTESIAN_POINT('Ctrl Pts',(1.5129078685785E-11,-10.7439842542419,
8.40164026751963));
#22421=CARTESIAN_POINT('Ctrl Pts',(4.85068927010198,-10.5689842542419,8.4016402675109));
#22422=CARTESIAN_POINT('Ctrl Pts',(7.27603390513785,-10.393984254242,4.20082013374672));
#22423=CARTESIAN_POINT('Ctrl Pts',(9.70137854017372,-10.2189842542419,-1.74689612655491E-11));
#22424=CARTESIAN_POINT('Ctrl Pts',(7.27603390512273,-10.0439842542419,-4.20082013377291));
#22425=CARTESIAN_POINT('Ctrl Pts',(4.85068927007173,-9.86898425424196,-8.40164026752836));
#22426=CARTESIAN_POINT('Ctrl Pts',(-1.51301075899711E-11,-9.69398425424195,
-8.40164026751963));
#22427=CARTESIAN_POINT('Ctrl Pts',(-4.85068927010199,-9.51898425424195,
-8.4016402675109));
#22428=CARTESIAN_POINT('Ctrl Pts',(-7.27603390513785,-9.34398425424196,
-4.20082013374671));
#22429=CARTESIAN_POINT('Ctrl Pts',(-9.70137854017372,-9.16898425424195,
1.74701493417668E-11));
#22430=CARTESIAN_POINT('Ctrl Pts',(-7.27603390512272,-8.99398425424194,
4.20082013377292));
#22431=CARTESIAN_POINT('Ctrl Pts',(-4.85068927007173,-8.81898425424197,
8.40164026752836));
#22432=CARTESIAN_POINT('Ctrl Pts',(1.5129078685785E-11,-8.64398425424195,
8.40164026751963));
#22433=CARTESIAN_POINT('Ctrl Pts',(4.85068927010198,-8.46898425424195,8.4016402675109));
#22434=CARTESIAN_POINT('Ctrl Pts',(7.27603390513785,-8.29398425424196,4.20082013374672));
#22435=CARTESIAN_POINT('Ctrl Pts',(9.70137854017372,-8.11898425424196,-1.74689612655491E-11));
#22436=CARTESIAN_POINT('Ctrl Pts',(7.27603390512273,-7.94398425424195,-4.20082013377291));
#22437=CARTESIAN_POINT('Ctrl Pts',(4.85068927007173,-7.76898425424197,-8.40164026752836));
#22438=CARTESIAN_POINT('Ctrl Pts',(-1.51301075899711E-11,-7.59398425424196,
-8.40164026751963));
#22439=CARTESIAN_POINT('Ctrl Pts',(-4.85068927010199,-7.41898425424196,
-8.4016402675109));
#22440=CARTESIAN_POINT('Ctrl Pts',(-7.27603390513785,-7.24398425424194,
-4.20082013374671));
#22441=CARTESIAN_POINT('Ctrl Pts',(-9.70137854017372,-7.06898425424196,
1.74701493417668E-11));
#22442=CARTESIAN_POINT('Ctrl Pts',(-7.27603390512272,-6.89398425424195,
4.20082013377292));
#22443=CARTESIAN_POINT('Ctrl Pts',(-4.85068927007173,-6.71898425424195,
8.40164026752836));
#22444=CARTESIAN_POINT('Ctrl Pts',(1.5129078685785E-11,-6.54398425424196,
8.40164026751963));
#22445=CARTESIAN_POINT('Ctrl Pts',(4.85068927010198,-6.36898425424197,8.4016402675109));
#22446=CARTESIAN_POINT('Ctrl Pts',(7.27603390513785,-6.19398425424195,4.20082013374672));
#22447=CARTESIAN_POINT('Ctrl Pts',(9.70137854017372,-6.01898425424197,-1.74689612655491E-11));
#22448=CARTESIAN_POINT('Ctrl Pts',(7.27603390512273,-5.84398425424196,-4.20082013377291));
#22449=CARTESIAN_POINT('Ctrl Pts',(4.85068927007173,-5.66898425424195,-8.40164026752836));
#22450=CARTESIAN_POINT('Ctrl Pts',(-1.51301075899711E-11,-5.49398425424197,
-8.40164026751963));
#22451=CARTESIAN_POINT('Ctrl Pts',(-4.85068927010199,-5.31898425424197,
-8.4016402675109));
#22452=CARTESIAN_POINT('Ctrl Pts',(-7.27603390513785,-5.14398425424195,
-4.20082013374671));
#22453=CARTESIAN_POINT('Ctrl Pts',(-9.70137854017372,-4.96898425424197,
1.74701493417668E-11));
#22454=CARTESIAN_POINT('Ctrl Pts',(-7.27603390512272,-4.79398425424196,
4.20082013377292));
#22455=CARTESIAN_POINT('Ctrl Pts',(-4.85068927007173,-4.61898425424196,
8.40164026752836));
#22456=CARTESIAN_POINT('Ctrl Pts',(1.5129078685785E-11,-4.44398425424197,
8.40164026751963));
#22457=CARTESIAN_POINT('Ctrl Pts',(4.85068927010198,-4.26898425424197,8.4016402675109));
#22458=CARTESIAN_POINT('Ctrl Pts',(7.27603390513785,-4.09398425424196,4.20082013374672));
#22459=CARTESIAN_POINT('Ctrl Pts',(9.70137854017372,-3.91898425424198,-1.74689612655491E-11));
#22460=CARTESIAN_POINT('Ctrl Pts',(7.27603390512273,-3.74398425424197,-4.20082013377291));
#22461=CARTESIAN_POINT('Ctrl Pts',(4.85068927007173,-3.56898425424196,-8.40164026752836));
#22462=CARTESIAN_POINT('Ctrl Pts',(-1.51301075899711E-11,-3.39398425424198,
-8.40164026751963));
#22463=CARTESIAN_POINT('Ctrl Pts',(-4.85068927010199,-3.21898425424198,
-8.4016402675109));
#22464=CARTESIAN_POINT('Ctrl Pts',(-7.27603390513785,-3.04398425424196,
-4.20082013374671));
#22465=CARTESIAN_POINT('Ctrl Pts',(-9.70137854017372,-2.86898425424196,
1.74701493417668E-11));
#22466=CARTESIAN_POINT('Ctrl Pts',(-7.27603390512272,-2.69398425424197,
4.20082013377292));
#22467=CARTESIAN_POINT('Ctrl Pts',(-4.85068927007173,-2.51898425424196,
8.40164026752836));
#22468=CARTESIAN_POINT('Ctrl Pts',(1.5129078685785E-11,-2.34398425424195,
8.40164026751963));
#22469=CARTESIAN_POINT('Ctrl Pts',(4.85068927010198,-2.16898425424197,8.4016402675109));
#22470=CARTESIAN_POINT('Ctrl Pts',(7.27603390513785,-1.99398425424197,4.20082013374672));
#22471=CARTESIAN_POINT('Ctrl Pts',(9.70137854017372,-1.81898425424196,-1.74689612655491E-11));
#22472=CARTESIAN_POINT('Ctrl Pts',(7.27603390512273,-1.64398425424198,-4.20082013377291));
#22473=CARTESIAN_POINT('Ctrl Pts',(4.85068927007173,-1.46898425424197,-8.40164026752836));
#22474=CARTESIAN_POINT('Ctrl Pts',(-1.51301075899711E-11,-1.29398425424196,
-8.40164026751963));
#22475=CARTESIAN_POINT('Ctrl Pts',(-4.85068927010199,-1.11898425424198,
-8.4016402675109));
#22476=CARTESIAN_POINT('Ctrl Pts',(-7.27603390513785,-0.94398425424197,
-4.20082013374671));
#22477=CARTESIAN_POINT('Ctrl Pts',(-9.70137854017372,-0.768984254241965,
1.74701493417668E-11));
#22478=CARTESIAN_POINT('Ctrl Pts',(-7.27603390512272,-0.59398425424198,
4.20082013377292));
#22479=CARTESIAN_POINT('Ctrl Pts',(-4.85068927007173,-0.418984254241974,
8.40164026752836));
#22480=CARTESIAN_POINT('Ctrl Pts',(1.5129078685785E-11,-0.243984254241963,
8.40164026751963));
#22481=CARTESIAN_POINT('Ctrl Pts',(4.85068927010198,-0.068984254241984,
8.4016402675109));
#22482=CARTESIAN_POINT('Ctrl Pts',(7.27603390513785,0.106015745758026,4.20082013374672));
#22483=CARTESIAN_POINT('Ctrl Pts',(9.70137854017372,0.28101574575803,-1.74689612655491E-11));
#22484=CARTESIAN_POINT('Ctrl Pts',(7.27603390512273,0.456015745758015,-4.20082013377291));
#22485=CARTESIAN_POINT('Ctrl Pts',(4.85068927007173,0.631015745758021,-8.40164026752836));
#22486=CARTESIAN_POINT('Ctrl Pts',(-1.51301075899711E-11,0.806015745758032,
-8.40164026751963));
#22487=CARTESIAN_POINT('Ctrl Pts',(-4.85068927010199,0.981015745758011,
-8.4016402675109));
#22488=CARTESIAN_POINT('Ctrl Pts',(-7.27603390513785,1.15601574575802,-4.20082013374671));
#22489=CARTESIAN_POINT('Ctrl Pts',(-9.70137854017372,1.33101574575803,1.74701493417668E-11));
#22490=CARTESIAN_POINT('Ctrl Pts',(-7.27603390512272,1.50601574575804,4.20082013377292));
#22491=CARTESIAN_POINT('Ctrl Pts',(-4.85068927007173,1.68101574575802,8.40164026752836));
#22492=CARTESIAN_POINT('Ctrl Pts',(1.5129078685785E-11,1.85601574575803,
8.40164026751963));
#22493=CARTESIAN_POINT('Ctrl Pts',(4.85068927010198,2.03101574575803,8.4016402675109));
#22494=CARTESIAN_POINT('Ctrl Pts',(7.27603390513785,2.20601574575802,4.20082013374672));
#22495=CARTESIAN_POINT('Ctrl Pts',(9.70137854017372,2.38101574575802,-1.74689612655491E-11));
#22496=CARTESIAN_POINT('Ctrl Pts',(7.27603390512273,2.55601574575803,-4.20082013377291));
#22497=CARTESIAN_POINT('Ctrl Pts',(4.85068927007173,2.73101574575801,-8.40164026752836));
#22498=CARTESIAN_POINT('Ctrl Pts',(-1.51301075899711E-11,2.90601574575802,
-8.40164026751963));
#22499=CARTESIAN_POINT('Ctrl Pts',(-4.85068927010199,3.08101574575803,-8.4016402675109));
#22500=CARTESIAN_POINT('Ctrl Pts',(-7.27603390513785,3.25601574575801,-4.20082013374671));
#22501=CARTESIAN_POINT('Ctrl Pts',(-9.70137854017372,3.43101574575802,1.74701493417668E-11));
#22502=CARTESIAN_POINT('Ctrl Pts',(-7.27603390512272,3.60601574575803,4.20082013377292));
#22503=CARTESIAN_POINT('Ctrl Pts',(-4.85068927007173,3.78101574575801,8.40164026752836));
#22504=CARTESIAN_POINT('Ctrl Pts',(1.5129078685785E-11,3.95601574575802,
8.40164026751963));
#22505=CARTESIAN_POINT('Ctrl Pts',(4.85068927010198,4.13101574575802,8.4016402675109));
#22506=CARTESIAN_POINT('Ctrl Pts',(7.27603390513785,4.30601574575801,4.20082013374672));
#22507=CARTESIAN_POINT('Ctrl Pts',(9.70137854017372,4.48101574575801,-1.74689612655491E-11));
#22508=CARTESIAN_POINT('Ctrl Pts',(7.27603390512273,4.65601574575802,-4.20082013377291));
#22509=CARTESIAN_POINT('Ctrl Pts',(4.85068927007173,4.831015745758,-8.40164026752836));
#22510=CARTESIAN_POINT('Ctrl Pts',(-1.51301075899711E-11,5.00601574575801,
-8.40164026751963));
#22511=CARTESIAN_POINT('Ctrl Pts',(-4.85068927010199,5.18101574575802,-8.4016402675109));
#22512=CARTESIAN_POINT('Ctrl Pts',(-7.27603390513785,5.356015745758,-4.20082013374671));
#22513=CARTESIAN_POINT('Ctrl Pts',(-9.70137854017372,5.53101574575801,1.74701493417668E-11));
#22514=CARTESIAN_POINT('Ctrl Pts',(-7.27603390512272,5.70601574575802,4.20082013377292));
#22515=CARTESIAN_POINT('Ctrl Pts',(-4.85068927007173,5.881015745758,8.40164026752836));
#22516=CARTESIAN_POINT('Ctrl Pts',(1.5129078685785E-11,6.05601574575801,
8.40164026751963));
#22517=CARTESIAN_POINT('Ctrl Pts',(4.85068927010198,6.23101574575801,8.4016402675109));
#22518=CARTESIAN_POINT('Ctrl Pts',(7.27603390513785,6.40601574575803,4.20082013374672));
#22519=CARTESIAN_POINT('Ctrl Pts',(9.70137854017372,6.581015745758,-1.74689612655491E-11));
#22520=CARTESIAN_POINT('Ctrl Pts',(7.27603390512273,6.75601574575802,-4.20082013377291));
#22521=CARTESIAN_POINT('Ctrl Pts',(4.85068927007173,6.93101574575802,-8.40164026752836));
#22522=CARTESIAN_POINT('Ctrl Pts',(-1.51301075899711E-11,7.106015745758,
-8.40164026751963));
#22523=CARTESIAN_POINT('Ctrl Pts',(-4.85068927010199,7.28101574575801,-8.4016402675109));
#22524=CARTESIAN_POINT('Ctrl Pts',(-7.27603390513785,7.45601574575802,-4.20082013374671));
#22525=CARTESIAN_POINT('Ctrl Pts',(-9.70137854017372,7.631015745758,1.74701493417668E-11));
#22526=CARTESIAN_POINT('Ctrl Pts',(-7.27603390512272,7.80601574575801,4.20082013377292));
#22527=CARTESIAN_POINT('Ctrl Pts',(-4.85068927007173,7.98101574575801,8.40164026752836));
#22528=CARTESIAN_POINT('Ctrl Pts',(1.5129078685785E-11,8.156015745758,8.40164026751963));
#22529=CARTESIAN_POINT('Ctrl Pts',(4.85068927010198,8.331015745758,8.4016402675109));
#22530=CARTESIAN_POINT('Ctrl Pts',(7.27603390513785,8.50601574575802,4.20082013374672));
#22531=CARTESIAN_POINT('Ctrl Pts',(9.70137854017372,8.68101574575799,-1.74689612655491E-11));
#22532=CARTESIAN_POINT('Ctrl Pts',(7.27603390512273,8.85601574575801,-4.20082013377291));
#22533=CARTESIAN_POINT('Ctrl Pts',(4.85068927007173,9.03101574575801,-8.40164026752836));
#22534=CARTESIAN_POINT('Ctrl Pts',(-1.51301075899711E-11,9.20601574575799,
-8.40164026751963));
#22535=CARTESIAN_POINT('Ctrl Pts',(-4.85068927010199,9.381015745758,-8.4016402675109));
#22536=CARTESIAN_POINT('Ctrl Pts',(-7.27603390513785,9.55601574575801,-4.20082013374671));
#22537=CARTESIAN_POINT('Ctrl Pts',(-9.70137854017372,9.73101574575799,1.74701493417668E-11));
#22538=CARTESIAN_POINT('Ctrl Pts',(-7.27603390512272,9.906015745758,4.20082013377292));
#22539=CARTESIAN_POINT('Ctrl Pts',(-4.85068927007173,10.081015745758,8.40164026752836));
#22540=CARTESIAN_POINT('Ctrl Pts',(1.5129078685785E-11,10.256015745758,
8.40164026751963));
#22541=CARTESIAN_POINT('Ctrl Pts',(4.85068927010198,10.431015745758,8.4016402675109));
#22542=CARTESIAN_POINT('Ctrl Pts',(7.27603390513785,10.606015745758,4.20082013374672));
#22543=CARTESIAN_POINT('Ctrl Pts',(9.70137854017372,10.781015745758,-1.74689612655491E-11));
#22544=CARTESIAN_POINT('Ctrl Pts',(7.27603390512273,10.956015745758,-4.20082013377291));
#22545=CARTESIAN_POINT('Ctrl Pts',(4.85068927007173,11.131015745758,-8.40164026752836));
#22546=CARTESIAN_POINT('Ctrl Pts',(-1.51301075899711E-11,11.306015745758,
-8.40164026751963));
#22547=CARTESIAN_POINT('Ctrl Pts',(-4.85068927010199,11.481015745758,-8.4016402675109));
#22548=CARTESIAN_POINT('Ctrl Pts',(-7.27603390513785,11.656015745758,-4.20082013374671));
#22549=CARTESIAN_POINT('Ctrl Pts',(-9.70137854017372,11.831015745758,1.74701493417668E-11));
#22550=CARTESIAN_POINT('Ctrl Pts',(-7.27603390512272,12.006015745758,4.20082013377292));
#22551=CARTESIAN_POINT('Ctrl Pts',(-4.85068927007173,12.181015745758,8.40164026752836));
#22552=CARTESIAN_POINT('Ctrl Pts',(1.5129078685785E-11,12.356015745758,
8.40164026751963));
#22553=CARTESIAN_POINT('Ctrl Pts',(4.85068927010198,12.531015745758,8.4016402675109));
#22554=CARTESIAN_POINT('Ctrl Pts',(7.27603390513785,12.706015745758,4.20082013374672));
#22555=CARTESIAN_POINT('Ctrl Pts',(9.70137854017372,12.881015745758,-1.74689612655491E-11));
#22556=CARTESIAN_POINT('Ctrl Pts',(7.27603390512273,13.056015745758,-4.20082013377291));
#22557=CARTESIAN_POINT('Ctrl Pts',(4.85068927007173,13.231015745758,-8.40164026752836));
#22558=CARTESIAN_POINT('Ctrl Pts',(-1.51301075899711E-11,13.406015745758,
-8.40164026751963));
#22559=CARTESIAN_POINT('Ctrl Pts',(-4.85068927010199,13.581015745758,-8.4016402675109));
#22560=CARTESIAN_POINT('Ctrl Pts',(-7.27603390513785,13.756015745758,-4.20082013374671));
#22561=CARTESIAN_POINT('Ctrl Pts',(-9.70137854017372,13.931015745758,1.74701493417668E-11));
#22562=CARTESIAN_POINT('Ctrl Pts',(-7.27603390512272,14.106015745758,4.20082013377292));
#22563=CARTESIAN_POINT('Ctrl Pts',(-4.85068927007173,14.281015745758,8.40164026752836));
#22564=CARTESIAN_POINT('Ctrl Pts',(1.5129078685785E-11,14.456015745758,
8.40164026751963));
#22565=CARTESIAN_POINT('Ctrl Pts',(4.85068927010198,14.631015745758,8.4016402675109));
#22566=CARTESIAN_POINT('Ctrl Pts',(7.27603390513785,14.806015745758,4.20082013374672));
#22567=CARTESIAN_POINT('Ctrl Pts',(9.70137854017372,14.981015745758,-1.74689612655491E-11));
#22568=CARTESIAN_POINT('Ctrl Pts',(7.27603390512273,15.156015745758,-4.20082013377291));
#22569=CARTESIAN_POINT('Ctrl Pts',(4.85068927007173,15.331015745758,-8.40164026752836));
#22570=CARTESIAN_POINT('Ctrl Pts',(-1.51301075899711E-11,15.506015745758,
-8.40164026751963));
#22571=CARTESIAN_POINT('Ctrl Pts',(-4.85068927010199,15.681015745758,-8.4016402675109));
#22572=CARTESIAN_POINT('Ctrl Pts',(-7.27603390513785,15.856015745758,-4.20082013374671));
#22573=CARTESIAN_POINT('Ctrl Pts',(-9.70137854017372,16.031015745758,1.74701493417668E-11));
#22574=CARTESIAN_POINT('Ctrl Pts',(-7.27603390512272,16.206015745758,4.20082013377292));
#22575=CARTESIAN_POINT('Ctrl Pts',(-4.85068927007173,16.381015745758,8.40164026752836));
#22576=CARTESIAN_POINT('Ctrl Pts',(1.5129078685785E-11,16.556015745758,
8.40164026751963));
#22577=CARTESIAN_POINT('Ctrl Pts',(4.85068927010198,16.731015745758,8.4016402675109));
#22578=CARTESIAN_POINT('Ctrl Pts',(7.27603390513785,16.906015745758,4.20082013374672));
#22579=CARTESIAN_POINT('Ctrl Pts',(9.70137854017372,17.081015745758,-1.74689612655491E-11));
#22580=CARTESIAN_POINT('Ctrl Pts',(7.27603390512273,17.256015745758,-4.20082013377291));
#22581=CARTESIAN_POINT('Ctrl Pts',(4.85068927007173,17.431015745758,-8.40164026752836));
#22582=CARTESIAN_POINT('Ctrl Pts',(-1.51301075899711E-11,17.606015745758,
-8.40164026751963));
#22583=CARTESIAN_POINT('Ctrl Pts',(-4.85068927010199,17.781015745758,-8.4016402675109));
#22584=CARTESIAN_POINT('Ctrl Pts',(-7.27603390513785,17.956015745758,-4.20082013374671));
#22585=CARTESIAN_POINT('Ctrl Pts',(-9.70137854017372,18.131015745758,1.74701493417668E-11));
#22586=CARTESIAN_POINT('Ctrl Pts',(-7.27603390512272,18.306015745758,4.20082013377292));
#22587=CARTESIAN_POINT('Ctrl Pts',(-4.85068927007173,18.481015745758,8.40164026752836));
#22588=CARTESIAN_POINT('Ctrl Pts',(1.5129078685785E-11,18.656015745758,
8.40164026751963));
#22589=CARTESIAN_POINT('Ctrl Pts',(4.85068927010198,18.831015745758,8.4016402675109));
#22590=CARTESIAN_POINT('Ctrl Pts',(7.27603390513785,19.006015745758,4.20082013374672));
#22591=CARTESIAN_POINT('Ctrl Pts',(9.70137854017372,19.181015745758,-1.74689612655491E-11));
#22592=CARTESIAN_POINT('Ctrl Pts',(7.27603390512273,19.356015745758,-4.20082013377291));
#22593=CARTESIAN_POINT('Ctrl Pts',(4.85068927007173,19.531015745758,-8.40164026752836));
#22594=CARTESIAN_POINT('Ctrl Pts',(-1.51301075899711E-11,19.706015745758,
-8.40164026751963));
#22595=CARTESIAN_POINT('Ctrl Pts',(-4.85068927010199,19.881015745758,-8.4016402675109));
#22596=CARTESIAN_POINT('Ctrl Pts',(-7.27603390513785,20.056015745758,-4.20082013374671));
#22597=CARTESIAN_POINT('Ctrl Pts',(-9.70137854017372,20.231015745758,1.74701493417668E-11));
#22598=CARTESIAN_POINT('Ctrl Pts',(-7.27603390512272,20.406015745758,4.20082013377292));
#22599=CARTESIAN_POINT('Ctrl Pts',(-4.85068927007173,20.581015745758,8.40164026752836));
#22600=CARTESIAN_POINT('Ctrl Pts',(1.5129078685785E-11,20.756015745758,
8.40164026751963));
#22601=CARTESIAN_POINT('Ctrl Pts',(4.85068927010198,20.931015745758,8.4016402675109));
#22602=CARTESIAN_POINT('Ctrl Pts',(7.27603390513785,21.106015745758,4.20082013374672));
#22603=CARTESIAN_POINT('Ctrl Pts',(9.70137854017372,21.281015745758,-1.74689612655491E-11));
#22604=CARTESIAN_POINT('Ctrl Pts',(7.27603390512273,21.456015745758,-4.20082013377291));
#22605=CARTESIAN_POINT('Ctrl Pts',(4.85068927007173,21.631015745758,-8.40164026752836));
#22606=CARTESIAN_POINT('Ctrl Pts',(-1.51301075899711E-11,21.806015745758,
-8.40164026751963));
#22607=CARTESIAN_POINT('Ctrl Pts',(-4.85068927010199,21.981015745758,-8.4016402675109));
#22608=CARTESIAN_POINT('Ctrl Pts',(-7.27603390513785,22.156015745758,-4.20082013374671));
#22609=CARTESIAN_POINT('Ctrl Pts',(-9.70137854017372,22.331015745758,1.74701493417668E-11));
#22610=CARTESIAN_POINT('Ctrl Pts',(-7.27603390512272,22.506015745758,4.20082013377292));
#22611=CARTESIAN_POINT('Ctrl Pts',(-4.85068927007173,22.681015745758,8.40164026752836));
#22612=CARTESIAN_POINT('Ctrl Pts',(1.5129078685785E-11,22.856015745758,
8.40164026751963));
#22613=CARTESIAN_POINT('Ctrl Pts',(4.85068927010198,23.031015745758,8.4016402675109));
#22614=CARTESIAN_POINT('Ctrl Pts',(7.27603390513785,23.206015745758,4.20082013374672));
#22615=CARTESIAN_POINT('Ctrl Pts',(9.70137854017372,23.381015745758,-1.74689612655491E-11));
#22616=CARTESIAN_POINT('Ctrl Pts',(7.27603390512273,23.556015745758,-4.20082013377291));
#22617=CARTESIAN_POINT('Ctrl Pts',(4.85068927007173,23.731015745758,-8.40164026752836));
#22618=CARTESIAN_POINT('Ctrl Pts',(-1.51301075899711E-11,23.906015745758,
-8.40164026751963));
#22619=CARTESIAN_POINT('Ctrl Pts',(-4.85068927010199,24.081015745758,-8.4016402675109));
#22620=CARTESIAN_POINT('Ctrl Pts',(-7.27603390513785,24.256015745758,-4.20082013374671));
#22621=CARTESIAN_POINT('Ctrl Pts',(-9.70137854017372,24.431015745758,1.74701493417668E-11));
#22622=CARTESIAN_POINT('Ctrl Pts',(-7.27603390512272,24.606015745758,4.20082013377292));
#22623=CARTESIAN_POINT('Ctrl Pts',(-4.85068927007173,24.781015745758,8.40164026752836));
#22624=CARTESIAN_POINT('Ctrl Pts',(1.5129078685785E-11,24.956015745758,
8.40164026751963));
#22625=CARTESIAN_POINT('Ctrl Pts',(4.85068927010198,25.131015745758,8.4016402675109));
#22626=CARTESIAN_POINT('Ctrl Pts',(7.27603390513785,25.306015745758,4.20082013374672));
#22627=CARTESIAN_POINT('Ctrl Pts',(9.70137854017372,25.481015745758,-1.74689612655491E-11));
#22628=CARTESIAN_POINT('Ctrl Pts',(7.27603390512273,25.656015745758,-4.20082013377291));
#22629=CARTESIAN_POINT('Ctrl Pts',(4.85068927007173,25.831015745758,-8.40164026752836));
#22630=CARTESIAN_POINT('Ctrl Pts',(-1.51301075899711E-11,26.006015745758,
-8.40164026751963));
#22631=CARTESIAN_POINT('Ctrl Pts',(-1.4702867290402E-11,-143.970483118095,
-8.16439679232146));
#22632=CARTESIAN_POINT('Ctrl Pts',(-4.71371668583241,-143.795483118095,
-8.16439679231297));
#22633=CARTESIAN_POINT('Ctrl Pts',(-7.07057502873392,-143.620483118095,
-4.082198396148));
#22634=CARTESIAN_POINT('Ctrl Pts',(-9.42743337163542,-143.445483118095,
1.69768315121407E-11));
#22635=CARTESIAN_POINT('Ctrl Pts',(-7.07057502871922,-143.270483118095,
4.08219839617346));
#22636=CARTESIAN_POINT('Ctrl Pts',(-4.71371668580301,-143.095483118095,
8.16439679232994));
#22637=CARTESIAN_POINT('Ctrl Pts',(1.47018674401621E-11,-142.920483118095,
8.16439679232146));
#22638=CARTESIAN_POINT('Ctrl Pts',(4.71371668583241,-142.745483118095,8.16439679231297));
#22639=CARTESIAN_POINT('Ctrl Pts',(7.07057502873392,-142.570483118095,4.082198396148));
#22640=CARTESIAN_POINT('Ctrl Pts',(9.42743337163542,-142.395483118095,-1.69756769845304E-11));
#22641=CARTESIAN_POINT('Ctrl Pts',(7.07057502871922,-142.220483118095,-4.08219839617346));
#22642=CARTESIAN_POINT('Ctrl Pts',(4.71371668580301,-142.045483118095,-8.16439679232994));
#22643=CARTESIAN_POINT('Ctrl Pts',(-1.4702867290402E-11,-141.870483118095,
-8.16439679232146));
#22644=CARTESIAN_POINT('Ctrl Pts',(-4.71371668583241,-141.695483118095,
-8.16439679231297));
#22645=CARTESIAN_POINT('Ctrl Pts',(-7.07057502873392,-141.520483118095,
-4.082198396148));
#22646=CARTESIAN_POINT('Ctrl Pts',(-9.42743337163542,-141.345483118095,
1.69768315121407E-11));
#22647=CARTESIAN_POINT('Ctrl Pts',(-7.07057502871922,-141.170483118095,
4.08219839617346));
#22648=CARTESIAN_POINT('Ctrl Pts',(-4.71371668580301,-140.995483118095,
8.16439679232994));
#22649=CARTESIAN_POINT('Ctrl Pts',(1.47018674401621E-11,-140.820483118095,
8.16439679232146));
#22650=CARTESIAN_POINT('Ctrl Pts',(4.71371668583241,-140.645483118095,8.16439679231297));
#22651=CARTESIAN_POINT('Ctrl Pts',(7.07057502873392,-140.470483118095,4.082198396148));
#22652=CARTESIAN_POINT('Ctrl Pts',(9.42743337163542,-140.295483118095,-1.69756769845304E-11));
#22653=CARTESIAN_POINT('Ctrl Pts',(7.07057502871922,-140.120483118095,-4.08219839617346));
#22654=CARTESIAN_POINT('Ctrl Pts',(4.71371668580301,-139.945483118095,-8.16439679232994));
#22655=CARTESIAN_POINT('Ctrl Pts',(-1.4702867290402E-11,-139.770483118095,
-8.16439679232146));
#22656=CARTESIAN_POINT('Ctrl Pts',(-4.71371668583241,-139.595483118095,
-8.16439679231297));
#22657=CARTESIAN_POINT('Ctrl Pts',(-7.07057502873392,-139.420483118095,
-4.082198396148));
#22658=CARTESIAN_POINT('Ctrl Pts',(-9.42743337163542,-139.245483118095,
1.69768315121407E-11));
#22659=CARTESIAN_POINT('Ctrl Pts',(-7.07057502871922,-139.070483118095,
4.08219839617346));
#22660=CARTESIAN_POINT('Ctrl Pts',(-4.71371668580301,-138.895483118095,
8.16439679232994));
#22661=CARTESIAN_POINT('Ctrl Pts',(1.47018674401621E-11,-138.720483118095,
8.16439679232146));
#22662=CARTESIAN_POINT('Ctrl Pts',(4.71371668583241,-138.545483118095,8.16439679231297));
#22663=CARTESIAN_POINT('Ctrl Pts',(7.07057502873392,-138.370483118095,4.082198396148));
#22664=CARTESIAN_POINT('Ctrl Pts',(9.42743337163542,-138.195483118095,-1.69756769845304E-11));
#22665=CARTESIAN_POINT('Ctrl Pts',(7.07057502871922,-138.020483118095,-4.08219839617346));
#22666=CARTESIAN_POINT('Ctrl Pts',(4.71371668580301,-137.845483118095,-8.16439679232994));
#22667=CARTESIAN_POINT('Ctrl Pts',(-1.4702867290402E-11,-137.670483118095,
-8.16439679232146));
#22668=CARTESIAN_POINT('Ctrl Pts',(-4.71371668583241,-137.495483118095,
-8.16439679231297));
#22669=CARTESIAN_POINT('Ctrl Pts',(-7.07057502873392,-137.320483118095,
-4.082198396148));
#22670=CARTESIAN_POINT('Ctrl Pts',(-9.42743337163542,-137.145483118095,
1.69768315121407E-11));
#22671=CARTESIAN_POINT('Ctrl Pts',(-7.07057502871922,-136.970483118095,
4.08219839617346));
#22672=CARTESIAN_POINT('Ctrl Pts',(-4.71371668580301,-136.795483118095,
8.16439679232994));
#22673=CARTESIAN_POINT('Ctrl Pts',(1.47018674401621E-11,-136.620483118095,
8.16439679232146));
#22674=CARTESIAN_POINT('Ctrl Pts',(4.71371668583241,-136.445483118095,8.16439679231297));
#22675=CARTESIAN_POINT('Ctrl Pts',(7.07057502873392,-136.270483118095,4.082198396148));
#22676=CARTESIAN_POINT('Ctrl Pts',(9.42743337163542,-136.095483118095,-1.69756769845304E-11));
#22677=CARTESIAN_POINT('Ctrl Pts',(7.07057502871922,-135.920483118095,-4.08219839617346));
#22678=CARTESIAN_POINT('Ctrl Pts',(4.71371668580301,-135.745483118095,-8.16439679232994));
#22679=CARTESIAN_POINT('Ctrl Pts',(-1.4702867290402E-11,-135.570483118095,
-8.16439679232146));
#22680=CARTESIAN_POINT('Ctrl Pts',(-4.71371668583241,-135.395483118095,
-8.16439679231297));
#22681=CARTESIAN_POINT('Ctrl Pts',(-7.07057502873392,-135.220483118095,
-4.082198396148));
#22682=CARTESIAN_POINT('Ctrl Pts',(-9.42743337163542,-135.045483118095,
1.69768315121407E-11));
#22683=CARTESIAN_POINT('Ctrl Pts',(-7.07057502871922,-134.870483118095,
4.08219839617346));
#22684=CARTESIAN_POINT('Ctrl Pts',(-4.71371668580301,-134.695483118095,
8.16439679232994));
#22685=CARTESIAN_POINT('Ctrl Pts',(1.47018674401621E-11,-134.520483118095,
8.16439679232146));
#22686=CARTESIAN_POINT('Ctrl Pts',(4.71371668583241,-134.345483118095,8.16439679231297));
#22687=CARTESIAN_POINT('Ctrl Pts',(7.07057502873392,-134.170483118095,4.082198396148));
#22688=CARTESIAN_POINT('Ctrl Pts',(9.42743337163542,-133.995483118095,-1.69756769845304E-11));
#22689=CARTESIAN_POINT('Ctrl Pts',(7.07057502871922,-133.820483118095,-4.08219839617346));
#22690=CARTESIAN_POINT('Ctrl Pts',(4.71371668580301,-133.645483118095,-8.16439679232994));
#22691=CARTESIAN_POINT('Ctrl Pts',(-1.4702867290402E-11,-133.470483118095,
-8.16439679232146));
#22692=CARTESIAN_POINT('Ctrl Pts',(-4.71371668583241,-133.295483118095,
-8.16439679231297));
#22693=CARTESIAN_POINT('Ctrl Pts',(-7.07057502873392,-133.120483118095,
-4.082198396148));
#22694=CARTESIAN_POINT('Ctrl Pts',(-9.42743337163542,-132.945483118095,
1.69768315121407E-11));
#22695=CARTESIAN_POINT('Ctrl Pts',(-7.07057502871922,-132.770483118095,
4.08219839617346));
#22696=CARTESIAN_POINT('Ctrl Pts',(-4.71371668580301,-132.595483118095,
8.16439679232994));
#22697=CARTESIAN_POINT('Ctrl Pts',(1.47018674401621E-11,-132.420483118095,
8.16439679232146));
#22698=CARTESIAN_POINT('Ctrl Pts',(4.71371668583241,-132.245483118095,8.16439679231297));
#22699=CARTESIAN_POINT('Ctrl Pts',(7.07057502873392,-132.070483118095,4.082198396148));
#22700=CARTESIAN_POINT('Ctrl Pts',(9.42743337163542,-131.895483118095,-1.69756769845304E-11));
#22701=CARTESIAN_POINT('Ctrl Pts',(7.07057502871922,-131.720483118095,-4.08219839617346));
#22702=CARTESIAN_POINT('Ctrl Pts',(4.71371668580301,-131.545483118095,-8.16439679232994));
#22703=CARTESIAN_POINT('Ctrl Pts',(-1.4702867290402E-11,-131.370483118095,
-8.16439679232146));
#22704=CARTESIAN_POINT('Ctrl Pts',(-4.71371668583241,-131.195483118095,
-8.16439679231297));
#22705=CARTESIAN_POINT('Ctrl Pts',(-7.07057502873392,-131.020483118095,
-4.082198396148));
#22706=CARTESIAN_POINT('Ctrl Pts',(-9.42743337163542,-130.845483118095,
1.69768315121407E-11));
#22707=CARTESIAN_POINT('Ctrl Pts',(-7.07057502871922,-130.670483118095,
4.08219839617346));
#22708=CARTESIAN_POINT('Ctrl Pts',(-4.71371668580301,-130.495483118095,
8.16439679232994));
#22709=CARTESIAN_POINT('Ctrl Pts',(1.47018674401621E-11,-130.320483118095,
8.16439679232146));
#22710=CARTESIAN_POINT('Ctrl Pts',(4.71371668583241,-130.145483118095,8.16439679231297));
#22711=CARTESIAN_POINT('Ctrl Pts',(7.07057502873392,-129.970483118095,4.082198396148));
#22712=CARTESIAN_POINT('Ctrl Pts',(9.42743337163542,-129.795483118095,-1.69756769845304E-11));
#22713=CARTESIAN_POINT('Ctrl Pts',(7.07057502871922,-129.620483118095,-4.08219839617346));
#22714=CARTESIAN_POINT('Ctrl Pts',(4.71371668580301,-129.445483118095,-8.16439679232994));
#22715=CARTESIAN_POINT('Ctrl Pts',(-1.4702867290402E-11,-129.270483118095,
-8.16439679232146));
#22716=CARTESIAN_POINT('Ctrl Pts',(-4.71371668583241,-129.095483118095,
-8.16439679231297));
#22717=CARTESIAN_POINT('Ctrl Pts',(-7.07057502873392,-128.920483118095,
-4.082198396148));
#22718=CARTESIAN_POINT('Ctrl Pts',(-9.42743337163542,-128.745483118095,
1.69768315121407E-11));
#22719=CARTESIAN_POINT('Ctrl Pts',(-7.07057502871922,-128.570483118095,
4.08219839617346));
#22720=CARTESIAN_POINT('Ctrl Pts',(-4.71371668580301,-128.395483118095,
8.16439679232994));
#22721=CARTESIAN_POINT('Ctrl Pts',(1.47018674401621E-11,-128.220483118095,
8.16439679232146));
#22722=CARTESIAN_POINT('Ctrl Pts',(4.71371668583241,-128.045483118095,8.16439679231297));
#22723=CARTESIAN_POINT('Ctrl Pts',(7.07057502873392,-127.870483118095,4.082198396148));
#22724=CARTESIAN_POINT('Ctrl Pts',(9.42743337163542,-127.695483118095,-1.69756769845304E-11));
#22725=CARTESIAN_POINT('Ctrl Pts',(7.07057502871922,-127.520483118095,-4.08219839617346));
#22726=CARTESIAN_POINT('Ctrl Pts',(4.71371668580301,-127.345483118095,-8.16439679232994));
#22727=CARTESIAN_POINT('Ctrl Pts',(-1.4702867290402E-11,-127.170483118095,
-8.16439679232146));
#22728=CARTESIAN_POINT('Ctrl Pts',(-4.71371668583241,-126.995483118095,
-8.16439679231297));
#22729=CARTESIAN_POINT('Ctrl Pts',(-7.07057502873392,-126.820483118095,
-4.082198396148));
#22730=CARTESIAN_POINT('Ctrl Pts',(-9.42743337163542,-126.645483118095,
1.69768315121407E-11));
#22731=CARTESIAN_POINT('Ctrl Pts',(-7.07057502871922,-126.470483118095,
4.08219839617346));
#22732=CARTESIAN_POINT('Ctrl Pts',(-4.71371668580301,-126.295483118095,
8.16439679232994));
#22733=CARTESIAN_POINT('Ctrl Pts',(1.47018674401621E-11,-126.120483118095,
8.16439679232146));
#22734=CARTESIAN_POINT('Ctrl Pts',(4.71371668583241,-125.945483118095,8.16439679231297));
#22735=CARTESIAN_POINT('Ctrl Pts',(7.07057502873392,-125.770483118095,4.082198396148));
#22736=CARTESIAN_POINT('Ctrl Pts',(9.42743337163542,-125.595483118095,-1.69756769845304E-11));
#22737=CARTESIAN_POINT('Ctrl Pts',(7.07057502871922,-125.420483118095,-4.08219839617346));
#22738=CARTESIAN_POINT('Ctrl Pts',(4.71371668580301,-125.245483118095,-8.16439679232994));
#22739=CARTESIAN_POINT('Ctrl Pts',(-1.4702867290402E-11,-125.070483118095,
-8.16439679232146));
#22740=CARTESIAN_POINT('Ctrl Pts',(-4.71371668583241,-124.895483118095,
-8.16439679231297));
#22741=CARTESIAN_POINT('Ctrl Pts',(-7.07057502873392,-124.720483118095,
-4.082198396148));
#22742=CARTESIAN_POINT('Ctrl Pts',(-9.42743337163542,-124.545483118095,
1.69768315121407E-11));
#22743=CARTESIAN_POINT('Ctrl Pts',(-7.07057502871922,-124.370483118095,
4.08219839617346));
#22744=CARTESIAN_POINT('Ctrl Pts',(-4.71371668580301,-124.195483118095,
8.16439679232994));
#22745=CARTESIAN_POINT('Ctrl Pts',(1.47018674401621E-11,-124.020483118095,
8.16439679232146));
#22746=CARTESIAN_POINT('Ctrl Pts',(4.71371668583241,-123.845483118095,8.16439679231297));
#22747=CARTESIAN_POINT('Ctrl Pts',(7.07057502873392,-123.670483118095,4.082198396148));
#22748=CARTESIAN_POINT('Ctrl Pts',(9.42743337163542,-123.495483118095,-1.69756769845304E-11));
#22749=CARTESIAN_POINT('Ctrl Pts',(7.07057502871922,-123.320483118095,-4.08219839617346));
#22750=CARTESIAN_POINT('Ctrl Pts',(4.71371668580301,-123.145483118095,-8.16439679232994));
#22751=CARTESIAN_POINT('Ctrl Pts',(-1.4702867290402E-11,-122.970483118095,
-8.16439679232146));
#22752=CARTESIAN_POINT('Ctrl Pts',(-4.71371668583241,-122.795483118095,
-8.16439679231297));
#22753=CARTESIAN_POINT('Ctrl Pts',(-7.07057502873392,-122.620483118095,
-4.082198396148));
#22754=CARTESIAN_POINT('Ctrl Pts',(-9.42743337163542,-122.445483118095,
1.69768315121407E-11));
#22755=CARTESIAN_POINT('Ctrl Pts',(-7.07057502871922,-122.270483118095,
4.08219839617346));
#22756=CARTESIAN_POINT('Ctrl Pts',(-4.71371668580301,-122.095483118095,
8.16439679232994));
#22757=CARTESIAN_POINT('Ctrl Pts',(1.47018674401621E-11,-121.920483118095,
8.16439679232146));
#22758=CARTESIAN_POINT('Ctrl Pts',(4.71371668583241,-121.745483118095,8.16439679231297));
#22759=CARTESIAN_POINT('Ctrl Pts',(7.07057502873392,-121.570483118095,4.082198396148));
#22760=CARTESIAN_POINT('Ctrl Pts',(9.42743337163542,-121.395483118095,-1.69756769845304E-11));
#22761=CARTESIAN_POINT('Ctrl Pts',(7.07057502871922,-121.220483118095,-4.08219839617346));
#22762=CARTESIAN_POINT('Ctrl Pts',(4.71371668580301,-121.045483118095,-8.16439679232994));
#22763=CARTESIAN_POINT('Ctrl Pts',(-1.4702867290402E-11,-120.870483118095,
-8.16439679232146));
#22764=CARTESIAN_POINT('Ctrl Pts',(-4.71371668583241,-120.695483118095,
-8.16439679231297));
#22765=CARTESIAN_POINT('Ctrl Pts',(-7.07057502873392,-120.520483118095,
-4.082198396148));
#22766=CARTESIAN_POINT('Ctrl Pts',(-9.42743337163542,-120.345483118095,
1.69768315121407E-11));
#22767=CARTESIAN_POINT('Ctrl Pts',(-7.07057502871922,-120.170483118095,
4.08219839617346));
#22768=CARTESIAN_POINT('Ctrl Pts',(-4.71371668580301,-119.995483118095,
8.16439679232994));
#22769=CARTESIAN_POINT('Ctrl Pts',(1.47018674401621E-11,-119.820483118095,
8.16439679232146));
#22770=CARTESIAN_POINT('Ctrl Pts',(4.71371668583241,-119.645483118095,8.16439679231297));
#22771=CARTESIAN_POINT('Ctrl Pts',(7.07057502873392,-119.470483118095,4.082198396148));
#22772=CARTESIAN_POINT('Ctrl Pts',(9.42743337163542,-119.295483118095,-1.69756769845304E-11));
#22773=CARTESIAN_POINT('Ctrl Pts',(7.07057502871922,-119.120483118095,-4.08219839617346));
#22774=CARTESIAN_POINT('Ctrl Pts',(4.71371668580301,-118.945483118095,-8.16439679232994));
#22775=CARTESIAN_POINT('Ctrl Pts',(-1.4702867290402E-11,-118.770483118095,
-8.16439679232146));
#22776=CARTESIAN_POINT('Ctrl Pts',(-4.71371668583241,-118.595483118095,
-8.16439679231297));
#22777=CARTESIAN_POINT('Ctrl Pts',(-7.07057502873392,-118.420483118095,
-4.082198396148));
#22778=CARTESIAN_POINT('Ctrl Pts',(-9.42743337163542,-118.245483118095,
1.69768315121407E-11));
#22779=CARTESIAN_POINT('Ctrl Pts',(-7.07057502871922,-118.070483118095,
4.08219839617346));
#22780=CARTESIAN_POINT('Ctrl Pts',(-4.71371668580301,-117.895483118095,
8.16439679232994));
#22781=CARTESIAN_POINT('Ctrl Pts',(1.47018674401621E-11,-117.720483118095,
8.16439679232146));
#22782=CARTESIAN_POINT('Ctrl Pts',(4.71371668583241,-117.545483118095,8.16439679231297));
#22783=CARTESIAN_POINT('Ctrl Pts',(7.07057502873392,-117.370483118095,4.082198396148));
#22784=CARTESIAN_POINT('Ctrl Pts',(9.42743337163542,-117.195483118095,-1.69756769845304E-11));
#22785=CARTESIAN_POINT('Ctrl Pts',(7.07057502871922,-117.020483118095,-4.08219839617346));
#22786=CARTESIAN_POINT('Ctrl Pts',(4.71371668580301,-116.845483118095,-8.16439679232994));
#22787=CARTESIAN_POINT('Ctrl Pts',(-1.4702867290402E-11,-116.670483118095,
-8.16439679232146));
#22788=CARTESIAN_POINT('Ctrl Pts',(-4.71371668583241,-116.495483118095,
-8.16439679231297));
#22789=CARTESIAN_POINT('Ctrl Pts',(-7.07057502873392,-116.320483118095,
-4.082198396148));
#22790=CARTESIAN_POINT('Ctrl Pts',(-9.42743337163542,-116.145483118095,
1.69768315121407E-11));
#22791=CARTESIAN_POINT('Ctrl Pts',(-7.07057502871922,-115.970483118095,
4.08219839617346));
#22792=CARTESIAN_POINT('Ctrl Pts',(-4.71371668580301,-115.795483118095,
8.16439679232994));
#22793=CARTESIAN_POINT('Ctrl Pts',(1.47018674401621E-11,-115.620483118095,
8.16439679232146));
#22794=CARTESIAN_POINT('Ctrl Pts',(4.71371668583241,-115.445483118095,8.16439679231297));
#22795=CARTESIAN_POINT('Ctrl Pts',(7.07057502873392,-115.270483118095,4.082198396148));
#22796=CARTESIAN_POINT('Ctrl Pts',(9.42743337163542,-115.095483118095,-1.69756769845304E-11));
#22797=CARTESIAN_POINT('Ctrl Pts',(7.07057502871922,-114.920483118095,-4.08219839617346));
#22798=CARTESIAN_POINT('Ctrl Pts',(4.71371668580301,-114.745483118095,-8.16439679232994));
#22799=CARTESIAN_POINT('Ctrl Pts',(-1.4702867290402E-11,-114.570483118095,
-8.16439679232146));
#22800=CARTESIAN_POINT('Ctrl Pts',(-4.71371668583241,-114.395483118095,
-8.16439679231297));
#22801=CARTESIAN_POINT('Ctrl Pts',(-7.07057502873392,-114.220483118095,
-4.082198396148));
#22802=CARTESIAN_POINT('Ctrl Pts',(-9.42743337163542,-114.045483118095,
1.69768315121407E-11));
#22803=CARTESIAN_POINT('Ctrl Pts',(-7.07057502871922,-113.870483118095,
4.08219839617346));
#22804=CARTESIAN_POINT('Ctrl Pts',(-4.71371668580301,-113.695483118095,
8.16439679232994));
#22805=CARTESIAN_POINT('Ctrl Pts',(1.47018674401621E-11,-113.520483118095,
8.16439679232146));
#22806=CARTESIAN_POINT('Ctrl Pts',(4.71371668583241,-113.345483118095,8.16439679231297));
#22807=CARTESIAN_POINT('Ctrl Pts',(7.07057502873392,-113.170483118095,4.082198396148));
#22808=CARTESIAN_POINT('Ctrl Pts',(9.42743337163542,-112.995483118095,-1.69756769845304E-11));
#22809=CARTESIAN_POINT('Ctrl Pts',(7.07057502871922,-112.820483118095,-4.08219839617346));
#22810=CARTESIAN_POINT('Ctrl Pts',(4.71371668580301,-112.645483118095,-8.16439679232994));
#22811=CARTESIAN_POINT('Ctrl Pts',(-1.4702867290402E-11,-112.470483118095,
-8.16439679232146));
#22812=CARTESIAN_POINT('Ctrl Pts',(-4.71371668583241,-112.295483118095,
-8.16439679231297));
#22813=CARTESIAN_POINT('Ctrl Pts',(-7.07057502873392,-112.120483118095,
-4.082198396148));
#22814=CARTESIAN_POINT('Ctrl Pts',(-9.42743337163542,-111.945483118095,
1.69768315121407E-11));
#22815=CARTESIAN_POINT('Ctrl Pts',(-7.07057502871922,-111.770483118095,
4.08219839617346));
#22816=CARTESIAN_POINT('Ctrl Pts',(-4.71371668580301,-111.595483118095,
8.16439679232994));
#22817=CARTESIAN_POINT('Ctrl Pts',(1.47018674401621E-11,-111.420483118095,
8.16439679232146));
#22818=CARTESIAN_POINT('Ctrl Pts',(4.71371668583241,-111.245483118095,8.16439679231297));
#22819=CARTESIAN_POINT('Ctrl Pts',(7.07057502873392,-111.070483118095,4.082198396148));
#22820=CARTESIAN_POINT('Ctrl Pts',(9.42743337163542,-110.895483118095,-1.69756769845304E-11));
#22821=CARTESIAN_POINT('Ctrl Pts',(7.07057502871922,-110.720483118095,-4.08219839617346));
#22822=CARTESIAN_POINT('Ctrl Pts',(4.71371668580301,-110.545483118095,-8.16439679232994));
#22823=CARTESIAN_POINT('Ctrl Pts',(-1.4702867290402E-11,-110.370483118095,
-8.16439679232146));
#22824=CARTESIAN_POINT('Ctrl Pts',(-4.71371668583241,-110.195483118095,
-8.16439679231297));
#22825=CARTESIAN_POINT('Ctrl Pts',(-7.07057502873392,-110.020483118095,
-4.082198396148));
#22826=CARTESIAN_POINT('Ctrl Pts',(-9.42743337163542,-109.845483118095,
1.69768315121407E-11));
#22827=CARTESIAN_POINT('Ctrl Pts',(-7.07057502871922,-109.670483118095,
4.08219839617346));
#22828=CARTESIAN_POINT('Ctrl Pts',(-4.71371668580301,-109.495483118095,
8.16439679232994));
#22829=CARTESIAN_POINT('Ctrl Pts',(1.47018674401621E-11,-109.320483118095,
8.16439679232146));
#22830=CARTESIAN_POINT('Ctrl Pts',(4.71371668583241,-109.145483118095,8.16439679231297));
#22831=CARTESIAN_POINT('Ctrl Pts',(7.07057502873392,-108.970483118095,4.082198396148));
#22832=CARTESIAN_POINT('Ctrl Pts',(9.42743337163542,-108.795483118095,-1.69756769845304E-11));
#22833=CARTESIAN_POINT('Ctrl Pts',(7.07057502871922,-108.620483118095,-4.08219839617346));
#22834=CARTESIAN_POINT('Ctrl Pts',(4.71371668580301,-108.445483118095,-8.16439679232994));
#22835=CARTESIAN_POINT('Ctrl Pts',(-1.4702867290402E-11,-108.270483118095,
-8.16439679232146));
#22836=CARTESIAN_POINT('Ctrl Pts',(-4.71371668583241,-108.095483118095,
-8.16439679231297));
#22837=CARTESIAN_POINT('Ctrl Pts',(-7.07057502873392,-107.920483118095,
-4.082198396148));
#22838=CARTESIAN_POINT('Ctrl Pts',(-9.42743337163542,-107.745483118095,
1.69768315121407E-11));
#22839=CARTESIAN_POINT('Ctrl Pts',(-7.07057502871922,-107.570483118095,
4.08219839617346));
#22840=CARTESIAN_POINT('Ctrl Pts',(-4.71371668580301,-107.395483118095,
8.16439679232994));
#22841=CARTESIAN_POINT('Ctrl Pts',(1.47018674401621E-11,-107.220483118095,
8.16439679232146));
#22842=CARTESIAN_POINT('Ctrl Pts',(4.71371668583241,-107.045483118095,8.16439679231297));
#22843=CARTESIAN_POINT('Ctrl Pts',(7.07057502873392,-106.870483118095,4.082198396148));
#22844=CARTESIAN_POINT('Ctrl Pts',(9.42743337163542,-106.695483118095,-1.69756769845304E-11));
#22845=CARTESIAN_POINT('Ctrl Pts',(7.07057502871922,-106.520483118095,-4.08219839617346));
#22846=CARTESIAN_POINT('Ctrl Pts',(4.71371668580301,-106.345483118095,-8.16439679232994));
#22847=CARTESIAN_POINT('Ctrl Pts',(-1.4702867290402E-11,-106.170483118095,
-8.16439679232146));
#22848=CARTESIAN_POINT('Ctrl Pts',(-4.71371668583241,-105.995483118095,
-8.16439679231297));
#22849=CARTESIAN_POINT('Ctrl Pts',(-7.07057502873392,-105.820483118095,
-4.082198396148));
#22850=CARTESIAN_POINT('Ctrl Pts',(-9.42743337163542,-105.645483118095,
1.69768315121407E-11));
#22851=CARTESIAN_POINT('Ctrl Pts',(-7.07057502871922,-105.470483118095,
4.08219839617346));
#22852=CARTESIAN_POINT('Ctrl Pts',(-4.71371668580301,-105.295483118095,
8.16439679232994));
#22853=CARTESIAN_POINT('Ctrl Pts',(1.47018674401621E-11,-105.120483118095,
8.16439679232146));
#22854=CARTESIAN_POINT('Ctrl Pts',(4.71371668583241,-104.945483118095,8.16439679231297));
#22855=CARTESIAN_POINT('Ctrl Pts',(7.07057502873392,-104.770483118095,4.082198396148));
#22856=CARTESIAN_POINT('Ctrl Pts',(9.42743337163542,-104.595483118095,-1.69756769845304E-11));
#22857=CARTESIAN_POINT('Ctrl Pts',(7.07057502871922,-104.420483118095,-4.08219839617346));
#22858=CARTESIAN_POINT('Ctrl Pts',(4.71371668580301,-104.245483118095,-8.16439679232994));
#22859=CARTESIAN_POINT('Ctrl Pts',(-1.4702867290402E-11,-104.070483118095,
-8.16439679232146));
#22860=CARTESIAN_POINT('Ctrl Pts',(-4.71371668583241,-103.895483118095,
-8.16439679231297));
#22861=CARTESIAN_POINT('Ctrl Pts',(-7.07057502873392,-103.720483118095,
-4.082198396148));
#22862=CARTESIAN_POINT('Ctrl Pts',(-9.42743337163542,-103.545483118095,
1.69768315121407E-11));
#22863=CARTESIAN_POINT('Ctrl Pts',(-7.07057502871922,-103.370483118095,
4.08219839617346));
#22864=CARTESIAN_POINT('Ctrl Pts',(-4.71371668580301,-103.195483118095,
8.16439679232994));
#22865=CARTESIAN_POINT('Ctrl Pts',(1.47018674401621E-11,-103.020483118095,
8.16439679232146));
#22866=CARTESIAN_POINT('Ctrl Pts',(4.71371668583241,-102.845483118095,8.16439679231297));
#22867=CARTESIAN_POINT('Ctrl Pts',(7.07057502873392,-102.670483118095,4.082198396148));
#22868=CARTESIAN_POINT('Ctrl Pts',(9.42743337163542,-102.495483118095,-1.69756769845304E-11));
#22869=CARTESIAN_POINT('Ctrl Pts',(7.07057502871922,-102.320483118095,-4.08219839617346));
#22870=CARTESIAN_POINT('Ctrl Pts',(4.71371668580301,-102.145483118095,-8.16439679232994));
#22871=CARTESIAN_POINT('Ctrl Pts',(-1.4702867290402E-11,-101.970483118095,
-8.16439679232146));
#22872=CARTESIAN_POINT('Ctrl Pts',(-4.71371668583241,-101.795483118095,
-8.16439679231297));
#22873=CARTESIAN_POINT('Ctrl Pts',(-7.07057502873392,-101.620483118095,
-4.082198396148));
#22874=CARTESIAN_POINT('Ctrl Pts',(-9.42743337163542,-101.445483118095,
1.69768315121407E-11));
#22875=CARTESIAN_POINT('Ctrl Pts',(-7.07057502871922,-101.270483118095,
4.08219839617346));
#22876=CARTESIAN_POINT('Ctrl Pts',(-4.71371668580301,-101.095483118095,
8.16439679232994));
#22877=CARTESIAN_POINT('Ctrl Pts',(1.47018674401621E-11,-100.920483118095,
8.16439679232146));
#22878=CARTESIAN_POINT('Ctrl Pts',(4.71371668583241,-100.745483118095,8.16439679231297));
#22879=CARTESIAN_POINT('Ctrl Pts',(7.07057502873392,-100.570483118095,4.082198396148));
#22880=CARTESIAN_POINT('Ctrl Pts',(9.42743337163542,-100.395483118095,-1.69756769845304E-11));
#22881=CARTESIAN_POINT('Ctrl Pts',(7.07057502871922,-100.220483118095,-4.08219839617346));
#22882=CARTESIAN_POINT('Ctrl Pts',(4.71371668580301,-100.045483118095,-8.16439679232994));
#22883=CARTESIAN_POINT('Ctrl Pts',(-1.4702867290402E-11,-99.8704831180952,
-8.16439679232146));
#22884=CARTESIAN_POINT('Ctrl Pts',(-4.71371668583241,-99.6954831180952,
-8.16439679231297));
#22885=CARTESIAN_POINT('Ctrl Pts',(-7.07057502873392,-99.5204831180952,
-4.082198396148));
#22886=CARTESIAN_POINT('Ctrl Pts',(-9.42743337163542,-99.3454831180952,
1.69768315121407E-11));
#22887=CARTESIAN_POINT('Ctrl Pts',(-7.07057502871922,-99.1704831180952,
4.08219839617346));
#22888=CARTESIAN_POINT('Ctrl Pts',(-4.71371668580301,-98.9954831180952,
8.16439679232994));
#22889=CARTESIAN_POINT('Ctrl Pts',(1.47018674401621E-11,-98.8204831180952,
8.16439679232146));
#22890=CARTESIAN_POINT('Ctrl Pts',(4.71371668583241,-98.6454831180952,8.16439679231297));
#22891=CARTESIAN_POINT('Ctrl Pts',(7.07057502873392,-98.4704831180952,4.082198396148));
#22892=CARTESIAN_POINT('Ctrl Pts',(9.42743337163542,-98.2954831180952,-1.69756769845304E-11));
#22893=CARTESIAN_POINT('Ctrl Pts',(7.07057502871922,-98.1204831180952,-4.08219839617346));
#22894=CARTESIAN_POINT('Ctrl Pts',(4.71371668580301,-97.9454831180952,-8.16439679232994));
#22895=CARTESIAN_POINT('Ctrl Pts',(-1.4702867290402E-11,-97.7704831180952,
-8.16439679232146));
#22896=CARTESIAN_POINT('Ctrl Pts',(-4.71371668583241,-97.5954831180952,
-8.16439679231297));
#22897=CARTESIAN_POINT('Ctrl Pts',(-7.07057502873392,-97.4204831180952,
-4.082198396148));
#22898=CARTESIAN_POINT('Ctrl Pts',(-9.42743337163542,-97.2454831180952,
1.69768315121407E-11));
#22899=CARTESIAN_POINT('Ctrl Pts',(-7.07057502871922,-97.0704831180952,
4.08219839617346));
#22900=CARTESIAN_POINT('Ctrl Pts',(-4.71371668580301,-96.8954831180952,
8.16439679232994));
#22901=CARTESIAN_POINT('Ctrl Pts',(1.47018674401621E-11,-96.7204831180952,
8.16439679232146));
#22902=CARTESIAN_POINT('Ctrl Pts',(4.71371668583241,-96.5454831180952,8.16439679231297));
#22903=CARTESIAN_POINT('Ctrl Pts',(7.07057502873392,-96.3704831180952,4.082198396148));
#22904=CARTESIAN_POINT('Ctrl Pts',(9.42743337163542,-96.1954831180952,-1.69756769845304E-11));
#22905=CARTESIAN_POINT('Ctrl Pts',(7.07057502871922,-96.0204831180952,-4.08219839617346));
#22906=CARTESIAN_POINT('Ctrl Pts',(4.71371668580301,-95.8454831180952,-8.16439679232994));
#22907=CARTESIAN_POINT('Ctrl Pts',(-1.4702867290402E-11,-95.6704831180952,
-8.16439679232146));
#22908=CARTESIAN_POINT('Ctrl Pts',(-4.71371668583241,-95.4954831180952,
-8.16439679231297));
#22909=CARTESIAN_POINT('Ctrl Pts',(-7.07057502873392,-95.3204831180952,
-4.082198396148));
#22910=CARTESIAN_POINT('Ctrl Pts',(-9.42743337163542,-95.1454831180952,
1.69768315121407E-11));
#22911=CARTESIAN_POINT('Ctrl Pts',(-7.07057502871922,-94.9704831180952,
4.08219839617346));
#22912=CARTESIAN_POINT('Ctrl Pts',(-4.71371668580301,-94.7954831180952,
8.16439679232994));
#22913=CARTESIAN_POINT('Ctrl Pts',(1.47018674401621E-11,-94.6204831180952,
8.16439679232146));
#22914=CARTESIAN_POINT('Ctrl Pts',(4.71371668583241,-94.4454831180952,8.16439679231297));
#22915=CARTESIAN_POINT('Ctrl Pts',(7.07057502873392,-94.2704831180952,4.082198396148));
#22916=CARTESIAN_POINT('Ctrl Pts',(9.42743337163542,-94.0954831180952,-1.69756769845304E-11));
#22917=CARTESIAN_POINT('Ctrl Pts',(7.07057502871922,-93.9204831180952,-4.08219839617346));
#22918=CARTESIAN_POINT('Ctrl Pts',(4.71371668580301,-93.7454831180952,-8.16439679232994));
#22919=CARTESIAN_POINT('Ctrl Pts',(-1.4702867290402E-11,-93.5704831180952,
-8.16439679232146));
#22920=CARTESIAN_POINT('Ctrl Pts',(-4.71371668583241,-93.3954831180952,
-8.16439679231297));
#22921=CARTESIAN_POINT('Ctrl Pts',(-7.07057502873392,-93.2204831180952,
-4.082198396148));
#22922=CARTESIAN_POINT('Ctrl Pts',(-9.42743337163542,-93.0454831180952,
1.69768315121407E-11));
#22923=CARTESIAN_POINT('Ctrl Pts',(-7.07057502871922,-92.8704831180952,
4.08219839617346));
#22924=CARTESIAN_POINT('Ctrl Pts',(-4.71371668580301,-92.6954831180952,
8.16439679232994));
#22925=CARTESIAN_POINT('Ctrl Pts',(1.47018674401621E-11,-92.5204831180952,
8.16439679232146));
#22926=CARTESIAN_POINT('Ctrl Pts',(4.71371668583241,-92.3454831180952,8.16439679231297));
#22927=CARTESIAN_POINT('Ctrl Pts',(7.07057502873392,-92.1704831180952,4.082198396148));
#22928=CARTESIAN_POINT('Ctrl Pts',(9.42743337163542,-91.9954831180952,-1.69756769845304E-11));
#22929=CARTESIAN_POINT('Ctrl Pts',(7.07057502871922,-91.8204831180952,-4.08219839617346));
#22930=CARTESIAN_POINT('Ctrl Pts',(4.71371668580301,-91.6454831180952,-8.16439679232994));
#22931=CARTESIAN_POINT('Ctrl Pts',(-1.4702867290402E-11,-91.4704831180952,
-8.16439679232146));
#22932=CARTESIAN_POINT('Ctrl Pts',(-4.71371668583241,-91.2954831180952,
-8.16439679231297));
#22933=CARTESIAN_POINT('Ctrl Pts',(-7.07057502873392,-91.1204831180952,
-4.082198396148));
#22934=CARTESIAN_POINT('Ctrl Pts',(-9.42743337163542,-90.9454831180952,
1.69768315121407E-11));
#22935=CARTESIAN_POINT('Ctrl Pts',(-7.07057502871922,-90.7704831180952,
4.08219839617346));
#22936=CARTESIAN_POINT('Ctrl Pts',(-4.71371668580301,-90.5954831180952,
8.16439679232994));
#22937=CARTESIAN_POINT('Ctrl Pts',(1.47018674401621E-11,-90.4204831180952,
8.16439679232146));
#22938=CARTESIAN_POINT('Ctrl Pts',(4.71371668583241,-90.2454831180952,8.16439679231297));
#22939=CARTESIAN_POINT('Ctrl Pts',(7.07057502873392,-90.0704831180952,4.082198396148));
#22940=CARTESIAN_POINT('Ctrl Pts',(9.42743337163542,-89.8954831180952,-1.69756769845304E-11));
#22941=CARTESIAN_POINT('Ctrl Pts',(7.07057502871922,-89.7204831180952,-4.08219839617346));
#22942=CARTESIAN_POINT('Ctrl Pts',(4.71371668580301,-89.5454831180952,-8.16439679232994));
#22943=CARTESIAN_POINT('Ctrl Pts',(-1.4702867290402E-11,-89.3704831180952,
-8.16439679232146));
#22944=CARTESIAN_POINT('Ctrl Pts',(-4.71371668583241,-89.1954831180952,
-8.16439679231297));
#22945=CARTESIAN_POINT('Ctrl Pts',(-7.07057502873392,-89.0204831180952,
-4.082198396148));
#22946=CARTESIAN_POINT('Ctrl Pts',(-9.42743337163542,-88.8454831180952,
1.69768315121407E-11));
#22947=CARTESIAN_POINT('Ctrl Pts',(-7.07057502871922,-88.6704831180952,
4.08219839617346));
#22948=CARTESIAN_POINT('Ctrl Pts',(-4.71371668580301,-88.4954831180952,
8.16439679232994));
#22949=CARTESIAN_POINT('Ctrl Pts',(1.47018674401621E-11,-88.3204831180952,
8.16439679232146));
#22950=CARTESIAN_POINT('Ctrl Pts',(4.71371668583241,-88.1454831180952,8.16439679231297));
#22951=CARTESIAN_POINT('Ctrl Pts',(7.07057502873392,-87.9704831180952,4.082198396148));
#22952=CARTESIAN_POINT('Ctrl Pts',(9.42743337163542,-87.7954831180952,-1.69756769845304E-11));
#22953=CARTESIAN_POINT('Ctrl Pts',(7.07057502871922,-87.6204831180952,-4.08219839617346));
#22954=CARTESIAN_POINT('Ctrl Pts',(4.71371668580301,-87.4454831180952,-8.16439679232994));
#22955=CARTESIAN_POINT('Ctrl Pts',(-1.4702867290402E-11,-87.2704831180952,
-8.16439679232146));
#22956=CARTESIAN_POINT('Ctrl Pts',(-4.71371668583241,-87.0954831180952,
-8.16439679231297));
#22957=CARTESIAN_POINT('Ctrl Pts',(-7.07057502873392,-86.9204831180952,
-4.082198396148));
#22958=CARTESIAN_POINT('Ctrl Pts',(-9.42743337163542,-86.7454831180952,
1.69768315121407E-11));
#22959=CARTESIAN_POINT('Ctrl Pts',(-7.07057502871922,-86.5704831180952,
4.08219839617346));
#22960=CARTESIAN_POINT('Ctrl Pts',(-4.71371668580301,-86.3954831180952,
8.16439679232994));
#22961=CARTESIAN_POINT('Ctrl Pts',(1.47018674401621E-11,-86.2204831180952,
8.16439679232146));
#22962=CARTESIAN_POINT('Ctrl Pts',(4.71371668583241,-86.0454831180952,8.16439679231297));
#22963=CARTESIAN_POINT('Ctrl Pts',(7.07057502873392,-85.8704831180952,4.082198396148));
#22964=CARTESIAN_POINT('Ctrl Pts',(9.42743337163542,-85.6954831180952,-1.69756769845304E-11));
#22965=CARTESIAN_POINT('Ctrl Pts',(7.07057502871922,-85.5204831180952,-4.08219839617346));
#22966=CARTESIAN_POINT('Ctrl Pts',(4.71371668580301,-85.3454831180952,-8.16439679232994));
#22967=CARTESIAN_POINT('Ctrl Pts',(-1.4702867290402E-11,-85.1704831180952,
-8.16439679232146));
#22968=CARTESIAN_POINT('Ctrl Pts',(-4.71371668583241,-84.9954831180952,
-8.16439679231297));
#22969=CARTESIAN_POINT('Ctrl Pts',(-7.07057502873392,-84.8204831180952,
-4.082198396148));
#22970=CARTESIAN_POINT('Ctrl Pts',(-9.42743337163542,-84.6454831180952,
1.69768315121407E-11));
#22971=CARTESIAN_POINT('Ctrl Pts',(-7.07057502871922,-84.4704831180952,
4.08219839617346));
#22972=CARTESIAN_POINT('Ctrl Pts',(-4.71371668580301,-84.2954831180952,
8.16439679232994));
#22973=CARTESIAN_POINT('Ctrl Pts',(1.47018674401621E-11,-84.1204831180952,
8.16439679232146));
#22974=CARTESIAN_POINT('Ctrl Pts',(4.71371668583241,-83.9454831180952,8.16439679231297));
#22975=CARTESIAN_POINT('Ctrl Pts',(7.07057502873392,-83.7704831180952,4.082198396148));
#22976=CARTESIAN_POINT('Ctrl Pts',(9.42743337163542,-83.5954831180952,-1.69756769845304E-11));
#22977=CARTESIAN_POINT('Ctrl Pts',(7.07057502871922,-83.4204831180952,-4.08219839617346));
#22978=CARTESIAN_POINT('Ctrl Pts',(4.71371668580301,-83.2454831180952,-8.16439679232994));
#22979=CARTESIAN_POINT('Ctrl Pts',(-1.4702867290402E-11,-83.0704831180952,
-8.16439679232146));
#22980=CARTESIAN_POINT('Ctrl Pts',(-4.71371668583241,-82.8954831180952,
-8.16439679231297));
#22981=CARTESIAN_POINT('Ctrl Pts',(-7.07057502873392,-82.7204831180952,
-4.082198396148));
#22982=CARTESIAN_POINT('Ctrl Pts',(-9.42743337163542,-82.5454831180952,
1.69768315121407E-11));
#22983=CARTESIAN_POINT('Ctrl Pts',(-7.07057502871922,-82.3704831180952,
4.08219839617346));
#22984=CARTESIAN_POINT('Ctrl Pts',(-4.71371668580301,-82.1954831180952,
8.16439679232994));
#22985=CARTESIAN_POINT('Ctrl Pts',(1.47018674401621E-11,-82.0204831180952,
8.16439679232146));
#22986=CARTESIAN_POINT('Ctrl Pts',(4.71371668583241,-81.8454831180952,8.16439679231297));
#22987=CARTESIAN_POINT('Ctrl Pts',(7.07057502873392,-81.6704831180952,4.082198396148));
#22988=CARTESIAN_POINT('Ctrl Pts',(9.42743337163542,-81.4954831180952,-1.69756769845304E-11));
#22989=CARTESIAN_POINT('Ctrl Pts',(7.07057502871922,-81.3204831180952,-4.08219839617346));
#22990=CARTESIAN_POINT('Ctrl Pts',(4.71371668580301,-81.1454831180953,-8.16439679232994));
#22991=CARTESIAN_POINT('Ctrl Pts',(-1.4702867290402E-11,-80.9704831180952,
-8.16439679232146));
#22992=CARTESIAN_POINT('Ctrl Pts',(-4.71371668583241,-80.7954831180952,
-8.16439679231297));
#22993=CARTESIAN_POINT('Ctrl Pts',(-7.07057502873392,-80.6204831180952,
-4.082198396148));
#22994=CARTESIAN_POINT('Ctrl Pts',(-9.42743337163542,-80.4454831180952,
1.69768315121407E-11));
#22995=CARTESIAN_POINT('Ctrl Pts',(-7.07057502871922,-80.2704831180952,
4.08219839617346));
#22996=CARTESIAN_POINT('Ctrl Pts',(-4.71371668580301,-80.0954831180952,
8.16439679232994));
#22997=CARTESIAN_POINT('Ctrl Pts',(1.47018674401621E-11,-79.9204831180952,
8.16439679232146));
#22998=CARTESIAN_POINT('Ctrl Pts',(4.71371668583241,-79.7454831180953,8.16439679231297));
#22999=CARTESIAN_POINT('Ctrl Pts',(7.07057502873392,-79.5704831180952,4.082198396148));
#23000=CARTESIAN_POINT('Ctrl Pts',(9.42743337163542,-79.3954831180952,-1.69756769845304E-11));
#23001=CARTESIAN_POINT('Ctrl Pts',(7.07057502871922,-79.2204831180952,-4.08219839617346));
#23002=CARTESIAN_POINT('Ctrl Pts',(4.71371668580301,-79.0454831180952,-8.16439679232994));
#23003=CARTESIAN_POINT('Ctrl Pts',(-1.4702867290402E-11,-78.8704831180952,
-8.16439679232146));
#23004=CARTESIAN_POINT('Ctrl Pts',(-4.71371668583241,-78.6954831180953,
-8.16439679231297));
#23005=CARTESIAN_POINT('Ctrl Pts',(-7.07057502873392,-78.5204831180952,
-4.082198396148));
#23006=CARTESIAN_POINT('Ctrl Pts',(-9.42743337163542,-78.3454831180952,
1.69768315121407E-11));
#23007=CARTESIAN_POINT('Ctrl Pts',(-7.07057502871922,-78.1704831180953,
4.08219839617346));
#23008=CARTESIAN_POINT('Ctrl Pts',(-4.71371668580301,-77.9954831180953,
8.16439679232994));
#23009=CARTESIAN_POINT('Ctrl Pts',(1.47018674401621E-11,-77.8204831180952,
8.16439679232146));
#23010=CARTESIAN_POINT('Ctrl Pts',(4.71371668583241,-77.6454831180953,8.16439679231297));
#23011=CARTESIAN_POINT('Ctrl Pts',(7.07057502873392,-77.4704831180952,4.082198396148));
#23012=CARTESIAN_POINT('Ctrl Pts',(9.42743337163542,-77.2954831180952,-1.69756769845304E-11));
#23013=CARTESIAN_POINT('Ctrl Pts',(7.07057502871922,-77.1204831180952,-4.08219839617346));
#23014=CARTESIAN_POINT('Ctrl Pts',(4.71371668580301,-76.9454831180952,-8.16439679232994));
#23015=CARTESIAN_POINT('Ctrl Pts',(-1.4702867290402E-11,-76.7704831180952,
-8.16439679232146));
#23016=CARTESIAN_POINT('Ctrl Pts',(-4.71371668583241,-76.5954831180953,
-8.16439679231297));
#23017=CARTESIAN_POINT('Ctrl Pts',(-7.07057502873392,-76.4204831180952,
-4.082198396148));
#23018=CARTESIAN_POINT('Ctrl Pts',(-9.42743337163542,-76.2454831180952,
1.69768315121407E-11));
#23019=CARTESIAN_POINT('Ctrl Pts',(-7.07057502871922,-76.0704831180952,
4.08219839617346));
#23020=CARTESIAN_POINT('Ctrl Pts',(-4.71371668580301,-75.8954831180952,
8.16439679232994));
#23021=CARTESIAN_POINT('Ctrl Pts',(1.47018674401621E-11,-75.7204831180952,
8.16439679232146));
#23022=CARTESIAN_POINT('Ctrl Pts',(4.71371668583241,-75.5454831180952,8.16439679231297));
#23023=CARTESIAN_POINT('Ctrl Pts',(7.07057502873392,-75.3704831180952,4.082198396148));
#23024=CARTESIAN_POINT('Ctrl Pts',(9.42743337163542,-75.1954831180952,-1.69756769845304E-11));
#23025=CARTESIAN_POINT('Ctrl Pts',(7.07057502871922,-75.0204831180952,-4.08219839617346));
#23026=CARTESIAN_POINT('Ctrl Pts',(4.71371668580301,-74.8454831180952,-8.16439679232994));
#23027=CARTESIAN_POINT('Ctrl Pts',(-1.4702867290402E-11,-74.6704831180952,
-8.16439679232146));
#23028=CARTESIAN_POINT('Ctrl Pts',(-4.71371668583241,-74.4954831180953,
-8.16439679231297));
#23029=CARTESIAN_POINT('Ctrl Pts',(-7.07057502873392,-74.3204831180952,
-4.082198396148));
#23030=CARTESIAN_POINT('Ctrl Pts',(-9.42743337163542,-74.1454831180952,
1.69768315121407E-11));
#23031=CARTESIAN_POINT('Ctrl Pts',(-7.07057502871922,-73.9704831180952,
4.08219839617346));
#23032=CARTESIAN_POINT('Ctrl Pts',(-4.71371668580301,-73.7954831180952,
8.16439679232994));
#23033=CARTESIAN_POINT('Ctrl Pts',(1.47018674401621E-11,-73.6204831180952,
8.16439679232146));
#23034=CARTESIAN_POINT('Ctrl Pts',(4.71371668583241,-73.4454831180953,8.16439679231297));
#23035=CARTESIAN_POINT('Ctrl Pts',(7.07057502873392,-73.2704831180952,4.082198396148));
#23036=CARTESIAN_POINT('Ctrl Pts',(9.42743337163542,-73.0954831180953,-1.69756769845304E-11));
#23037=CARTESIAN_POINT('Ctrl Pts',(7.07057502871922,-72.9204831180952,-4.08219839617346));
#23038=CARTESIAN_POINT('Ctrl Pts',(4.71371668580301,-72.7454831180952,-8.16439679232994));
#23039=CARTESIAN_POINT('Ctrl Pts',(-1.4702867290402E-11,-72.5704831180953,
-8.16439679232146));
#23040=CARTESIAN_POINT('Ctrl Pts',(-4.71371668583241,-72.3954831180953,
-8.16439679231297));
#23041=CARTESIAN_POINT('Ctrl Pts',(-7.07057502873392,-72.2204831180952,
-4.082198396148));
#23042=CARTESIAN_POINT('Ctrl Pts',(-9.42743337163542,-72.0454831180953,
1.69768315121407E-11));
#23043=CARTESIAN_POINT('Ctrl Pts',(-7.07057502871922,-71.8704831180952,
4.08219839617346));
#23044=CARTESIAN_POINT('Ctrl Pts',(-4.71371668580301,-71.6954831180952,
8.16439679232994));
#23045=CARTESIAN_POINT('Ctrl Pts',(1.47018674401621E-11,-71.5204831180953,
8.16439679232146));
#23046=CARTESIAN_POINT('Ctrl Pts',(4.71371668583241,-71.3454831180952,8.16439679231297));
#23047=CARTESIAN_POINT('Ctrl Pts',(7.07057502873392,-71.1704831180952,4.082198396148));
#23048=CARTESIAN_POINT('Ctrl Pts',(9.42743337163542,-70.9954831180953,-1.69756769845304E-11));
#23049=CARTESIAN_POINT('Ctrl Pts',(7.07057502871922,-70.8204831180952,-4.08219839617346));
#23050=CARTESIAN_POINT('Ctrl Pts',(4.71371668580301,-70.6454831180952,-8.16439679232994));
#23051=CARTESIAN_POINT('Ctrl Pts',(-1.4702867290402E-11,-70.4704831180953,
-8.16439679232146));
#23052=CARTESIAN_POINT('Ctrl Pts',(-4.71371668583241,-70.2954831180952,
-8.16439679231297));
#23053=CARTESIAN_POINT('Ctrl Pts',(-7.07057502873392,-70.1204831180952,
-4.082198396148));
#23054=CARTESIAN_POINT('Ctrl Pts',(-9.42743337163542,-69.9454831180953,
1.69768315121407E-11));
#23055=CARTESIAN_POINT('Ctrl Pts',(-7.07057502871922,-69.7704831180953,
4.08219839617346));
#23056=CARTESIAN_POINT('Ctrl Pts',(-4.71371668580301,-69.5954831180952,
8.16439679232994));
#23057=CARTESIAN_POINT('Ctrl Pts',(1.47018674401621E-11,-69.4204831180953,
8.16439679232146));
#23058=CARTESIAN_POINT('Ctrl Pts',(4.71371668583241,-69.2454831180953,8.16439679231297));
#23059=CARTESIAN_POINT('Ctrl Pts',(7.07057502873392,-69.0704831180953,4.082198396148));
#23060=CARTESIAN_POINT('Ctrl Pts',(9.42743337163542,-68.8954831180953,-1.69756769845304E-11));
#23061=CARTESIAN_POINT('Ctrl Pts',(7.07057502871922,-68.7204831180952,-4.08219839617346));
#23062=CARTESIAN_POINT('Ctrl Pts',(4.71371668580301,-68.5454831180952,-8.16439679232994));
#23063=CARTESIAN_POINT('Ctrl Pts',(-1.4702867290402E-11,-68.3704831180953,
-8.16439679232146));
#23064=CARTESIAN_POINT('Ctrl Pts',(-4.71371668583241,-68.1954831180952,
-8.16439679231297));
#23065=CARTESIAN_POINT('Ctrl Pts',(-7.07057502873392,-68.0204831180953,
-4.082198396148));
#23066=CARTESIAN_POINT('Ctrl Pts',(-9.42743337163542,-67.8454831180953,
1.69768315121407E-11));
#23067=CARTESIAN_POINT('Ctrl Pts',(-7.07057502871922,-67.6704831180952,
4.08219839617346));
#23068=CARTESIAN_POINT('Ctrl Pts',(-4.71371668580301,-67.4954831180953,
8.16439679232994));
#23069=CARTESIAN_POINT('Ctrl Pts',(1.47018674401621E-11,-67.3204831180953,
8.16439679232146));
#23070=CARTESIAN_POINT('Ctrl Pts',(4.71371668583241,-67.1454831180952,8.16439679231297));
#23071=CARTESIAN_POINT('Ctrl Pts',(7.07057502873392,-66.9704831180952,4.082198396148));
#23072=CARTESIAN_POINT('Ctrl Pts',(9.42743337163542,-66.7954831180953,-1.69756769845304E-11));
#23073=CARTESIAN_POINT('Ctrl Pts',(7.07057502871922,-66.6204831180952,-4.08219839617346));
#23074=CARTESIAN_POINT('Ctrl Pts',(4.71371668580301,-66.4454831180952,-8.16439679232994));
#23075=CARTESIAN_POINT('Ctrl Pts',(-1.4702867290402E-11,-66.2704831180953,
-8.16439679232146));
#23076=CARTESIAN_POINT('Ctrl Pts',(-4.71371668583241,-66.0954831180952,
-8.16439679231297));
#23077=CARTESIAN_POINT('Ctrl Pts',(-7.07057502873392,-65.9204831180952,
-4.082198396148));
#23078=CARTESIAN_POINT('Ctrl Pts',(-9.42743337163542,-65.7454831180953,
1.69768315121407E-11));
#23079=CARTESIAN_POINT('Ctrl Pts',(-7.07057502871922,-65.5704831180953,
4.08219839617346));
#23080=CARTESIAN_POINT('Ctrl Pts',(-4.71371668580301,-65.3954831180953,
8.16439679232994));
#23081=CARTESIAN_POINT('Ctrl Pts',(1.47018674401621E-11,-65.2204831180952,
8.16439679232146));
#23082=CARTESIAN_POINT('Ctrl Pts',(4.71371668583241,-65.0454831180952,8.16439679231297));
#23083=CARTESIAN_POINT('Ctrl Pts',(7.07057502873392,-64.8704831180953,4.082198396148));
#23084=CARTESIAN_POINT('Ctrl Pts',(9.42743337163542,-64.6954831180953,-1.69756769845304E-11));
#23085=CARTESIAN_POINT('Ctrl Pts',(7.07057502871922,-64.5204831180953,-4.08219839617346));
#23086=CARTESIAN_POINT('Ctrl Pts',(4.71371668580301,-64.3454831180953,-8.16439679232994));
#23087=CARTESIAN_POINT('Ctrl Pts',(-1.4702867290402E-11,-64.1704831180952,
-8.16439679232146));
#23088=CARTESIAN_POINT('Ctrl Pts',(-4.71371668583241,-63.9954831180953,
-8.16439679231297));
#23089=CARTESIAN_POINT('Ctrl Pts',(-7.07057502873392,-63.8204831180953,
-4.082198396148));
#23090=CARTESIAN_POINT('Ctrl Pts',(-9.42743337163542,-63.6454831180953,
1.69768315121407E-11));
#23091=CARTESIAN_POINT('Ctrl Pts',(-7.07057502871922,-63.4704831180953,
4.08219839617346));
#23092=CARTESIAN_POINT('Ctrl Pts',(-4.71371668580301,-63.2954831180953,
8.16439679232994));
#23093=CARTESIAN_POINT('Ctrl Pts',(1.47018674401621E-11,-63.1204831180953,
8.16439679232146));
#23094=CARTESIAN_POINT('Ctrl Pts',(4.71371668583241,-62.9454831180952,8.16439679231297));
#23095=CARTESIAN_POINT('Ctrl Pts',(7.07057502873392,-62.7704831180953,4.082198396148));
#23096=CARTESIAN_POINT('Ctrl Pts',(9.42743337163542,-62.5954831180953,-1.69756769845304E-11));
#23097=CARTESIAN_POINT('Ctrl Pts',(7.07057502871922,-62.4204831180953,-4.08219839617346));
#23098=CARTESIAN_POINT('Ctrl Pts',(4.71371668580301,-62.2454831180953,-8.16439679232994));
#23099=CARTESIAN_POINT('Ctrl Pts',(-1.4702867290402E-11,-62.0704831180953,
-8.16439679232146));
#23100=CARTESIAN_POINT('Ctrl Pts',(-4.71371668583241,-61.8954831180952,
-8.16439679231297));
#23101=CARTESIAN_POINT('Ctrl Pts',(-7.07057502873392,-61.7204831180953,
-4.082198396148));
#23102=CARTESIAN_POINT('Ctrl Pts',(-9.42743337163542,-61.5454831180953,
1.69768315121407E-11));
#23103=CARTESIAN_POINT('Ctrl Pts',(-7.07057502871922,-61.3704831180953,
4.08219839617346));
#23104=CARTESIAN_POINT('Ctrl Pts',(-4.71371668580301,-61.1954831180953,
8.16439679232994));
#23105=CARTESIAN_POINT('Ctrl Pts',(1.47018674401621E-11,-61.0204831180953,
8.16439679232146));
#23106=CARTESIAN_POINT('Ctrl Pts',(4.71371668583241,-60.8454831180953,8.16439679231297));
#23107=CARTESIAN_POINT('Ctrl Pts',(7.07057502873392,-60.6704831180953,4.082198396148));
#23108=CARTESIAN_POINT('Ctrl Pts',(9.42743337163542,-60.4954831180953,-1.69756769845304E-11));
#23109=CARTESIAN_POINT('Ctrl Pts',(7.07057502871922,-60.3204831180953,-4.08219839617346));
#23110=CARTESIAN_POINT('Ctrl Pts',(4.71371668580301,-60.1454831180953,-8.16439679232994));
#23111=CARTESIAN_POINT('Ctrl Pts',(-1.4702867290402E-11,-59.9704831180953,
-8.16439679232146));
#23112=CARTESIAN_POINT('Ctrl Pts',(-4.71371668583241,-59.7954831180953,
-8.16439679231297));
#23113=CARTESIAN_POINT('Ctrl Pts',(-7.07057502873392,-59.6204831180953,
-4.082198396148));
#23114=CARTESIAN_POINT('Ctrl Pts',(-9.42743337163542,-59.4454831180953,
1.69768315121407E-11));
#23115=CARTESIAN_POINT('Ctrl Pts',(-7.07057502871922,-59.2704831180953,
4.08219839617346));
#23116=CARTESIAN_POINT('Ctrl Pts',(-4.71371668580301,-59.0954831180953,
8.16439679232994));
#23117=CARTESIAN_POINT('Ctrl Pts',(1.47018674401621E-11,-58.9204831180953,
8.16439679232146));
#23118=CARTESIAN_POINT('Ctrl Pts',(4.71371668583241,-58.7454831180953,8.16439679231297));
#23119=CARTESIAN_POINT('Ctrl Pts',(7.07057502873392,-58.5704831180953,4.082198396148));
#23120=CARTESIAN_POINT('Ctrl Pts',(9.42743337163542,-58.3954831180953,-1.69756769845304E-11));
#23121=CARTESIAN_POINT('Ctrl Pts',(7.07057502871922,-58.2204831180953,-4.08219839617346));
#23122=CARTESIAN_POINT('Ctrl Pts',(4.71371668580301,-58.0454831180953,-8.16439679232994));
#23123=CARTESIAN_POINT('Ctrl Pts',(-1.4702867290402E-11,-57.8704831180952,
-8.16439679232146));
#23124=CARTESIAN_POINT('Ctrl Pts',(-4.71371668583241,-57.6954831180953,
-8.16439679231297));
#23125=CARTESIAN_POINT('Ctrl Pts',(-7.07057502873392,-57.5204831180953,
-4.082198396148));
#23126=CARTESIAN_POINT('Ctrl Pts',(-9.42743337163542,-57.3454831180953,
1.69768315121407E-11));
#23127=CARTESIAN_POINT('Ctrl Pts',(-7.07057502871922,-57.1704831180953,
4.08219839617346));
#23128=CARTESIAN_POINT('Ctrl Pts',(-4.71371668580301,-56.9954831180953,
8.16439679232994));
#23129=CARTESIAN_POINT('Ctrl Pts',(1.47018674401621E-11,-56.8204831180953,
8.16439679232146));
#23130=CARTESIAN_POINT('Ctrl Pts',(4.71371668583241,-56.6454831180953,8.16439679231297));
#23131=CARTESIAN_POINT('Ctrl Pts',(7.07057502873392,-56.4704831180953,4.082198396148));
#23132=CARTESIAN_POINT('Ctrl Pts',(9.42743337163542,-56.2954831180953,-1.69756769845304E-11));
#23133=CARTESIAN_POINT('Ctrl Pts',(7.07057502871922,-56.1204831180953,-4.08219839617346));
#23134=CARTESIAN_POINT('Ctrl Pts',(4.71371668580301,-55.9454831180953,-8.16439679232994));
#23135=CARTESIAN_POINT('Ctrl Pts',(-1.4702867290402E-11,-55.7704831180953,
-8.16439679232146));
#23136=CARTESIAN_POINT('Ctrl Pts',(-4.71371668583241,-55.5954831180953,
-8.16439679231297));
#23137=CARTESIAN_POINT('Ctrl Pts',(-7.07057502873392,-55.4204831180953,
-4.082198396148));
#23138=CARTESIAN_POINT('Ctrl Pts',(-9.42743337163542,-55.2454831180953,
1.69768315121407E-11));
#23139=CARTESIAN_POINT('Ctrl Pts',(-7.07057502871922,-55.0704831180953,
4.08219839617346));
#23140=CARTESIAN_POINT('Ctrl Pts',(-4.71371668580301,-54.8954831180953,
8.16439679232994));
#23141=CARTESIAN_POINT('Ctrl Pts',(1.47018674401621E-11,-54.7204831180953,
8.16439679232146));
#23142=CARTESIAN_POINT('Ctrl Pts',(4.71371668583241,-54.5454831180953,8.16439679231297));
#23143=CARTESIAN_POINT('Ctrl Pts',(7.07057502873392,-54.3704831180953,4.082198396148));
#23144=CARTESIAN_POINT('Ctrl Pts',(9.42743337163542,-54.1954831180953,-1.69756769845304E-11));
#23145=CARTESIAN_POINT('Ctrl Pts',(7.07057502871922,-54.0204831180953,-4.08219839617346));
#23146=CARTESIAN_POINT('Ctrl Pts',(4.71371668580301,-53.8454831180953,-8.16439679232994));
#23147=CARTESIAN_POINT('Ctrl Pts',(-1.4702867290402E-11,-53.6704831180953,
-8.16439679232146));
#23148=CARTESIAN_POINT('Ctrl Pts',(-4.71371668583241,-53.4954831180953,
-8.16439679231297));
#23149=CARTESIAN_POINT('Ctrl Pts',(-7.07057502873392,-53.3204831180953,
-4.082198396148));
#23150=CARTESIAN_POINT('Ctrl Pts',(-9.42743337163542,-53.1454831180953,
1.69768315121407E-11));
#23151=CARTESIAN_POINT('Ctrl Pts',(-7.07057502871922,-52.9704831180953,
4.08219839617346));
#23152=CARTESIAN_POINT('Ctrl Pts',(-4.71371668580301,-52.7954831180953,
8.16439679232994));
#23153=CARTESIAN_POINT('Ctrl Pts',(1.47018674401621E-11,-52.6204831180953,
8.16439679232146));
#23154=CARTESIAN_POINT('Ctrl Pts',(4.71371668583241,-52.4454831180953,8.16439679231297));
#23155=CARTESIAN_POINT('Ctrl Pts',(7.07057502873392,-52.2704831180953,4.082198396148));
#23156=CARTESIAN_POINT('Ctrl Pts',(9.42743337163542,-52.0954831180953,-1.69756769845304E-11));
#23157=CARTESIAN_POINT('Ctrl Pts',(7.07057502871922,-51.9204831180953,-4.08219839617346));
#23158=CARTESIAN_POINT('Ctrl Pts',(4.71371668580301,-51.7454831180953,-8.16439679232994));
#23159=CARTESIAN_POINT('Ctrl Pts',(-1.4702867290402E-11,-51.5704831180953,
-8.16439679232146));
#23160=CARTESIAN_POINT('Ctrl Pts',(-4.71371668583241,-51.3954831180953,
-8.16439679231297));
#23161=CARTESIAN_POINT('Ctrl Pts',(-7.07057502873392,-51.2204831180953,
-4.082198396148));
#23162=CARTESIAN_POINT('Ctrl Pts',(-9.42743337163542,-51.0454831180953,
1.69768315121407E-11));
#23163=CARTESIAN_POINT('Ctrl Pts',(-7.07057502871922,-50.8704831180953,
4.08219839617346));
#23164=CARTESIAN_POINT('Ctrl Pts',(-4.71371668580301,-50.6954831180953,
8.16439679232994));
#23165=CARTESIAN_POINT('Ctrl Pts',(1.47018674401621E-11,-50.5204831180953,
8.16439679232146));
#23166=CARTESIAN_POINT('Ctrl Pts',(4.71371668583241,-50.3454831180953,8.16439679231297));
#23167=CARTESIAN_POINT('Ctrl Pts',(7.07057502873392,-50.1704831180953,4.082198396148));
#23168=CARTESIAN_POINT('Ctrl Pts',(9.42743337163542,-49.9954831180953,-1.69756769845304E-11));
#23169=CARTESIAN_POINT('Ctrl Pts',(7.07057502871922,-49.8204831180953,-4.08219839617346));
#23170=CARTESIAN_POINT('Ctrl Pts',(4.71371668580301,-49.6454831180953,-8.16439679232994));
#23171=CARTESIAN_POINT('Ctrl Pts',(-1.4702867290402E-11,-49.4704831180953,
-8.16439679232146));
#23172=CARTESIAN_POINT('Ctrl Pts',(-4.71371668583241,-49.2954831180953,
-8.16439679231297));
#23173=CARTESIAN_POINT('Ctrl Pts',(-7.07057502873392,-49.1204831180953,
-4.082198396148));
#23174=CARTESIAN_POINT('Ctrl Pts',(-9.42743337163542,-48.9454831180953,
1.69768315121407E-11));
#23175=CARTESIAN_POINT('Ctrl Pts',(-7.07057502871922,-48.7704831180953,
4.08219839617346));
#23176=CARTESIAN_POINT('Ctrl Pts',(-4.71371668580301,-48.5954831180953,
8.16439679232994));
#23177=CARTESIAN_POINT('Ctrl Pts',(1.47018674401621E-11,-48.4204831180953,
8.16439679232146));
#23178=CARTESIAN_POINT('Ctrl Pts',(4.71371668583241,-48.2454831180953,8.16439679231297));
#23179=CARTESIAN_POINT('Ctrl Pts',(7.07057502873392,-48.0704831180953,4.082198396148));
#23180=CARTESIAN_POINT('Ctrl Pts',(9.42743337163542,-47.8954831180953,-1.69756769845304E-11));
#23181=CARTESIAN_POINT('Ctrl Pts',(7.07057502871922,-47.7204831180953,-4.08219839617346));
#23182=CARTESIAN_POINT('Ctrl Pts',(4.71371668580301,-47.5454831180953,-8.16439679232994));
#23183=CARTESIAN_POINT('Ctrl Pts',(-1.4702867290402E-11,-47.3704831180953,
-8.16439679232146));
#23184=CARTESIAN_POINT('Ctrl Pts',(-4.71371668583241,-47.1954831180953,
-8.16439679231297));
#23185=CARTESIAN_POINT('Ctrl Pts',(-7.07057502873392,-47.0204831180953,
-4.082198396148));
#23186=CARTESIAN_POINT('Ctrl Pts',(-9.42743337163542,-46.8454831180953,
1.69768315121407E-11));
#23187=CARTESIAN_POINT('Ctrl Pts',(-7.07057502871922,-46.6704831180953,
4.08219839617346));
#23188=CARTESIAN_POINT('Ctrl Pts',(-4.71371668580301,-46.4954831180953,
8.16439679232994));
#23189=CARTESIAN_POINT('Ctrl Pts',(1.47018674401621E-11,-46.3204831180953,
8.16439679232146));
#23190=CARTESIAN_POINT('Ctrl Pts',(4.71371668583241,-46.1454831180953,8.16439679231297));
#23191=CARTESIAN_POINT('Ctrl Pts',(7.07057502873392,-45.9704831180953,4.082198396148));
#23192=CARTESIAN_POINT('Ctrl Pts',(9.42743337163542,-45.7954831180953,-1.69756769845304E-11));
#23193=CARTESIAN_POINT('Ctrl Pts',(7.07057502871922,-45.6204831180953,-4.08219839617346));
#23194=CARTESIAN_POINT('Ctrl Pts',(4.71371668580301,-45.4454831180953,-8.16439679232994));
#23195=CARTESIAN_POINT('Ctrl Pts',(-1.4702867290402E-11,-45.2704831180953,
-8.16439679232146));
#23196=CARTESIAN_POINT('Ctrl Pts',(-4.71371668583241,-45.0954831180953,
-8.16439679231297));
#23197=CARTESIAN_POINT('Ctrl Pts',(-7.07057502873392,-44.9204831180953,
-4.082198396148));
#23198=CARTESIAN_POINT('Ctrl Pts',(-9.42743337163542,-44.7454831180953,
1.69768315121407E-11));
#23199=CARTESIAN_POINT('Ctrl Pts',(-7.07057502871922,-44.5704831180953,
4.08219839617346));
#23200=CARTESIAN_POINT('Ctrl Pts',(-4.71371668580301,-44.3954831180953,
8.16439679232994));
#23201=CARTESIAN_POINT('Ctrl Pts',(1.47018674401621E-11,-44.2204831180953,
8.16439679232146));
#23202=CARTESIAN_POINT('Ctrl Pts',(4.71371668583241,-44.0454831180953,8.16439679231297));
#23203=CARTESIAN_POINT('Ctrl Pts',(7.07057502873392,-43.8704831180953,4.082198396148));
#23204=CARTESIAN_POINT('Ctrl Pts',(9.42743337163542,-43.6954831180953,-1.69756769845304E-11));
#23205=CARTESIAN_POINT('Ctrl Pts',(7.07057502871922,-43.5204831180953,-4.08219839617346));
#23206=CARTESIAN_POINT('Ctrl Pts',(4.71371668580301,-43.3454831180953,-8.16439679232994));
#23207=CARTESIAN_POINT('Ctrl Pts',(-1.4702867290402E-11,-43.1704831180953,
-8.16439679232146));
#23208=CARTESIAN_POINT('Ctrl Pts',(-4.71371668583241,-42.9954831180953,
-8.16439679231297));
#23209=CARTESIAN_POINT('Ctrl Pts',(-7.07057502873392,-42.8204831180953,
-4.082198396148));
#23210=CARTESIAN_POINT('Ctrl Pts',(-9.42743337163542,-42.6454831180953,
1.69768315121407E-11));
#23211=CARTESIAN_POINT('Ctrl Pts',(-7.07057502871922,-42.4704831180953,
4.08219839617346));
#23212=CARTESIAN_POINT('Ctrl Pts',(-4.71371668580301,-42.2954831180953,
8.16439679232994));
#23213=CARTESIAN_POINT('Ctrl Pts',(1.47018674401621E-11,-42.1204831180953,
8.16439679232146));
#23214=CARTESIAN_POINT('Ctrl Pts',(4.71371668583241,-41.9454831180953,8.16439679231297));
#23215=CARTESIAN_POINT('Ctrl Pts',(7.07057502873392,-41.7704831180953,4.082198396148));
#23216=CARTESIAN_POINT('Ctrl Pts',(9.42743337163542,-41.5954831180953,-1.69756769845304E-11));
#23217=CARTESIAN_POINT('Ctrl Pts',(7.07057502871922,-41.4204831180953,-4.08219839617346));
#23218=CARTESIAN_POINT('Ctrl Pts',(4.71371668580301,-41.2454831180953,-8.16439679232994));
#23219=CARTESIAN_POINT('Ctrl Pts',(-1.4702867290402E-11,-41.0704831180953,
-8.16439679232146));
#23220=CARTESIAN_POINT('Ctrl Pts',(-4.71371668583241,-40.8954831180953,
-8.16439679231297));
#23221=CARTESIAN_POINT('Ctrl Pts',(-7.07057502873392,-40.7204831180953,
-4.082198396148));
#23222=CARTESIAN_POINT('Ctrl Pts',(-9.42743337163542,-40.5454831180953,
1.69768315121407E-11));
#23223=CARTESIAN_POINT('Ctrl Pts',(-7.07057502871922,-40.3704831180953,
4.08219839617346));
#23224=CARTESIAN_POINT('Ctrl Pts',(-4.71371668580301,-40.1954831180953,
8.16439679232994));
#23225=CARTESIAN_POINT('Ctrl Pts',(1.47018674401621E-11,-40.0204831180953,
8.16439679232146));
#23226=CARTESIAN_POINT('Ctrl Pts',(4.71371668583241,-39.8454831180953,8.16439679231297));
#23227=CARTESIAN_POINT('Ctrl Pts',(7.07057502873392,-39.6704831180953,4.082198396148));
#23228=CARTESIAN_POINT('Ctrl Pts',(9.42743337163542,-39.4954831180953,-1.69756769845304E-11));
#23229=CARTESIAN_POINT('Ctrl Pts',(7.07057502871922,-39.3204831180953,-4.08219839617346));
#23230=CARTESIAN_POINT('Ctrl Pts',(4.71371668580301,-39.1454831180953,-8.16439679232994));
#23231=CARTESIAN_POINT('Ctrl Pts',(-1.4702867290402E-11,-38.9704831180953,
-8.16439679232146));
#23232=CARTESIAN_POINT('Ctrl Pts',(-4.71371668583241,-38.7954831180953,
-8.16439679231297));
#23233=CARTESIAN_POINT('Ctrl Pts',(-7.07057502873392,-38.6204831180953,
-4.082198396148));
#23234=CARTESIAN_POINT('Ctrl Pts',(-9.42743337163542,-38.4454831180953,
1.69768315121407E-11));
#23235=CARTESIAN_POINT('Ctrl Pts',(-7.07057502871922,-38.2704831180953,
4.08219839617346));
#23236=CARTESIAN_POINT('Ctrl Pts',(-4.71371668580301,-38.0954831180953,
8.16439679232994));
#23237=CARTESIAN_POINT('Ctrl Pts',(1.47018674401621E-11,-37.9204831180953,
8.16439679232146));
#23238=CARTESIAN_POINT('Ctrl Pts',(4.71371668583241,-37.7454831180953,8.16439679231297));
#23239=CARTESIAN_POINT('Ctrl Pts',(7.07057502873392,-37.5704831180953,4.082198396148));
#23240=CARTESIAN_POINT('Ctrl Pts',(9.42743337163542,-37.3954831180953,-1.69756769845304E-11));
#23241=CARTESIAN_POINT('Ctrl Pts',(7.07057502871922,-37.2204831180953,-4.08219839617346));
#23242=CARTESIAN_POINT('Ctrl Pts',(4.71371668580301,-37.0454831180953,-8.16439679232994));
#23243=CARTESIAN_POINT('Ctrl Pts',(-1.4702867290402E-11,-36.8704831180953,
-8.16439679232146));
#23244=CARTESIAN_POINT('Ctrl Pts',(-4.71371668583241,-36.6954831180953,
-8.16439679231297));
#23245=CARTESIAN_POINT('Ctrl Pts',(-7.07057502873392,-36.5204831180953,
-4.082198396148));
#23246=CARTESIAN_POINT('Ctrl Pts',(-9.42743337163542,-36.3454831180953,
1.69768315121407E-11));
#23247=CARTESIAN_POINT('Ctrl Pts',(-7.07057502871922,-36.1704831180953,
4.08219839617346));
#23248=CARTESIAN_POINT('Ctrl Pts',(-4.71371668580301,-35.9954831180953,
8.16439679232994));
#23249=CARTESIAN_POINT('Ctrl Pts',(1.47018674401621E-11,-35.8204831180953,
8.16439679232146));
#23250=CARTESIAN_POINT('Ctrl Pts',(4.71371668583241,-35.6454831180953,8.16439679231297));
#23251=CARTESIAN_POINT('Ctrl Pts',(7.07057502873392,-35.4704831180953,4.082198396148));
#23252=CARTESIAN_POINT('Ctrl Pts',(9.42743337163542,-35.2954831180953,-1.69756769845304E-11));
#23253=CARTESIAN_POINT('Ctrl Pts',(7.07057502871922,-35.1204831180953,-4.08219839617346));
#23254=CARTESIAN_POINT('Ctrl Pts',(4.71371668580301,-34.9454831180953,-8.16439679232994));
#23255=CARTESIAN_POINT('Ctrl Pts',(-1.4702867290402E-11,-34.7704831180953,
-8.16439679232146));
#23256=CARTESIAN_POINT('Ctrl Pts',(-4.71371668583241,-34.5954831180953,
-8.16439679231297));
#23257=CARTESIAN_POINT('Ctrl Pts',(-7.07057502873392,-34.4204831180953,
-4.082198396148));
#23258=CARTESIAN_POINT('Ctrl Pts',(-9.42743337163542,-34.2454831180953,
1.69768315121407E-11));
#23259=CARTESIAN_POINT('Ctrl Pts',(-7.07057502871922,-34.0704831180953,
4.08219839617346));
#23260=CARTESIAN_POINT('Ctrl Pts',(-4.71371668580301,-33.8954831180953,
8.16439679232994));
#23261=CARTESIAN_POINT('Ctrl Pts',(1.47018674401621E-11,-33.7204831180953,
8.16439679232146));
#23262=CARTESIAN_POINT('Ctrl Pts',(4.71371668583241,-33.5454831180953,8.16439679231297));
#23263=CARTESIAN_POINT('Ctrl Pts',(7.07057502873392,-33.3704831180953,4.082198396148));
#23264=CARTESIAN_POINT('Ctrl Pts',(9.42743337163542,-33.1954831180953,-1.69756769845304E-11));
#23265=CARTESIAN_POINT('Ctrl Pts',(7.07057502871922,-33.0204831180953,-4.08219839617346));
#23266=CARTESIAN_POINT('Ctrl Pts',(4.71371668580301,-32.8454831180953,-8.16439679232994));
#23267=CARTESIAN_POINT('Ctrl Pts',(-1.4702867290402E-11,-32.6704831180953,
-8.16439679232146));
#23268=CARTESIAN_POINT('Ctrl Pts',(-4.71371668583241,-32.4954831180953,
-8.16439679231297));
#23269=CARTESIAN_POINT('Ctrl Pts',(-7.07057502873392,-32.3204831180953,
-4.082198396148));
#23270=CARTESIAN_POINT('Ctrl Pts',(-9.42743337163542,-32.1454831180953,
1.69768315121407E-11));
#23271=CARTESIAN_POINT('Ctrl Pts',(-7.07057502871922,-31.9704831180953,
4.08219839617346));
#23272=CARTESIAN_POINT('Ctrl Pts',(-4.71371668580301,-31.7954831180953,
8.16439679232994));
#23273=CARTESIAN_POINT('Ctrl Pts',(1.47018674401621E-11,-31.6204831180953,
8.16439679232146));
#23274=CARTESIAN_POINT('Ctrl Pts',(4.71371668583241,-31.4454831180953,8.16439679231297));
#23275=CARTESIAN_POINT('Ctrl Pts',(7.07057502873392,-31.2704831180953,4.082198396148));
#23276=CARTESIAN_POINT('Ctrl Pts',(9.42743337163542,-31.0954831180953,-1.69756769845304E-11));
#23277=CARTESIAN_POINT('Ctrl Pts',(7.07057502871922,-30.9204831180953,-4.08219839617346));
#23278=CARTESIAN_POINT('Ctrl Pts',(4.71371668580301,-30.7454831180953,-8.16439679232994));
#23279=CARTESIAN_POINT('Ctrl Pts',(-1.4702867290402E-11,-30.5704831180953,
-8.16439679232146));
#23280=CARTESIAN_POINT('Ctrl Pts',(-4.71371668583241,-30.3954831180953,
-8.16439679231297));
#23281=CARTESIAN_POINT('Ctrl Pts',(-7.07057502873392,-30.2204831180953,
-4.082198396148));
#23282=CARTESIAN_POINT('Ctrl Pts',(-9.42743337163542,-30.0454831180953,
1.69768315121407E-11));
#23283=CARTESIAN_POINT('Ctrl Pts',(-7.07057502871922,-29.8704831180953,
4.08219839617346));
#23284=CARTESIAN_POINT('Ctrl Pts',(-4.71371668580301,-29.6954831180953,
8.16439679232994));
#23285=CARTESIAN_POINT('Ctrl Pts',(1.47018674401621E-11,-29.5204831180953,
8.16439679232146));
#23286=CARTESIAN_POINT('Ctrl Pts',(4.71371668583241,-29.3454831180953,8.16439679231297));
#23287=CARTESIAN_POINT('Ctrl Pts',(7.07057502873392,-29.1704831180953,4.082198396148));
#23288=CARTESIAN_POINT('Ctrl Pts',(9.42743337163542,-28.9954831180954,-1.69756769845304E-11));
#23289=CARTESIAN_POINT('Ctrl Pts',(7.07057502871922,-28.8204831180953,-4.08219839617346));
#23290=CARTESIAN_POINT('Ctrl Pts',(4.71371668580301,-28.6454831180953,-8.16439679232994));
#23291=CARTESIAN_POINT('Ctrl Pts',(-1.4702867290402E-11,-28.4704831180953,
-8.16439679232146));
#23292=CARTESIAN_POINT('Ctrl Pts',(-4.71371668583241,-28.2954831180953,
-8.16439679231297));
#23293=CARTESIAN_POINT('Ctrl Pts',(-7.07057502873392,-28.1204831180953,
-4.082198396148));
#23294=CARTESIAN_POINT('Ctrl Pts',(-9.42743337163542,-27.9454831180954,
1.69768315121407E-11));
#23295=CARTESIAN_POINT('Ctrl Pts',(-7.07057502871922,-27.7704831180953,
4.08219839617346));
#23296=CARTESIAN_POINT('Ctrl Pts',(-4.71371668580301,-27.5954831180953,
8.16439679232994));
#23297=CARTESIAN_POINT('Ctrl Pts',(1.47018674401621E-11,-27.4204831180953,
8.16439679232146));
#23298=CARTESIAN_POINT('Ctrl Pts',(4.71371668583241,-27.2454831180954,8.16439679231297));
#23299=CARTESIAN_POINT('Ctrl Pts',(7.07057502873392,-27.0704831180953,4.082198396148));
#23300=CARTESIAN_POINT('Ctrl Pts',(9.42743337163542,-26.8954831180954,-1.69756769845304E-11));
#23301=CARTESIAN_POINT('Ctrl Pts',(7.07057502871922,-26.7204831180953,-4.08219839617346));
#23302=CARTESIAN_POINT('Ctrl Pts',(4.71371668580301,-26.5454831180953,-8.16439679232994));
#23303=CARTESIAN_POINT('Ctrl Pts',(-1.4702867290402E-11,-26.3704831180953,
-8.16439679232146));
#23304=CARTESIAN_POINT('Ctrl Pts',(-4.71371668583241,-26.1954831180954,
-8.16439679231297));
#23305=CARTESIAN_POINT('Ctrl Pts',(-7.07057502873392,-26.0204831180953,
-4.082198396148));
#23306=CARTESIAN_POINT('Ctrl Pts',(-9.42743337163542,-25.8454831180953,
1.69768315121407E-11));
#23307=CARTESIAN_POINT('Ctrl Pts',(-7.07057502871922,-25.6704831180953,
4.08219839617346));
#23308=CARTESIAN_POINT('Ctrl Pts',(-4.71371668580301,-25.4954831180954,
8.16439679232994));
#23309=CARTESIAN_POINT('Ctrl Pts',(1.47018674401621E-11,-25.3204831180953,
8.16439679232146));
#23310=CARTESIAN_POINT('Ctrl Pts',(4.71371668583241,-25.1454831180954,8.16439679231297));
#23311=CARTESIAN_POINT('Ctrl Pts',(7.07057502873392,-24.9704831180954,4.082198396148));
#23312=CARTESIAN_POINT('Ctrl Pts',(9.42743337163542,-24.7954831180953,-1.69756769845304E-11));
#23313=CARTESIAN_POINT('Ctrl Pts',(7.07057502871922,-24.6204831180954,-4.08219839617346));
#23314=CARTESIAN_POINT('Ctrl Pts',(4.71371668580301,-24.4454831180954,-8.16439679232994));
#23315=CARTESIAN_POINT('Ctrl Pts',(-1.4702867290402E-11,-24.2704831180953,
-8.16439679232146));
#23316=CARTESIAN_POINT('Ctrl Pts',(-4.71371668583241,-24.0954831180954,
-8.16439679231297));
#23317=CARTESIAN_POINT('Ctrl Pts',(-7.07057502873392,-23.9204831180953,
-4.082198396148));
#23318=CARTESIAN_POINT('Ctrl Pts',(-9.42743337163542,-23.7454831180954,
1.69768315121407E-11));
#23319=CARTESIAN_POINT('Ctrl Pts',(-7.07057502871922,-23.5704831180954,
4.08219839617346));
#23320=CARTESIAN_POINT('Ctrl Pts',(-4.71371668580301,-23.3954831180954,
8.16439679232994));
#23321=CARTESIAN_POINT('Ctrl Pts',(1.47018674401621E-11,-23.2204831180953,
8.16439679232146));
#23322=CARTESIAN_POINT('Ctrl Pts',(4.71371668583241,-23.0454831180954,8.16439679231297));
#23323=CARTESIAN_POINT('Ctrl Pts',(7.07057502873392,-22.8704831180954,4.082198396148));
#23324=CARTESIAN_POINT('Ctrl Pts',(9.42743337163542,-22.6954831180954,-1.69756769845304E-11));
#23325=CARTESIAN_POINT('Ctrl Pts',(7.07057502871922,-22.5204831180954,-4.08219839617346));
#23326=CARTESIAN_POINT('Ctrl Pts',(4.71371668580301,-22.3454831180954,-8.16439679232994));
#23327=CARTESIAN_POINT('Ctrl Pts',(-1.4702867290402E-11,-22.1704831180954,
-8.16439679232146));
#23328=CARTESIAN_POINT('Ctrl Pts',(-4.71371668583241,-21.9954831180954,
-8.16439679231297));
#23329=CARTESIAN_POINT('Ctrl Pts',(-7.07057502873392,-21.8204831180954,
-4.082198396148));
#23330=CARTESIAN_POINT('Ctrl Pts',(-9.42743337163542,-21.6454831180954,
1.69768315121407E-11));
#23331=CARTESIAN_POINT('Ctrl Pts',(-7.07057502871922,-21.4704831180953,
4.08219839617346));
#23332=CARTESIAN_POINT('Ctrl Pts',(-4.71371668580301,-21.2954831180954,
8.16439679232994));
#23333=CARTESIAN_POINT('Ctrl Pts',(1.47018674401621E-11,-21.1204831180954,
8.16439679232146));
#23334=CARTESIAN_POINT('Ctrl Pts',(4.71371668583241,-20.9454831180954,8.16439679231297));
#23335=CARTESIAN_POINT('Ctrl Pts',(7.07057502873392,-20.7704831180954,4.082198396148));
#23336=CARTESIAN_POINT('Ctrl Pts',(9.42743337163542,-20.5954831180954,-1.69756769845304E-11));
#23337=CARTESIAN_POINT('Ctrl Pts',(7.07057502871922,-20.4204831180954,-4.08219839617346));
#23338=CARTESIAN_POINT('Ctrl Pts',(4.71371668580301,-20.2454831180954,-8.16439679232994));
#23339=CARTESIAN_POINT('Ctrl Pts',(-1.4702867290402E-11,-20.0704831180954,
-8.16439679232146));
#23340=CARTESIAN_POINT('Ctrl Pts',(-4.71371668583241,-19.8954831180954,
-8.16439679231297));
#23341=CARTESIAN_POINT('Ctrl Pts',(-7.07057502873392,-19.7204831180954,
-4.082198396148));
#23342=CARTESIAN_POINT('Ctrl Pts',(-9.42743337163542,-19.5454831180954,
1.69768315121407E-11));
#23343=CARTESIAN_POINT('Ctrl Pts',(-7.07057502871922,-19.3704831180954,
4.08219839617346));
#23344=CARTESIAN_POINT('Ctrl Pts',(-4.71371668580301,-19.1954831180954,
8.16439679232994));
#23345=CARTESIAN_POINT('Ctrl Pts',(1.47018674401621E-11,-19.0204831180954,
8.16439679232146));
#23346=CARTESIAN_POINT('Ctrl Pts',(4.71371668583241,-18.8454831180954,8.16439679231297));
#23347=CARTESIAN_POINT('Ctrl Pts',(7.07057502873392,-18.6704831180954,4.082198396148));
#23348=CARTESIAN_POINT('Ctrl Pts',(9.42743337163542,-18.4954831180954,-1.69756769845304E-11));
#23349=CARTESIAN_POINT('Ctrl Pts',(7.07057502871922,-18.3204831180954,-4.08219839617346));
#23350=CARTESIAN_POINT('Ctrl Pts',(4.71371668580301,-18.1454831180954,-8.16439679232994));
#23351=CARTESIAN_POINT('Ctrl Pts',(-1.4702867290402E-11,-17.9704831180954,
-8.16439679232146));
#23352=CARTESIAN_POINT('Ctrl Pts',(-4.71371668583241,-17.7954831180954,
-8.16439679231297));
#23353=CARTESIAN_POINT('Ctrl Pts',(-7.07057502873392,-17.6204831180954,
-4.082198396148));
#23354=CARTESIAN_POINT('Ctrl Pts',(-9.42743337163542,-17.4454831180954,
1.69768315121407E-11));
#23355=CARTESIAN_POINT('Ctrl Pts',(-7.07057502871922,-17.2704831180954,
4.08219839617346));
#23356=CARTESIAN_POINT('Ctrl Pts',(-4.71371668580301,-17.0954831180954,
8.16439679232994));
#23357=CARTESIAN_POINT('Ctrl Pts',(1.47018674401621E-11,-16.9204831180954,
8.16439679232146));
#23358=CARTESIAN_POINT('Ctrl Pts',(4.71371668583241,-16.7454831180954,8.16439679231297));
#23359=CARTESIAN_POINT('Ctrl Pts',(7.07057502873392,-16.5704831180954,4.082198396148));
#23360=CARTESIAN_POINT('Ctrl Pts',(9.42743337163542,-16.3954831180954,-1.69756769845304E-11));
#23361=CARTESIAN_POINT('Ctrl Pts',(7.07057502871922,-16.2204831180954,-4.08219839617346));
#23362=CARTESIAN_POINT('Ctrl Pts',(4.71371668580301,-16.0454831180954,-8.16439679232994));
#23363=CARTESIAN_POINT('Ctrl Pts',(-1.4702867290402E-11,-15.8704831180954,
-8.16439679232146));
#23364=CARTESIAN_POINT('Ctrl Pts',(-4.71371668583241,-15.6954831180954,
-8.16439679231297));
#23365=CARTESIAN_POINT('Ctrl Pts',(-7.07057502873392,-15.5204831180954,
-4.082198396148));
#23366=CARTESIAN_POINT('Ctrl Pts',(-9.42743337163542,-15.3454831180954,
1.69768315121407E-11));
#23367=CARTESIAN_POINT('Ctrl Pts',(-7.07057502871922,-15.1704831180954,
4.08219839617346));
#23368=CARTESIAN_POINT('Ctrl Pts',(-4.71371668580301,-14.9954831180954,
8.16439679232994));
#23369=CARTESIAN_POINT('Ctrl Pts',(1.47018674401621E-11,-14.8204831180954,
8.16439679232146));
#23370=CARTESIAN_POINT('Ctrl Pts',(4.71371668583241,-14.6454831180954,8.16439679231297));
#23371=CARTESIAN_POINT('Ctrl Pts',(7.07057502873392,-14.4704831180954,4.082198396148));
#23372=CARTESIAN_POINT('Ctrl Pts',(9.42743337163542,-14.2954831180954,-1.69756769845304E-11));
#23373=CARTESIAN_POINT('Ctrl Pts',(7.07057502871922,-14.1204831180954,-4.08219839617346));
#23374=CARTESIAN_POINT('Ctrl Pts',(4.71371668580301,-13.9454831180954,-8.16439679232994));
#23375=CARTESIAN_POINT('Ctrl Pts',(-1.4702867290402E-11,-13.7704831180954,
-8.16439679232146));
#23376=CARTESIAN_POINT('Ctrl Pts',(-4.71371668583241,-13.5954831180954,
-8.16439679231297));
#23377=CARTESIAN_POINT('Ctrl Pts',(-7.07057502873392,-13.4204831180954,
-4.082198396148));
#23378=CARTESIAN_POINT('Ctrl Pts',(-9.42743337163542,-13.2454831180954,
1.69768315121407E-11));
#23379=CARTESIAN_POINT('Ctrl Pts',(-7.07057502871922,-13.0704831180954,
4.08219839617346));
#23380=CARTESIAN_POINT('Ctrl Pts',(-4.71371668580301,-12.8954831180954,
8.16439679232994));
#23381=CARTESIAN_POINT('Ctrl Pts',(1.47018674401621E-11,-12.7204831180954,
8.16439679232146));
#23382=CARTESIAN_POINT('Ctrl Pts',(4.71371668583241,-12.5454831180954,8.16439679231297));
#23383=CARTESIAN_POINT('Ctrl Pts',(7.07057502873392,-12.3704831180954,4.082198396148));
#23384=CARTESIAN_POINT('Ctrl Pts',(9.42743337163542,-12.1954831180954,-1.69756769845304E-11));
#23385=CARTESIAN_POINT('Ctrl Pts',(7.07057502871922,-12.0204831180954,-4.08219839617346));
#23386=CARTESIAN_POINT('Ctrl Pts',(4.71371668580301,-11.8454831180954,-8.16439679232994));
#23387=CARTESIAN_POINT('Ctrl Pts',(-1.4702867290402E-11,-11.6704831180954,
-8.16439679232146));
#23388=CARTESIAN_POINT('Ctrl Pts',(-4.71371668583241,-11.4954831180954,
-8.16439679231297));
#23389=CARTESIAN_POINT('Ctrl Pts',(-7.07057502873392,-11.3204831180954,
-4.082198396148));
#23390=CARTESIAN_POINT('Ctrl Pts',(-9.42743337163542,-11.1454831180954,
1.69768315121407E-11));
#23391=CARTESIAN_POINT('Ctrl Pts',(-7.07057502871922,-10.9704831180954,
4.08219839617346));
#23392=CARTESIAN_POINT('Ctrl Pts',(-4.71371668580301,-10.7954831180954,
8.16439679232994));
#23393=CARTESIAN_POINT('Ctrl Pts',(1.47018674401621E-11,-10.6204831180954,
8.16439679232146));
#23394=CARTESIAN_POINT('Ctrl Pts',(4.71371668583241,-10.4454831180954,8.16439679231297));
#23395=CARTESIAN_POINT('Ctrl Pts',(7.07057502873392,-10.2704831180954,4.082198396148));
#23396=CARTESIAN_POINT('Ctrl Pts',(9.42743337163542,-10.0954831180954,-1.69756769845304E-11));
#23397=CARTESIAN_POINT('Ctrl Pts',(7.07057502871922,-9.92048311809537,-4.08219839617346));
#23398=CARTESIAN_POINT('Ctrl Pts',(4.71371668580301,-9.74548311809539,-8.16439679232994));
#23399=CARTESIAN_POINT('Ctrl Pts',(-1.4702867290402E-11,-9.57048311809539,
-8.16439679232146));
#23400=CARTESIAN_POINT('Ctrl Pts',(-4.71371668583241,-9.39548311809538,
-8.16439679231297));
#23401=CARTESIAN_POINT('Ctrl Pts',(-7.07057502873392,-9.22048311809539,
-4.082198396148));
#23402=CARTESIAN_POINT('Ctrl Pts',(-9.42743337163542,-9.04548311809539,
1.69768315121407E-11));
#23403=CARTESIAN_POINT('Ctrl Pts',(-7.07057502871922,-8.87048311809537,
4.08219839617346));
#23404=CARTESIAN_POINT('Ctrl Pts',(-4.71371668580301,-8.6954831180954,8.16439679232994));
#23405=CARTESIAN_POINT('Ctrl Pts',(1.47018674401621E-11,-8.52048311809539,
8.16439679232146));
#23406=CARTESIAN_POINT('Ctrl Pts',(4.71371668583241,-8.34548311809539,8.16439679231297));
#23407=CARTESIAN_POINT('Ctrl Pts',(7.07057502873392,-8.1704831180954,4.082198396148));
#23408=CARTESIAN_POINT('Ctrl Pts',(9.42743337163542,-7.9954831180954,-1.69756769845304E-11));
#23409=CARTESIAN_POINT('Ctrl Pts',(7.07057502871922,-7.82048311809538,-4.08219839617346));
#23410=CARTESIAN_POINT('Ctrl Pts',(4.71371668580301,-7.64548311809541,-8.16439679232994));
#23411=CARTESIAN_POINT('Ctrl Pts',(-1.4702867290402E-11,-7.47048311809539,
-8.16439679232146));
#23412=CARTESIAN_POINT('Ctrl Pts',(-4.71371668583241,-7.29548311809539,
-8.16439679231297));
#23413=CARTESIAN_POINT('Ctrl Pts',(-7.07057502873392,-7.12048311809538,
-4.082198396148));
#23414=CARTESIAN_POINT('Ctrl Pts',(-9.42743337163542,-6.94548311809541,
1.69768315121407E-11));
#23415=CARTESIAN_POINT('Ctrl Pts',(-7.07057502871922,-6.77048311809538,
4.08219839617346));
#23416=CARTESIAN_POINT('Ctrl Pts',(-4.71371668580301,-6.59548311809539,
8.16439679232994));
#23417=CARTESIAN_POINT('Ctrl Pts',(1.47018674401621E-11,-6.4204831180954,
8.16439679232146));
#23418=CARTESIAN_POINT('Ctrl Pts',(4.71371668583241,-6.24548311809539,8.16439679231297));
#23419=CARTESIAN_POINT('Ctrl Pts',(7.07057502873392,-6.07048311809538,4.082198396148));
#23420=CARTESIAN_POINT('Ctrl Pts',(9.42743337163542,-5.89548311809541,-1.69756769845304E-11));
#23421=CARTESIAN_POINT('Ctrl Pts',(7.07057502871922,-5.72048311809538,-4.08219839617346));
#23422=CARTESIAN_POINT('Ctrl Pts',(4.71371668580301,-5.54548311809539,-8.16439679232994));
#23423=CARTESIAN_POINT('Ctrl Pts',(-1.4702867290402E-11,-5.3704831180954,
-8.16439679232146));
#23424=CARTESIAN_POINT('Ctrl Pts',(-4.71371668583241,-5.19548311809541,
-8.16439679231297));
#23425=CARTESIAN_POINT('Ctrl Pts',(-7.07057502873392,-5.02048311809538,
-4.082198396148));
#23426=CARTESIAN_POINT('Ctrl Pts',(-9.42743337163542,-4.84548311809541,
1.69768315121407E-11));
#23427=CARTESIAN_POINT('Ctrl Pts',(-7.07057502871922,-4.6704831180954,4.08219839617346));
#23428=CARTESIAN_POINT('Ctrl Pts',(-4.71371668580301,-4.49548311809539,
8.16439679232994));
#23429=CARTESIAN_POINT('Ctrl Pts',(1.47018674401621E-11,-4.3204831180954,
8.16439679232146));
#23430=CARTESIAN_POINT('Ctrl Pts',(4.71371668583241,-4.14548311809541,8.16439679231297));
#23431=CARTESIAN_POINT('Ctrl Pts',(7.07057502873392,-3.97048311809539,4.082198396148));
#23432=CARTESIAN_POINT('Ctrl Pts',(9.42743337163542,-3.79548311809541,-1.69756769845304E-11));
#23433=CARTESIAN_POINT('Ctrl Pts',(7.07057502871922,-3.6204831180954,-4.08219839617346));
#23434=CARTESIAN_POINT('Ctrl Pts',(4.71371668580301,-3.44548311809539,-8.16439679232994));
#23435=CARTESIAN_POINT('Ctrl Pts',(-1.4702867290402E-11,-3.27048311809541,
-8.16439679232146));
#23436=CARTESIAN_POINT('Ctrl Pts',(-4.71371668583241,-3.09548311809541,
-8.16439679231297));
#23437=CARTESIAN_POINT('Ctrl Pts',(-7.07057502873392,-2.92048311809539,
-4.082198396148));
#23438=CARTESIAN_POINT('Ctrl Pts',(-9.42743337163542,-2.74548311809539,
1.69768315121407E-11));
#23439=CARTESIAN_POINT('Ctrl Pts',(-7.07057502871922,-2.5704831180954,4.08219839617346));
#23440=CARTESIAN_POINT('Ctrl Pts',(-4.71371668580301,-2.3954831180954,8.16439679232994));
#23441=CARTESIAN_POINT('Ctrl Pts',(1.47018674401621E-11,-2.22048311809539,
8.16439679232146));
#23442=CARTESIAN_POINT('Ctrl Pts',(4.71371668583241,-2.04548311809541,8.16439679231297));
#23443=CARTESIAN_POINT('Ctrl Pts',(7.07057502873392,-1.87048311809539,4.082198396148));
#23444=CARTESIAN_POINT('Ctrl Pts',(9.42743337163542,-1.69548311809539,-1.69756769845304E-11));
#23445=CARTESIAN_POINT('Ctrl Pts',(7.07057502871922,-1.52048311809541,-4.08219839617346));
#23446=CARTESIAN_POINT('Ctrl Pts',(4.71371668580301,-1.34548311809541,-8.16439679232994));
#23447=CARTESIAN_POINT('Ctrl Pts',(-1.4702867290402E-11,-1.17048311809539,
-8.16439679232146));
#23448=CARTESIAN_POINT('Ctrl Pts',(-4.71371668583241,-0.995483118095416,
-8.16439679231297));
#23449=CARTESIAN_POINT('Ctrl Pts',(-7.07057502873392,-0.820483118095406,
-4.082198396148));
#23450=CARTESIAN_POINT('Ctrl Pts',(-9.42743337163542,-0.645483118095396,
1.69768315121407E-11));
#23451=CARTESIAN_POINT('Ctrl Pts',(-7.07057502871922,-0.47048311809541,
4.08219839617346));
#23452=CARTESIAN_POINT('Ctrl Pts',(-4.71371668580301,-0.295483118095414,
8.16439679232994));
#23453=CARTESIAN_POINT('Ctrl Pts',(1.47018674401621E-11,-0.120483118095393,
8.16439679232146));
#23454=CARTESIAN_POINT('Ctrl Pts',(4.71371668583241,0.054516881904581,8.16439679231297));
#23455=CARTESIAN_POINT('Ctrl Pts',(7.07057502873392,0.229516881904591,4.082198396148));
#23456=CARTESIAN_POINT('Ctrl Pts',(9.42743337163542,0.404516881904601,-1.69756769845304E-11));
#23457=CARTESIAN_POINT('Ctrl Pts',(7.07057502871922,0.579516881904587,-4.08219839617346));
#23458=CARTESIAN_POINT('Ctrl Pts',(4.71371668580301,0.754516881904583,-8.16439679232994));
#23459=CARTESIAN_POINT('Ctrl Pts',(-1.4702867290402E-11,0.929516881904604,
-8.16439679232146));
#23460=CARTESIAN_POINT('Ctrl Pts',(-4.71371668583241,1.10451688190458,-8.16439679231297));
#23461=CARTESIAN_POINT('Ctrl Pts',(-7.07057502873392,1.27951688190459,-4.082198396148));
#23462=CARTESIAN_POINT('Ctrl Pts',(-9.42743337163542,1.4545168819046,1.69768315121407E-11));
#23463=CARTESIAN_POINT('Ctrl Pts',(-7.07057502871922,1.62951688190461,4.08219839617346));
#23464=CARTESIAN_POINT('Ctrl Pts',(-4.71371668580301,1.80451688190458,8.16439679232994));
#23465=CARTESIAN_POINT('Ctrl Pts',(1.47018674401621E-11,1.9795168819046,
8.16439679232146));
#23466=CARTESIAN_POINT('Ctrl Pts',(4.71371668583241,2.1545168819046,8.16439679231297));
#23467=CARTESIAN_POINT('Ctrl Pts',(7.07057502873392,2.32951688190458,4.082198396148));
#23468=CARTESIAN_POINT('Ctrl Pts',(9.42743337163542,2.50451688190458,-1.69756769845304E-11));
#23469=CARTESIAN_POINT('Ctrl Pts',(7.07057502871922,2.6795168819046,-4.08219839617346));
#23470=CARTESIAN_POINT('Ctrl Pts',(4.71371668580301,2.85451688190458,-8.16439679232994));
#23471=CARTESIAN_POINT('Ctrl Pts',(-1.4702867290402E-11,3.02951688190459,
-8.16439679232146));
#23472=CARTESIAN_POINT('Ctrl Pts',(-4.71371668583241,3.2045168819046,-8.16439679231297));
#23473=CARTESIAN_POINT('Ctrl Pts',(-7.07057502873392,3.37951688190458,-4.082198396148));
#23474=CARTESIAN_POINT('Ctrl Pts',(-9.42743337163542,3.55451688190458,1.69768315121407E-11));
#23475=CARTESIAN_POINT('Ctrl Pts',(-7.07057502871922,3.7295168819046,4.08219839617346));
#23476=CARTESIAN_POINT('Ctrl Pts',(-4.71371668580301,3.90451688190458,8.16439679232994));
#23477=CARTESIAN_POINT('Ctrl Pts',(1.47018674401621E-11,4.07951688190458,
8.16439679232146));
#23478=CARTESIAN_POINT('Ctrl Pts',(4.71371668583241,4.2545168819046,8.16439679231297));
#23479=CARTESIAN_POINT('Ctrl Pts',(7.07057502873392,4.42951688190458,4.082198396148));
#23480=CARTESIAN_POINT('Ctrl Pts',(9.42743337163542,4.60451688190458,-1.69756769845304E-11));
#23481=CARTESIAN_POINT('Ctrl Pts',(7.07057502871922,4.7795168819046,-4.08219839617346));
#23482=CARTESIAN_POINT('Ctrl Pts',(4.71371668580301,4.95451688190457,-8.16439679232994));
#23483=CARTESIAN_POINT('Ctrl Pts',(-1.4702867290402E-11,5.12951688190458,
-8.16439679232146));
#23484=CARTESIAN_POINT('Ctrl Pts',(-4.71371668583241,5.30451688190459,-8.16439679231297));
#23485=CARTESIAN_POINT('Ctrl Pts',(-7.07057502873392,5.47951688190458,-4.082198396148));
#23486=CARTESIAN_POINT('Ctrl Pts',(-9.42743337163542,5.65451688190458,1.69768315121407E-11));
#23487=CARTESIAN_POINT('Ctrl Pts',(-7.07057502871922,5.82951688190459,4.08219839617346));
#23488=CARTESIAN_POINT('Ctrl Pts',(-4.71371668580301,6.00451688190457,8.16439679232994));
#23489=CARTESIAN_POINT('Ctrl Pts',(1.47018674401621E-11,6.17951688190458,
8.16439679232146));
#23490=CARTESIAN_POINT('Ctrl Pts',(4.71371668583241,6.35451688190459,8.16439679231297));
#23491=CARTESIAN_POINT('Ctrl Pts',(7.07057502873392,6.52951688190459,4.082198396148));
#23492=CARTESIAN_POINT('Ctrl Pts',(9.42743337163542,6.70451688190457,-1.69756769845304E-11));
#23493=CARTESIAN_POINT('Ctrl Pts',(7.07057502871922,6.87951688190458,-4.08219839617346));
#23494=CARTESIAN_POINT('Ctrl Pts',(4.71371668580301,7.05451688190459,-8.16439679232994));
#23495=CARTESIAN_POINT('Ctrl Pts',(-1.4702867290402E-11,7.22951688190457,
-8.16439679232146));
#23496=CARTESIAN_POINT('Ctrl Pts',(-4.71371668583241,7.40451688190458,-8.16439679231297));
#23497=CARTESIAN_POINT('Ctrl Pts',(-7.07057502873392,7.57951688190459,-4.082198396148));
#23498=CARTESIAN_POINT('Ctrl Pts',(-9.42743337163542,7.75451688190457,1.69768315121407E-11));
#23499=CARTESIAN_POINT('Ctrl Pts',(-7.07057502871922,7.92951688190458,4.08219839617346));
#23500=CARTESIAN_POINT('Ctrl Pts',(-4.71371668580301,8.10451688190458,8.16439679232994));
#23501=CARTESIAN_POINT('Ctrl Pts',(1.47018674401621E-11,8.27951688190457,
8.16439679232146));
#23502=CARTESIAN_POINT('Ctrl Pts',(4.71371668583241,8.45451688190457,8.16439679231297));
#23503=CARTESIAN_POINT('Ctrl Pts',(7.07057502873392,8.62951688190459,4.082198396148));
#23504=CARTESIAN_POINT('Ctrl Pts',(9.42743337163542,8.80451688190457,-1.69756769845304E-11));
#23505=CARTESIAN_POINT('Ctrl Pts',(7.07057502871922,8.97951688190457,-4.08219839617346));
#23506=CARTESIAN_POINT('Ctrl Pts',(4.71371668580301,9.15451688190458,-8.16439679232994));
#23507=CARTESIAN_POINT('Ctrl Pts',(-1.4702867290402E-11,9.32951688190457,
-8.16439679232146));
#23508=CARTESIAN_POINT('Ctrl Pts',(-4.71371668583241,9.50451688190457,-8.16439679231297));
#23509=CARTESIAN_POINT('Ctrl Pts',(-7.07057502873392,9.67951688190458,-4.082198396148));
#23510=CARTESIAN_POINT('Ctrl Pts',(-9.42743337163542,9.85451688190457,1.69768315121407E-11));
#23511=CARTESIAN_POINT('Ctrl Pts',(-7.07057502871922,10.0295168819046,4.08219839617346));
#23512=CARTESIAN_POINT('Ctrl Pts',(-4.71371668580301,10.2045168819046,8.16439679232994));
#23513=CARTESIAN_POINT('Ctrl Pts',(1.47018674401621E-11,10.3795168819046,
8.16439679232146));
#23514=CARTESIAN_POINT('Ctrl Pts',(4.71371668583241,10.5545168819046,8.16439679231297));
#23515=CARTESIAN_POINT('Ctrl Pts',(7.07057502873392,10.7295168819046,4.082198396148));
#23516=CARTESIAN_POINT('Ctrl Pts',(9.42743337163542,10.9045168819046,-1.69756769845304E-11));
#23517=CARTESIAN_POINT('Ctrl Pts',(7.07057502871922,11.0795168819046,-4.08219839617346));
#23518=CARTESIAN_POINT('Ctrl Pts',(4.71371668580301,11.2545168819046,-8.16439679232994));
#23519=CARTESIAN_POINT('Ctrl Pts',(-1.4702867290402E-11,11.4295168819046,
-8.16439679232146));
#23520=CARTESIAN_POINT('Ctrl Pts',(-4.71371668583241,11.6045168819046,-8.16439679231297));
#23521=CARTESIAN_POINT('Ctrl Pts',(-7.07057502873392,11.7795168819046,-4.082198396148));
#23522=CARTESIAN_POINT('Ctrl Pts',(-9.42743337163542,11.9545168819046,1.69768315121407E-11));
#23523=CARTESIAN_POINT('Ctrl Pts',(-7.07057502871922,12.1295168819046,4.08219839617346));
#23524=CARTESIAN_POINT('Ctrl Pts',(-4.71371668580301,12.3045168819046,8.16439679232994));
#23525=CARTESIAN_POINT('Ctrl Pts',(1.47018674401621E-11,12.4795168819046,
8.16439679232146));
#23526=CARTESIAN_POINT('Ctrl Pts',(4.71371668583241,12.6545168819046,8.16439679231297));
#23527=CARTESIAN_POINT('Ctrl Pts',(7.07057502873392,12.8295168819046,4.082198396148));
#23528=CARTESIAN_POINT('Ctrl Pts',(9.42743337163542,13.0045168819046,-1.69756769845304E-11));
#23529=CARTESIAN_POINT('Ctrl Pts',(7.07057502871922,13.1795168819046,-4.08219839617346));
#23530=CARTESIAN_POINT('Ctrl Pts',(4.71371668580301,13.3545168819046,-8.16439679232994));
#23531=CARTESIAN_POINT('Ctrl Pts',(-1.4702867290402E-11,13.5295168819046,
-8.16439679232146));
#23532=CARTESIAN_POINT('Ctrl Pts',(-4.71371668583241,13.7045168819046,-8.16439679231297));
#23533=CARTESIAN_POINT('Ctrl Pts',(-7.07057502873392,13.8795168819046,-4.082198396148));
#23534=CARTESIAN_POINT('Ctrl Pts',(-9.42743337163542,14.0545168819046,1.69768315121407E-11));
#23535=CARTESIAN_POINT('Ctrl Pts',(-7.07057502871922,14.2295168819046,4.08219839617346));
#23536=CARTESIAN_POINT('Ctrl Pts',(-4.71371668580301,14.4045168819046,8.16439679232994));
#23537=CARTESIAN_POINT('Ctrl Pts',(1.47018674401621E-11,14.5795168819046,
8.16439679232146));
#23538=CARTESIAN_POINT('Ctrl Pts',(4.71371668583241,14.7545168819045,8.16439679231297));
#23539=CARTESIAN_POINT('Ctrl Pts',(7.07057502873392,14.9295168819046,4.082198396148));
#23540=CARTESIAN_POINT('Ctrl Pts',(9.42743337163542,15.1045168819046,-1.69756769845304E-11));
#23541=CARTESIAN_POINT('Ctrl Pts',(7.07057502871922,15.2795168819046,-4.08219839617346));
#23542=CARTESIAN_POINT('Ctrl Pts',(4.71371668580301,15.4545168819046,-8.16439679232994));
#23543=CARTESIAN_POINT('Ctrl Pts',(-1.4702867290402E-11,15.6295168819046,
-8.16439679232146));
#23544=CARTESIAN_POINT('Ctrl Pts',(-4.71371668583241,15.8045168819046,-8.16439679231297));
#23545=CARTESIAN_POINT('Ctrl Pts',(-7.07057502873392,15.9795168819046,-4.082198396148));
#23546=CARTESIAN_POINT('Ctrl Pts',(-9.42743337163542,16.1545168819046,1.69768315121407E-11));
#23547=CARTESIAN_POINT('Ctrl Pts',(-7.07057502871922,16.3295168819046,4.08219839617346));
#23548=CARTESIAN_POINT('Ctrl Pts',(-4.71371668580301,16.5045168819046,8.16439679232994));
#23549=CARTESIAN_POINT('Ctrl Pts',(1.47018674401621E-11,16.6795168819046,
8.16439679232146));
#23550=CARTESIAN_POINT('Ctrl Pts',(4.71371668583241,16.8545168819046,8.16439679231297));
#23551=CARTESIAN_POINT('Ctrl Pts',(7.07057502873392,17.0295168819046,4.082198396148));
#23552=CARTESIAN_POINT('Ctrl Pts',(9.42743337163542,17.2045168819045,-1.69756769845304E-11));
#23553=CARTESIAN_POINT('Ctrl Pts',(7.07057502871922,17.3795168819046,-4.08219839617346));
#23554=CARTESIAN_POINT('Ctrl Pts',(4.71371668580301,17.5545168819045,-8.16439679232994));
#23555=CARTESIAN_POINT('Ctrl Pts',(-1.4702867290402E-11,17.7295168819046,
-8.16439679232146));
#23556=CARTESIAN_POINT('Ctrl Pts',(-4.71371668583241,17.9045168819046,-8.16439679231297));
#23557=CARTESIAN_POINT('Ctrl Pts',(-7.07057502873392,18.0795168819045,-4.082198396148));
#23558=CARTESIAN_POINT('Ctrl Pts',(-9.42743337163542,18.2545168819045,1.69768315121407E-11));
#23559=CARTESIAN_POINT('Ctrl Pts',(-7.07057502871922,18.4295168819046,4.08219839617346));
#23560=CARTESIAN_POINT('Ctrl Pts',(-4.71371668580301,18.6045168819045,8.16439679232994));
#23561=CARTESIAN_POINT('Ctrl Pts',(1.47018674401621E-11,18.7795168819046,
8.16439679232146));
#23562=CARTESIAN_POINT('Ctrl Pts',(4.71371668583241,18.9545168819045,8.16439679231297));
#23563=CARTESIAN_POINT('Ctrl Pts',(7.07057502873392,19.1295168819045,4.082198396148));
#23564=CARTESIAN_POINT('Ctrl Pts',(9.42743337163542,19.3045168819045,-1.69756769845304E-11));
#23565=CARTESIAN_POINT('Ctrl Pts',(7.07057502871922,19.4795168819046,-4.08219839617346));
#23566=CARTESIAN_POINT('Ctrl Pts',(4.71371668580301,19.6545168819046,-8.16439679232994));
#23567=CARTESIAN_POINT('Ctrl Pts',(-1.4702867290402E-11,19.8295168819045,
-8.16439679232146));
#23568=CARTESIAN_POINT('Ctrl Pts',(-4.71371668583241,20.0045168819045,-8.16439679231297));
#23569=CARTESIAN_POINT('Ctrl Pts',(-7.07057502873392,20.1795168819046,-4.082198396148));
#23570=CARTESIAN_POINT('Ctrl Pts',(-9.42743337163542,20.3545168819045,1.69768315121407E-11));
#23571=CARTESIAN_POINT('Ctrl Pts',(-7.07057502871922,20.5295168819046,4.08219839617346));
#23572=CARTESIAN_POINT('Ctrl Pts',(-4.71371668580301,20.7045168819046,8.16439679232994));
#23573=CARTESIAN_POINT('Ctrl Pts',(1.47018674401621E-11,20.8795168819045,
8.16439679232146));
#23574=CARTESIAN_POINT('Ctrl Pts',(4.71371668583241,21.0545168819045,8.16439679231297));
#23575=CARTESIAN_POINT('Ctrl Pts',(7.07057502873392,21.2295168819046,4.082198396148));
#23576=CARTESIAN_POINT('Ctrl Pts',(9.42743337163542,21.4045168819045,-1.69756769845304E-11));
#23577=CARTESIAN_POINT('Ctrl Pts',(7.07057502871922,21.5795168819045,-4.08219839617346));
#23578=CARTESIAN_POINT('Ctrl Pts',(4.71371668580301,21.7545168819045,-8.16439679232994));
#23579=CARTESIAN_POINT('Ctrl Pts',(-1.4702867290402E-11,21.9295168819045,
-8.16439679232146));
#23580=CARTESIAN_POINT('Ctrl Pts',(-4.71371668583241,22.1045168819045,-8.16439679231297));
#23581=CARTESIAN_POINT('Ctrl Pts',(-7.07057502873392,22.2795168819046,-4.082198396148));
#23582=CARTESIAN_POINT('Ctrl Pts',(-9.42743337163542,22.4545168819045,1.69768315121407E-11));
#23583=CARTESIAN_POINT('Ctrl Pts',(-7.07057502871922,22.6295168819045,4.08219839617346));
#23584=CARTESIAN_POINT('Ctrl Pts',(-4.71371668580301,22.8045168819045,8.16439679232994));
#23585=CARTESIAN_POINT('Ctrl Pts',(1.47018674401621E-11,22.9795168819045,
8.16439679232146));
#23586=CARTESIAN_POINT('Ctrl Pts',(4.71371668583241,23.1545168819045,8.16439679231297));
#23587=CARTESIAN_POINT('Ctrl Pts',(7.07057502873392,23.3295168819046,4.082198396148));
#23588=CARTESIAN_POINT('Ctrl Pts',(9.42743337163542,23.5045168819045,-1.69756769845304E-11));
#23589=CARTESIAN_POINT('Ctrl Pts',(7.07057502871922,23.6795168819045,-4.08219839617346));
#23590=CARTESIAN_POINT('Ctrl Pts',(4.71371668580301,23.8545168819045,-8.16439679232994));
#23591=CARTESIAN_POINT('Ctrl Pts',(-1.4702867290402E-11,24.0295168819045,
-8.16439679232146));
#23592=CARTESIAN_POINT('Ctrl Pts',(-4.71371668583241,24.2045168819045,-8.16439679231297));
#23593=CARTESIAN_POINT('Ctrl Pts',(-7.07057502873392,24.3795168819046,-4.082198396148));
#23594=CARTESIAN_POINT('Ctrl Pts',(-9.42743337163542,24.5545168819046,1.69768315121407E-11));
#23595=CARTESIAN_POINT('Ctrl Pts',(-7.07057502871922,24.7295168819045,4.08219839617346));
#23596=CARTESIAN_POINT('Ctrl Pts',(-4.71371668580301,24.9045168819045,8.16439679232994));
#23597=CARTESIAN_POINT('Ctrl Pts',(1.47018674401621E-11,25.0795168819046,
8.16439679232146));
#23598=CARTESIAN_POINT('Ctrl Pts',(4.71371668583241,25.2545168819045,8.16439679231297));
#23599=CARTESIAN_POINT('Ctrl Pts',(7.07057502873392,25.4295168819045,4.082198396148));
#23600=CARTESIAN_POINT('Ctrl Pts',(9.42743337163542,25.6045168819045,-1.69756769845304E-11));
#23601=CARTESIAN_POINT('Ctrl Pts',(7.07057502871922,25.7795168819045,-4.08219839617346));
#23602=CARTESIAN_POINT('Ctrl Pts',(4.71371668580301,25.9545168819045,-8.16439679232994));
#23603=CARTESIAN_POINT('Ctrl Pts',(-1.4702867290402E-11,26.1295168819045,
-8.16439679232146));
#23604=CARTESIAN_POINT('Ctrl Pts',(-1.4702867290402E-11,-143.703019107145,
-8.16439679232146));
#23605=CARTESIAN_POINT('Ctrl Pts',(-4.71371668583241,-143.528019107145,
-8.16439679231297));
#23606=CARTESIAN_POINT('Ctrl Pts',(-7.07057502873392,-143.353019107145,
-4.082198396148));
#23607=CARTESIAN_POINT('Ctrl Pts',(-9.42743337163542,-143.178019107145,
1.69768315121407E-11));
#23608=CARTESIAN_POINT('Ctrl Pts',(-7.07057502871922,-143.003019107145,
4.08219839617346));
#23609=CARTESIAN_POINT('Ctrl Pts',(-4.71371668580301,-142.828019107145,
8.16439679232994));
#23610=CARTESIAN_POINT('Ctrl Pts',(1.47018674401621E-11,-142.653019107145,
8.16439679232146));
#23611=CARTESIAN_POINT('Ctrl Pts',(4.71371668583241,-142.478019107145,8.16439679231297));
#23612=CARTESIAN_POINT('Ctrl Pts',(7.07057502873392,-142.303019107145,4.082198396148));
#23613=CARTESIAN_POINT('Ctrl Pts',(9.42743337163542,-142.128019107145,-1.69756769845304E-11));
#23614=CARTESIAN_POINT('Ctrl Pts',(7.07057502871922,-141.953019107145,-4.08219839617346));
#23615=CARTESIAN_POINT('Ctrl Pts',(4.71371668580301,-141.778019107145,-8.16439679232994));
#23616=CARTESIAN_POINT('Ctrl Pts',(-1.4702867290402E-11,-141.603019107145,
-8.16439679232146));
#23617=CARTESIAN_POINT('Ctrl Pts',(-4.71371668583241,-141.428019107145,
-8.16439679231297));
#23618=CARTESIAN_POINT('Ctrl Pts',(-7.07057502873392,-141.253019107145,
-4.082198396148));
#23619=CARTESIAN_POINT('Ctrl Pts',(-9.42743337163542,-141.078019107145,
1.69768315121407E-11));
#23620=CARTESIAN_POINT('Ctrl Pts',(-7.07057502871922,-140.903019107145,
4.08219839617346));
#23621=CARTESIAN_POINT('Ctrl Pts',(-4.71371668580301,-140.728019107145,
8.16439679232994));
#23622=CARTESIAN_POINT('Ctrl Pts',(1.47018674401621E-11,-140.553019107145,
8.16439679232146));
#23623=CARTESIAN_POINT('Ctrl Pts',(4.71371668583241,-140.378019107145,8.16439679231297));
#23624=CARTESIAN_POINT('Ctrl Pts',(7.07057502873392,-140.203019107145,4.082198396148));
#23625=CARTESIAN_POINT('Ctrl Pts',(9.42743337163542,-140.028019107145,-1.69756769845304E-11));
#23626=CARTESIAN_POINT('Ctrl Pts',(7.07057502871922,-139.853019107145,-4.08219839617346));
#23627=CARTESIAN_POINT('Ctrl Pts',(4.71371668580301,-139.678019107145,-8.16439679232994));
#23628=CARTESIAN_POINT('Ctrl Pts',(-1.4702867290402E-11,-139.503019107145,
-8.16439679232146));
#23629=CARTESIAN_POINT('Ctrl Pts',(-4.71371668583241,-139.328019107145,
-8.16439679231297));
#23630=CARTESIAN_POINT('Ctrl Pts',(-7.07057502873392,-139.153019107145,
-4.082198396148));
#23631=CARTESIAN_POINT('Ctrl Pts',(-9.42743337163542,-138.978019107145,
1.69768315121407E-11));
#23632=CARTESIAN_POINT('Ctrl Pts',(-7.07057502871922,-138.803019107145,
4.08219839617346));
#23633=CARTESIAN_POINT('Ctrl Pts',(-4.71371668580301,-138.628019107145,
8.16439679232994));
#23634=CARTESIAN_POINT('Ctrl Pts',(1.47018674401621E-11,-138.453019107145,
8.16439679232146));
#23635=CARTESIAN_POINT('Ctrl Pts',(4.71371668583241,-138.278019107145,8.16439679231297));
#23636=CARTESIAN_POINT('Ctrl Pts',(7.07057502873392,-138.103019107145,4.082198396148));
#23637=CARTESIAN_POINT('Ctrl Pts',(9.42743337163542,-137.928019107145,-1.69756769845304E-11));
#23638=CARTESIAN_POINT('Ctrl Pts',(7.07057502871922,-137.753019107145,-4.08219839617346));
#23639=CARTESIAN_POINT('Ctrl Pts',(4.71371668580301,-137.578019107145,-8.16439679232994));
#23640=CARTESIAN_POINT('Ctrl Pts',(-1.4702867290402E-11,-137.403019107145,
-8.16439679232146));
#23641=CARTESIAN_POINT('Ctrl Pts',(-4.71371668583241,-137.228019107145,
-8.16439679231297));
#23642=CARTESIAN_POINT('Ctrl Pts',(-7.07057502873392,-137.053019107145,
-4.082198396148));
#23643=CARTESIAN_POINT('Ctrl Pts',(-9.42743337163542,-136.878019107145,
1.69768315121407E-11));
#23644=CARTESIAN_POINT('Ctrl Pts',(-7.07057502871922,-136.703019107145,
4.08219839617346));
#23645=CARTESIAN_POINT('Ctrl Pts',(-4.71371668580301,-136.528019107145,
8.16439679232994));
#23646=CARTESIAN_POINT('Ctrl Pts',(1.47018674401621E-11,-136.353019107145,
8.16439679232146));
#23647=CARTESIAN_POINT('Ctrl Pts',(4.71371668583241,-136.178019107145,8.16439679231297));
#23648=CARTESIAN_POINT('Ctrl Pts',(7.07057502873392,-136.003019107145,4.082198396148));
#23649=CARTESIAN_POINT('Ctrl Pts',(9.42743337163542,-135.828019107145,-1.69756769845304E-11));
#23650=CARTESIAN_POINT('Ctrl Pts',(7.07057502871922,-135.653019107145,-4.08219839617346));
#23651=CARTESIAN_POINT('Ctrl Pts',(4.71371668580301,-135.478019107145,-8.16439679232994));
#23652=CARTESIAN_POINT('Ctrl Pts',(-1.4702867290402E-11,-135.303019107145,
-8.16439679232146));
#23653=CARTESIAN_POINT('Ctrl Pts',(-4.71371668583241,-135.128019107145,
-8.16439679231297));
#23654=CARTESIAN_POINT('Ctrl Pts',(-7.07057502873392,-134.953019107145,
-4.082198396148));
#23655=CARTESIAN_POINT('Ctrl Pts',(-9.42743337163542,-134.778019107145,
1.69768315121407E-11));
#23656=CARTESIAN_POINT('Ctrl Pts',(-7.07057502871922,-134.603019107145,
4.08219839617346));
#23657=CARTESIAN_POINT('Ctrl Pts',(-4.71371668580301,-134.428019107145,
8.16439679232994));
#23658=CARTESIAN_POINT('Ctrl Pts',(1.47018674401621E-11,-134.253019107145,
8.16439679232146));
#23659=CARTESIAN_POINT('Ctrl Pts',(4.71371668583241,-134.078019107145,8.16439679231297));
#23660=CARTESIAN_POINT('Ctrl Pts',(7.07057502873392,-133.903019107145,4.082198396148));
#23661=CARTESIAN_POINT('Ctrl Pts',(9.42743337163542,-133.728019107145,-1.69756769845304E-11));
#23662=CARTESIAN_POINT('Ctrl Pts',(7.07057502871922,-133.553019107145,-4.08219839617346));
#23663=CARTESIAN_POINT('Ctrl Pts',(4.71371668580301,-133.378019107145,-8.16439679232994));
#23664=CARTESIAN_POINT('Ctrl Pts',(-1.4702867290402E-11,-133.203019107145,
-8.16439679232146));
#23665=CARTESIAN_POINT('Ctrl Pts',(-4.71371668583241,-133.028019107145,
-8.16439679231297));
#23666=CARTESIAN_POINT('Ctrl Pts',(-7.07057502873392,-132.853019107145,
-4.082198396148));
#23667=CARTESIAN_POINT('Ctrl Pts',(-9.42743337163542,-132.678019107145,
1.69768315121407E-11));
#23668=CARTESIAN_POINT('Ctrl Pts',(-7.07057502871922,-132.503019107145,
4.08219839617346));
#23669=CARTESIAN_POINT('Ctrl Pts',(-4.71371668580301,-132.328019107145,
8.16439679232994));
#23670=CARTESIAN_POINT('Ctrl Pts',(1.47018674401621E-11,-132.153019107145,
8.16439679232146));
#23671=CARTESIAN_POINT('Ctrl Pts',(4.71371668583241,-131.978019107145,8.16439679231297));
#23672=CARTESIAN_POINT('Ctrl Pts',(7.07057502873392,-131.803019107145,4.082198396148));
#23673=CARTESIAN_POINT('Ctrl Pts',(9.42743337163542,-131.628019107145,-1.69756769845304E-11));
#23674=CARTESIAN_POINT('Ctrl Pts',(7.07057502871922,-131.453019107145,-4.08219839617346));
#23675=CARTESIAN_POINT('Ctrl Pts',(4.71371668580301,-131.278019107145,-8.16439679232994));
#23676=CARTESIAN_POINT('Ctrl Pts',(-1.4702867290402E-11,-131.103019107145,
-8.16439679232146));
#23677=CARTESIAN_POINT('Ctrl Pts',(-4.71371668583241,-130.928019107145,
-8.16439679231297));
#23678=CARTESIAN_POINT('Ctrl Pts',(-7.07057502873392,-130.753019107145,
-4.082198396148));
#23679=CARTESIAN_POINT('Ctrl Pts',(-9.42743337163542,-130.578019107145,
1.69768315121407E-11));
#23680=CARTESIAN_POINT('Ctrl Pts',(-7.07057502871922,-130.403019107145,
4.08219839617346));
#23681=CARTESIAN_POINT('Ctrl Pts',(-4.71371668580301,-130.228019107145,
8.16439679232994));
#23682=CARTESIAN_POINT('Ctrl Pts',(1.47018674401621E-11,-130.053019107145,
8.16439679232146));
#23683=CARTESIAN_POINT('Ctrl Pts',(4.71371668583241,-129.878019107145,8.16439679231297));
#23684=CARTESIAN_POINT('Ctrl Pts',(7.07057502873392,-129.703019107145,4.082198396148));
#23685=CARTESIAN_POINT('Ctrl Pts',(9.42743337163542,-129.528019107145,-1.69756769845304E-11));
#23686=CARTESIAN_POINT('Ctrl Pts',(7.07057502871922,-129.353019107145,-4.08219839617346));
#23687=CARTESIAN_POINT('Ctrl Pts',(4.71371668580301,-129.178019107145,-8.16439679232994));
#23688=CARTESIAN_POINT('Ctrl Pts',(-1.4702867290402E-11,-129.003019107145,
-8.16439679232146));
#23689=CARTESIAN_POINT('Ctrl Pts',(-4.71371668583241,-128.828019107145,
-8.16439679231297));
#23690=CARTESIAN_POINT('Ctrl Pts',(-7.07057502873392,-128.653019107145,
-4.082198396148));
#23691=CARTESIAN_POINT('Ctrl Pts',(-9.42743337163542,-128.478019107145,
1.69768315121407E-11));
#23692=CARTESIAN_POINT('Ctrl Pts',(-7.07057502871922,-128.303019107145,
4.08219839617346));
#23693=CARTESIAN_POINT('Ctrl Pts',(-4.71371668580301,-128.128019107145,
8.16439679232994));
#23694=CARTESIAN_POINT('Ctrl Pts',(1.47018674401621E-11,-127.953019107145,
8.16439679232146));
#23695=CARTESIAN_POINT('Ctrl Pts',(4.71371668583241,-127.778019107145,8.16439679231297));
#23696=CARTESIAN_POINT('Ctrl Pts',(7.07057502873392,-127.603019107145,4.082198396148));
#23697=CARTESIAN_POINT('Ctrl Pts',(9.42743337163542,-127.428019107145,-1.69756769845304E-11));
#23698=CARTESIAN_POINT('Ctrl Pts',(7.07057502871922,-127.253019107145,-4.08219839617346));
#23699=CARTESIAN_POINT('Ctrl Pts',(4.71371668580301,-127.078019107145,-8.16439679232994));
#23700=CARTESIAN_POINT('Ctrl Pts',(-1.4702867290402E-11,-126.903019107145,
-8.16439679232146));
#23701=CARTESIAN_POINT('Ctrl Pts',(-4.71371668583241,-126.728019107145,
-8.16439679231297));
#23702=CARTESIAN_POINT('Ctrl Pts',(-7.07057502873392,-126.553019107145,
-4.082198396148));
#23703=CARTESIAN_POINT('Ctrl Pts',(-9.42743337163542,-126.378019107145,
1.69768315121407E-11));
#23704=CARTESIAN_POINT('Ctrl Pts',(-7.07057502871922,-126.203019107145,
4.08219839617346));
#23705=CARTESIAN_POINT('Ctrl Pts',(-4.71371668580301,-126.028019107145,
8.16439679232994));
#23706=CARTESIAN_POINT('Ctrl Pts',(1.47018674401621E-11,-125.853019107145,
8.16439679232146));
#23707=CARTESIAN_POINT('Ctrl Pts',(4.71371668583241,-125.678019107145,8.16439679231297));
#23708=CARTESIAN_POINT('Ctrl Pts',(7.07057502873392,-125.503019107145,4.082198396148));
#23709=CARTESIAN_POINT('Ctrl Pts',(9.42743337163542,-125.328019107145,-1.69756769845304E-11));
#23710=CARTESIAN_POINT('Ctrl Pts',(7.07057502871922,-125.153019107145,-4.08219839617346));
#23711=CARTESIAN_POINT('Ctrl Pts',(4.71371668580301,-124.978019107145,-8.16439679232994));
#23712=CARTESIAN_POINT('Ctrl Pts',(-1.4702867290402E-11,-124.803019107145,
-8.16439679232146));
#23713=CARTESIAN_POINT('Ctrl Pts',(-4.71371668583241,-124.628019107145,
-8.16439679231297));
#23714=CARTESIAN_POINT('Ctrl Pts',(-7.07057502873392,-124.453019107145,
-4.082198396148));
#23715=CARTESIAN_POINT('Ctrl Pts',(-9.42743337163542,-124.278019107145,
1.69768315121407E-11));
#23716=CARTESIAN_POINT('Ctrl Pts',(-7.07057502871922,-124.103019107145,
4.08219839617346));
#23717=CARTESIAN_POINT('Ctrl Pts',(-4.71371668580301,-123.928019107145,
8.16439679232994));
#23718=CARTESIAN_POINT('Ctrl Pts',(1.47018674401621E-11,-123.753019107145,
8.16439679232146));
#23719=CARTESIAN_POINT('Ctrl Pts',(4.71371668583241,-123.578019107145,8.16439679231297));
#23720=CARTESIAN_POINT('Ctrl Pts',(7.07057502873392,-123.403019107145,4.082198396148));
#23721=CARTESIAN_POINT('Ctrl Pts',(9.42743337163542,-123.228019107145,-1.69756769845304E-11));
#23722=CARTESIAN_POINT('Ctrl Pts',(7.07057502871922,-123.053019107145,-4.08219839617346));
#23723=CARTESIAN_POINT('Ctrl Pts',(4.71371668580301,-122.878019107145,-8.16439679232994));
#23724=CARTESIAN_POINT('Ctrl Pts',(-1.4702867290402E-11,-122.703019107145,
-8.16439679232146));
#23725=CARTESIAN_POINT('Ctrl Pts',(-4.71371668583241,-122.528019107145,
-8.16439679231297));
#23726=CARTESIAN_POINT('Ctrl Pts',(-7.07057502873392,-122.353019107145,
-4.082198396148));
#23727=CARTESIAN_POINT('Ctrl Pts',(-9.42743337163542,-122.178019107145,
1.69768315121407E-11));
#23728=CARTESIAN_POINT('Ctrl Pts',(-7.07057502871922,-122.003019107145,
4.08219839617346));
#23729=CARTESIAN_POINT('Ctrl Pts',(-4.71371668580301,-121.828019107145,
8.16439679232994));
#23730=CARTESIAN_POINT('Ctrl Pts',(1.47018674401621E-11,-121.653019107145,
8.16439679232146));
#23731=CARTESIAN_POINT('Ctrl Pts',(4.71371668583241,-121.478019107145,8.16439679231297));
#23732=CARTESIAN_POINT('Ctrl Pts',(7.07057502873392,-121.303019107145,4.082198396148));
#23733=CARTESIAN_POINT('Ctrl Pts',(9.42743337163542,-121.128019107145,-1.69756769845304E-11));
#23734=CARTESIAN_POINT('Ctrl Pts',(7.07057502871922,-120.953019107145,-4.08219839617346));
#23735=CARTESIAN_POINT('Ctrl Pts',(4.71371668580301,-120.778019107145,-8.16439679232994));
#23736=CARTESIAN_POINT('Ctrl Pts',(-1.4702867290402E-11,-120.603019107145,
-8.16439679232146));
#23737=CARTESIAN_POINT('Ctrl Pts',(-4.71371668583241,-120.428019107145,
-8.16439679231297));
#23738=CARTESIAN_POINT('Ctrl Pts',(-7.07057502873392,-120.253019107145,
-4.082198396148));
#23739=CARTESIAN_POINT('Ctrl Pts',(-9.42743337163542,-120.078019107145,
1.69768315121407E-11));
#23740=CARTESIAN_POINT('Ctrl Pts',(-7.07057502871922,-119.903019107145,
4.08219839617346));
#23741=CARTESIAN_POINT('Ctrl Pts',(-4.71371668580301,-119.728019107145,
8.16439679232994));
#23742=CARTESIAN_POINT('Ctrl Pts',(1.47018674401621E-11,-119.553019107145,
8.16439679232146));
#23743=CARTESIAN_POINT('Ctrl Pts',(4.71371668583241,-119.378019107145,8.16439679231297));
#23744=CARTESIAN_POINT('Ctrl Pts',(7.07057502873392,-119.203019107145,4.082198396148));
#23745=CARTESIAN_POINT('Ctrl Pts',(9.42743337163542,-119.028019107145,-1.69756769845304E-11));
#23746=CARTESIAN_POINT('Ctrl Pts',(7.07057502871922,-118.853019107145,-4.08219839617346));
#23747=CARTESIAN_POINT('Ctrl Pts',(4.71371668580301,-118.678019107145,-8.16439679232994));
#23748=CARTESIAN_POINT('Ctrl Pts',(-1.4702867290402E-11,-118.503019107145,
-8.16439679232146));
#23749=CARTESIAN_POINT('Ctrl Pts',(-4.71371668583241,-118.328019107145,
-8.16439679231297));
#23750=CARTESIAN_POINT('Ctrl Pts',(-7.07057502873392,-118.153019107145,
-4.082198396148));
#23751=CARTESIAN_POINT('Ctrl Pts',(-9.42743337163542,-117.978019107145,
1.69768315121407E-11));
#23752=CARTESIAN_POINT('Ctrl Pts',(-7.07057502871922,-117.803019107145,
4.08219839617346));
#23753=CARTESIAN_POINT('Ctrl Pts',(-4.71371668580301,-117.628019107145,
8.16439679232994));
#23754=CARTESIAN_POINT('Ctrl Pts',(1.47018674401621E-11,-117.453019107145,
8.16439679232146));
#23755=CARTESIAN_POINT('Ctrl Pts',(4.71371668583241,-117.278019107145,8.16439679231297));
#23756=CARTESIAN_POINT('Ctrl Pts',(7.07057502873392,-117.103019107145,4.082198396148));
#23757=CARTESIAN_POINT('Ctrl Pts',(9.42743337163542,-116.928019107145,-1.69756769845304E-11));
#23758=CARTESIAN_POINT('Ctrl Pts',(7.07057502871922,-116.753019107145,-4.08219839617346));
#23759=CARTESIAN_POINT('Ctrl Pts',(4.71371668580301,-116.578019107145,-8.16439679232994));
#23760=CARTESIAN_POINT('Ctrl Pts',(-1.4702867290402E-11,-116.403019107145,
-8.16439679232146));
#23761=CARTESIAN_POINT('Ctrl Pts',(-4.71371668583241,-116.228019107145,
-8.16439679231297));
#23762=CARTESIAN_POINT('Ctrl Pts',(-7.07057502873392,-116.053019107145,
-4.082198396148));
#23763=CARTESIAN_POINT('Ctrl Pts',(-9.42743337163542,-115.878019107145,
1.69768315121407E-11));
#23764=CARTESIAN_POINT('Ctrl Pts',(-7.07057502871922,-115.703019107145,
4.08219839617346));
#23765=CARTESIAN_POINT('Ctrl Pts',(-4.71371668580301,-115.528019107145,
8.16439679232994));
#23766=CARTESIAN_POINT('Ctrl Pts',(1.47018674401621E-11,-115.353019107145,
8.16439679232146));
#23767=CARTESIAN_POINT('Ctrl Pts',(4.71371668583241,-115.178019107145,8.16439679231297));
#23768=CARTESIAN_POINT('Ctrl Pts',(7.07057502873392,-115.003019107145,4.082198396148));
#23769=CARTESIAN_POINT('Ctrl Pts',(9.42743337163542,-114.828019107145,-1.69756769845304E-11));
#23770=CARTESIAN_POINT('Ctrl Pts',(7.07057502871922,-114.653019107145,-4.08219839617346));
#23771=CARTESIAN_POINT('Ctrl Pts',(4.71371668580301,-114.478019107145,-8.16439679232994));
#23772=CARTESIAN_POINT('Ctrl Pts',(-1.4702867290402E-11,-114.303019107145,
-8.16439679232146));
#23773=CARTESIAN_POINT('Ctrl Pts',(-4.71371668583241,-114.128019107145,
-8.16439679231297));
#23774=CARTESIAN_POINT('Ctrl Pts',(-7.07057502873392,-113.953019107145,
-4.082198396148));
#23775=CARTESIAN_POINT('Ctrl Pts',(-9.42743337163542,-113.778019107145,
1.69768315121407E-11));
#23776=CARTESIAN_POINT('Ctrl Pts',(-7.07057502871922,-113.603019107145,
4.08219839617346));
#23777=CARTESIAN_POINT('Ctrl Pts',(-4.71371668580301,-113.428019107145,
8.16439679232994));
#23778=CARTESIAN_POINT('Ctrl Pts',(1.47018674401621E-11,-113.253019107145,
8.16439679232146));
#23779=CARTESIAN_POINT('Ctrl Pts',(4.71371668583241,-113.078019107145,8.16439679231297));
#23780=CARTESIAN_POINT('Ctrl Pts',(7.07057502873392,-112.903019107145,4.082198396148));
#23781=CARTESIAN_POINT('Ctrl Pts',(9.42743337163542,-112.728019107145,-1.69756769845304E-11));
#23782=CARTESIAN_POINT('Ctrl Pts',(7.07057502871922,-112.553019107145,-4.08219839617346));
#23783=CARTESIAN_POINT('Ctrl Pts',(4.71371668580301,-112.378019107145,-8.16439679232994));
#23784=CARTESIAN_POINT('Ctrl Pts',(-1.4702867290402E-11,-112.203019107145,
-8.16439679232146));
#23785=CARTESIAN_POINT('Ctrl Pts',(-4.71371668583241,-112.028019107145,
-8.16439679231297));
#23786=CARTESIAN_POINT('Ctrl Pts',(-7.07057502873392,-111.853019107145,
-4.082198396148));
#23787=CARTESIAN_POINT('Ctrl Pts',(-9.42743337163542,-111.678019107145,
1.69768315121407E-11));
#23788=CARTESIAN_POINT('Ctrl Pts',(-7.07057502871922,-111.503019107145,
4.08219839617346));
#23789=CARTESIAN_POINT('Ctrl Pts',(-4.71371668580301,-111.328019107145,
8.16439679232994));
#23790=CARTESIAN_POINT('Ctrl Pts',(1.47018674401621E-11,-111.153019107145,
8.16439679232146));
#23791=CARTESIAN_POINT('Ctrl Pts',(4.71371668583241,-110.978019107145,8.16439679231297));
#23792=CARTESIAN_POINT('Ctrl Pts',(7.07057502873392,-110.803019107145,4.082198396148));
#23793=CARTESIAN_POINT('Ctrl Pts',(9.42743337163542,-110.628019107145,-1.69756769845304E-11));
#23794=CARTESIAN_POINT('Ctrl Pts',(7.07057502871922,-110.453019107145,-4.08219839617346));
#23795=CARTESIAN_POINT('Ctrl Pts',(4.71371668580301,-110.278019107145,-8.16439679232994));
#23796=CARTESIAN_POINT('Ctrl Pts',(-1.4702867290402E-11,-110.103019107145,
-8.16439679232146));
#23797=CARTESIAN_POINT('Ctrl Pts',(-4.71371668583241,-109.928019107145,
-8.16439679231297));
#23798=CARTESIAN_POINT('Ctrl Pts',(-7.07057502873392,-109.753019107145,
-4.082198396148));
#23799=CARTESIAN_POINT('Ctrl Pts',(-9.42743337163542,-109.578019107145,
1.69768315121407E-11));
#23800=CARTESIAN_POINT('Ctrl Pts',(-7.07057502871922,-109.403019107145,
4.08219839617346));
#23801=CARTESIAN_POINT('Ctrl Pts',(-4.71371668580301,-109.228019107145,
8.16439679232994));
#23802=CARTESIAN_POINT('Ctrl Pts',(1.47018674401621E-11,-109.053019107145,
8.16439679232146));
#23803=CARTESIAN_POINT('Ctrl Pts',(4.71371668583241,-108.878019107145,8.16439679231297));
#23804=CARTESIAN_POINT('Ctrl Pts',(7.07057502873392,-108.703019107145,4.082198396148));
#23805=CARTESIAN_POINT('Ctrl Pts',(9.42743337163542,-108.528019107145,-1.69756769845304E-11));
#23806=CARTESIAN_POINT('Ctrl Pts',(7.07057502871922,-108.353019107145,-4.08219839617346));
#23807=CARTESIAN_POINT('Ctrl Pts',(4.71371668580301,-108.178019107145,-8.16439679232994));
#23808=CARTESIAN_POINT('Ctrl Pts',(-1.4702867290402E-11,-108.003019107145,
-8.16439679232146));
#23809=CARTESIAN_POINT('Ctrl Pts',(-4.71371668583241,-107.828019107145,
-8.16439679231297));
#23810=CARTESIAN_POINT('Ctrl Pts',(-7.07057502873392,-107.653019107145,
-4.082198396148));
#23811=CARTESIAN_POINT('Ctrl Pts',(-9.42743337163542,-107.478019107145,
1.69768315121407E-11));
#23812=CARTESIAN_POINT('Ctrl Pts',(-7.07057502871922,-107.303019107145,
4.08219839617346));
#23813=CARTESIAN_POINT('Ctrl Pts',(-4.71371668580301,-107.128019107145,
8.16439679232994));
#23814=CARTESIAN_POINT('Ctrl Pts',(1.47018674401621E-11,-106.953019107145,
8.16439679232146));
#23815=CARTESIAN_POINT('Ctrl Pts',(4.71371668583241,-106.778019107145,8.16439679231297));
#23816=CARTESIAN_POINT('Ctrl Pts',(7.07057502873392,-106.603019107145,4.082198396148));
#23817=CARTESIAN_POINT('Ctrl Pts',(9.42743337163542,-106.428019107145,-1.69756769845304E-11));
#23818=CARTESIAN_POINT('Ctrl Pts',(7.07057502871922,-106.253019107145,-4.08219839617346));
#23819=CARTESIAN_POINT('Ctrl Pts',(4.71371668580301,-106.078019107145,-8.16439679232994));
#23820=CARTESIAN_POINT('Ctrl Pts',(-1.4702867290402E-11,-105.903019107145,
-8.16439679232146));
#23821=CARTESIAN_POINT('Ctrl Pts',(-4.71371668583241,-105.728019107145,
-8.16439679231297));
#23822=CARTESIAN_POINT('Ctrl Pts',(-7.07057502873392,-105.553019107145,
-4.082198396148));
#23823=CARTESIAN_POINT('Ctrl Pts',(-9.42743337163542,-105.378019107145,
1.69768315121407E-11));
#23824=CARTESIAN_POINT('Ctrl Pts',(-7.07057502871922,-105.203019107145,
4.08219839617346));
#23825=CARTESIAN_POINT('Ctrl Pts',(-4.71371668580301,-105.028019107145,
8.16439679232994));
#23826=CARTESIAN_POINT('Ctrl Pts',(1.47018674401621E-11,-104.853019107145,
8.16439679232146));
#23827=CARTESIAN_POINT('Ctrl Pts',(4.71371668583241,-104.678019107145,8.16439679231297));
#23828=CARTESIAN_POINT('Ctrl Pts',(7.07057502873392,-104.503019107145,4.082198396148));
#23829=CARTESIAN_POINT('Ctrl Pts',(9.42743337163542,-104.328019107145,-1.69756769845304E-11));
#23830=CARTESIAN_POINT('Ctrl Pts',(7.07057502871922,-104.153019107145,-4.08219839617346));
#23831=CARTESIAN_POINT('Ctrl Pts',(4.71371668580301,-103.978019107145,-8.16439679232994));
#23832=CARTESIAN_POINT('Ctrl Pts',(-1.4702867290402E-11,-103.803019107145,
-8.16439679232146));
#23833=CARTESIAN_POINT('Ctrl Pts',(-4.71371668583241,-103.628019107145,
-8.16439679231297));
#23834=CARTESIAN_POINT('Ctrl Pts',(-7.07057502873392,-103.453019107145,
-4.082198396148));
#23835=CARTESIAN_POINT('Ctrl Pts',(-9.42743337163542,-103.278019107145,
1.69768315121407E-11));
#23836=CARTESIAN_POINT('Ctrl Pts',(-7.07057502871922,-103.103019107145,
4.08219839617346));
#23837=CARTESIAN_POINT('Ctrl Pts',(-4.71371668580301,-102.928019107145,
8.16439679232994));
#23838=CARTESIAN_POINT('Ctrl Pts',(1.47018674401621E-11,-102.753019107145,
8.16439679232146));
#23839=CARTESIAN_POINT('Ctrl Pts',(4.71371668583241,-102.578019107145,8.16439679231297));
#23840=CARTESIAN_POINT('Ctrl Pts',(7.07057502873392,-102.403019107145,4.082198396148));
#23841=CARTESIAN_POINT('Ctrl Pts',(9.42743337163542,-102.228019107145,-1.69756769845304E-11));
#23842=CARTESIAN_POINT('Ctrl Pts',(7.07057502871922,-102.053019107145,-4.08219839617346));
#23843=CARTESIAN_POINT('Ctrl Pts',(4.71371668580301,-101.878019107145,-8.16439679232994));
#23844=CARTESIAN_POINT('Ctrl Pts',(-1.4702867290402E-11,-101.703019107145,
-8.16439679232146));
#23845=CARTESIAN_POINT('Ctrl Pts',(-4.71371668583241,-101.528019107145,
-8.16439679231297));
#23846=CARTESIAN_POINT('Ctrl Pts',(-7.07057502873392,-101.353019107145,
-4.082198396148));
#23847=CARTESIAN_POINT('Ctrl Pts',(-9.42743337163542,-101.178019107145,
1.69768315121407E-11));
#23848=CARTESIAN_POINT('Ctrl Pts',(-7.07057502871922,-101.003019107145,
4.08219839617346));
#23849=CARTESIAN_POINT('Ctrl Pts',(-4.71371668580301,-100.828019107145,
8.16439679232994));
#23850=CARTESIAN_POINT('Ctrl Pts',(1.47018674401621E-11,-100.653019107145,
8.16439679232146));
#23851=CARTESIAN_POINT('Ctrl Pts',(4.71371668583241,-100.478019107145,8.16439679231297));
#23852=CARTESIAN_POINT('Ctrl Pts',(7.07057502873392,-100.303019107145,4.082198396148));
#23853=CARTESIAN_POINT('Ctrl Pts',(9.42743337163542,-100.128019107145,-1.69756769845304E-11));
#23854=CARTESIAN_POINT('Ctrl Pts',(7.07057502871922,-99.953019107145,-4.08219839617346));
#23855=CARTESIAN_POINT('Ctrl Pts',(4.71371668580301,-99.7780191071449,-8.16439679232994));
#23856=CARTESIAN_POINT('Ctrl Pts',(-1.4702867290402E-11,-99.6030191071449,
-8.16439679232146));
#23857=CARTESIAN_POINT('Ctrl Pts',(-4.71371668583241,-99.4280191071449,
-8.16439679231297));
#23858=CARTESIAN_POINT('Ctrl Pts',(-7.07057502873392,-99.253019107145,-4.082198396148));
#23859=CARTESIAN_POINT('Ctrl Pts',(-9.42743337163542,-99.078019107145,1.69768315121407E-11));
#23860=CARTESIAN_POINT('Ctrl Pts',(-7.07057502871922,-98.903019107145,4.08219839617346));
#23861=CARTESIAN_POINT('Ctrl Pts',(-4.71371668580301,-98.7280191071449,
8.16439679232994));
#23862=CARTESIAN_POINT('Ctrl Pts',(1.47018674401621E-11,-98.5530191071449,
8.16439679232146));
#23863=CARTESIAN_POINT('Ctrl Pts',(4.71371668583241,-98.378019107145,8.16439679231297));
#23864=CARTESIAN_POINT('Ctrl Pts',(7.07057502873392,-98.2030191071449,4.082198396148));
#23865=CARTESIAN_POINT('Ctrl Pts',(9.42743337163542,-98.0280191071449,-1.69756769845304E-11));
#23866=CARTESIAN_POINT('Ctrl Pts',(7.07057502871922,-97.8530191071449,-4.08219839617346));
#23867=CARTESIAN_POINT('Ctrl Pts',(4.71371668580301,-97.6780191071449,-8.16439679232994));
#23868=CARTESIAN_POINT('Ctrl Pts',(-1.4702867290402E-11,-97.503019107145,
-8.16439679232146));
#23869=CARTESIAN_POINT('Ctrl Pts',(-4.71371668583241,-97.328019107145,-8.16439679231297));
#23870=CARTESIAN_POINT('Ctrl Pts',(-7.07057502873392,-97.153019107145,-4.082198396148));
#23871=CARTESIAN_POINT('Ctrl Pts',(-9.42743337163542,-96.978019107145,1.69768315121407E-11));
#23872=CARTESIAN_POINT('Ctrl Pts',(-7.07057502871922,-96.803019107145,4.08219839617346));
#23873=CARTESIAN_POINT('Ctrl Pts',(-4.71371668580301,-96.6280191071449,
8.16439679232994));
#23874=CARTESIAN_POINT('Ctrl Pts',(1.47018674401621E-11,-96.453019107145,
8.16439679232146));
#23875=CARTESIAN_POINT('Ctrl Pts',(4.71371668583241,-96.278019107145,8.16439679231297));
#23876=CARTESIAN_POINT('Ctrl Pts',(7.07057502873392,-96.103019107145,4.082198396148));
#23877=CARTESIAN_POINT('Ctrl Pts',(9.42743337163542,-95.928019107145,-1.69756769845304E-11));
#23878=CARTESIAN_POINT('Ctrl Pts',(7.07057502871922,-95.753019107145,-4.08219839617346));
#23879=CARTESIAN_POINT('Ctrl Pts',(4.71371668580301,-95.5780191071449,-8.16439679232994));
#23880=CARTESIAN_POINT('Ctrl Pts',(-1.4702867290402E-11,-95.403019107145,
-8.16439679232146));
#23881=CARTESIAN_POINT('Ctrl Pts',(-4.71371668583241,-95.228019107145,-8.16439679231297));
#23882=CARTESIAN_POINT('Ctrl Pts',(-7.07057502873392,-95.053019107145,-4.082198396148));
#23883=CARTESIAN_POINT('Ctrl Pts',(-9.42743337163542,-94.8780191071449,
1.69768315121407E-11));
#23884=CARTESIAN_POINT('Ctrl Pts',(-7.07057502871922,-94.703019107145,4.08219839617346));
#23885=CARTESIAN_POINT('Ctrl Pts',(-4.71371668580301,-94.528019107145,8.16439679232994));
#23886=CARTESIAN_POINT('Ctrl Pts',(1.47018674401621E-11,-94.3530191071449,
8.16439679232146));
#23887=CARTESIAN_POINT('Ctrl Pts',(4.71371668583241,-94.178019107145,8.16439679231297));
#23888=CARTESIAN_POINT('Ctrl Pts',(7.07057502873392,-94.003019107145,4.082198396148));
#23889=CARTESIAN_POINT('Ctrl Pts',(9.42743337163542,-93.8280191071449,-1.69756769845304E-11));
#23890=CARTESIAN_POINT('Ctrl Pts',(7.07057502871922,-93.6530191071449,-4.08219839617346));
#23891=CARTESIAN_POINT('Ctrl Pts',(4.71371668580301,-93.4780191071449,-8.16439679232994));
#23892=CARTESIAN_POINT('Ctrl Pts',(-1.4702867290402E-11,-93.3030191071449,
-8.16439679232146));
#23893=CARTESIAN_POINT('Ctrl Pts',(-4.71371668583241,-93.128019107145,-8.16439679231297));
#23894=CARTESIAN_POINT('Ctrl Pts',(-7.07057502873392,-92.953019107145,-4.082198396148));
#23895=CARTESIAN_POINT('Ctrl Pts',(-9.42743337163542,-92.7780191071449,
1.69768315121407E-11));
#23896=CARTESIAN_POINT('Ctrl Pts',(-7.07057502871922,-92.6030191071449,
4.08219839617346));
#23897=CARTESIAN_POINT('Ctrl Pts',(-4.71371668580301,-92.428019107145,8.16439679232994));
#23898=CARTESIAN_POINT('Ctrl Pts',(1.47018674401621E-11,-92.253019107145,
8.16439679232146));
#23899=CARTESIAN_POINT('Ctrl Pts',(4.71371668583241,-92.0780191071449,8.16439679231297));
#23900=CARTESIAN_POINT('Ctrl Pts',(7.07057502873392,-91.903019107145,4.082198396148));
#23901=CARTESIAN_POINT('Ctrl Pts',(9.42743337163542,-91.728019107145,-1.69756769845304E-11));
#23902=CARTESIAN_POINT('Ctrl Pts',(7.07057502871922,-91.553019107145,-4.08219839617346));
#23903=CARTESIAN_POINT('Ctrl Pts',(4.71371668580301,-91.378019107145,-8.16439679232994));
#23904=CARTESIAN_POINT('Ctrl Pts',(-1.4702867290402E-11,-91.203019107145,
-8.16439679232146));
#23905=CARTESIAN_POINT('Ctrl Pts',(-4.71371668583241,-91.028019107145,-8.16439679231297));
#23906=CARTESIAN_POINT('Ctrl Pts',(-7.07057502873392,-90.853019107145,-4.082198396148));
#23907=CARTESIAN_POINT('Ctrl Pts',(-9.42743337163542,-90.678019107145,1.69768315121407E-11));
#23908=CARTESIAN_POINT('Ctrl Pts',(-7.07057502871922,-90.503019107145,4.08219839617346));
#23909=CARTESIAN_POINT('Ctrl Pts',(-4.71371668580301,-90.328019107145,8.16439679232994));
#23910=CARTESIAN_POINT('Ctrl Pts',(1.47018674401621E-11,-90.153019107145,
8.16439679232146));
#23911=CARTESIAN_POINT('Ctrl Pts',(4.71371668583241,-89.978019107145,8.16439679231297));
#23912=CARTESIAN_POINT('Ctrl Pts',(7.07057502873392,-89.803019107145,4.082198396148));
#23913=CARTESIAN_POINT('Ctrl Pts',(9.42743337163542,-89.628019107145,-1.69756769845304E-11));
#23914=CARTESIAN_POINT('Ctrl Pts',(7.07057502871922,-89.4530191071449,-4.08219839617346));
#23915=CARTESIAN_POINT('Ctrl Pts',(4.71371668580301,-89.278019107145,-8.16439679232994));
#23916=CARTESIAN_POINT('Ctrl Pts',(-1.4702867290402E-11,-89.103019107145,
-8.16439679232146));
#23917=CARTESIAN_POINT('Ctrl Pts',(-4.71371668583241,-88.9280191071449,
-8.16439679231297));
#23918=CARTESIAN_POINT('Ctrl Pts',(-7.07057502873392,-88.753019107145,-4.082198396148));
#23919=CARTESIAN_POINT('Ctrl Pts',(-9.42743337163542,-88.578019107145,1.69768315121407E-11));
#23920=CARTESIAN_POINT('Ctrl Pts',(-7.07057502871922,-88.403019107145,4.08219839617346));
#23921=CARTESIAN_POINT('Ctrl Pts',(-4.71371668580301,-88.228019107145,8.16439679232994));
#23922=CARTESIAN_POINT('Ctrl Pts',(1.47018674401621E-11,-88.053019107145,
8.16439679232146));
#23923=CARTESIAN_POINT('Ctrl Pts',(4.71371668583241,-87.878019107145,8.16439679231297));
#23924=CARTESIAN_POINT('Ctrl Pts',(7.07057502873392,-87.703019107145,4.082198396148));
#23925=CARTESIAN_POINT('Ctrl Pts',(9.42743337163542,-87.528019107145,-1.69756769845304E-11));
#23926=CARTESIAN_POINT('Ctrl Pts',(7.07057502871922,-87.353019107145,-4.08219839617346));
#23927=CARTESIAN_POINT('Ctrl Pts',(4.71371668580301,-87.178019107145,-8.16439679232994));
#23928=CARTESIAN_POINT('Ctrl Pts',(-1.4702867290402E-11,-87.003019107145,
-8.16439679232146));
#23929=CARTESIAN_POINT('Ctrl Pts',(-4.71371668583241,-86.828019107145,-8.16439679231297));
#23930=CARTESIAN_POINT('Ctrl Pts',(-7.07057502873392,-86.653019107145,-4.082198396148));
#23931=CARTESIAN_POINT('Ctrl Pts',(-9.42743337163542,-86.478019107145,1.69768315121407E-11));
#23932=CARTESIAN_POINT('Ctrl Pts',(-7.07057502871922,-86.303019107145,4.08219839617346));
#23933=CARTESIAN_POINT('Ctrl Pts',(-4.71371668580301,-86.128019107145,8.16439679232994));
#23934=CARTESIAN_POINT('Ctrl Pts',(1.47018674401621E-11,-85.953019107145,
8.16439679232146));
#23935=CARTESIAN_POINT('Ctrl Pts',(4.71371668583241,-85.778019107145,8.16439679231297));
#23936=CARTESIAN_POINT('Ctrl Pts',(7.07057502873392,-85.603019107145,4.082198396148));
#23937=CARTESIAN_POINT('Ctrl Pts',(9.42743337163542,-85.428019107145,-1.69756769845304E-11));
#23938=CARTESIAN_POINT('Ctrl Pts',(7.07057502871922,-85.253019107145,-4.08219839617346));
#23939=CARTESIAN_POINT('Ctrl Pts',(4.71371668580301,-85.078019107145,-8.16439679232994));
#23940=CARTESIAN_POINT('Ctrl Pts',(-1.4702867290402E-11,-84.903019107145,
-8.16439679232146));
#23941=CARTESIAN_POINT('Ctrl Pts',(-4.71371668583241,-84.728019107145,-8.16439679231297));
#23942=CARTESIAN_POINT('Ctrl Pts',(-7.07057502873392,-84.553019107145,-4.082198396148));
#23943=CARTESIAN_POINT('Ctrl Pts',(-9.42743337163542,-84.378019107145,1.69768315121407E-11));
#23944=CARTESIAN_POINT('Ctrl Pts',(-7.07057502871922,-84.203019107145,4.08219839617346));
#23945=CARTESIAN_POINT('Ctrl Pts',(-4.71371668580301,-84.028019107145,8.16439679232994));
#23946=CARTESIAN_POINT('Ctrl Pts',(1.47018674401621E-11,-83.853019107145,
8.16439679232146));
#23947=CARTESIAN_POINT('Ctrl Pts',(4.71371668583241,-83.678019107145,8.16439679231297));
#23948=CARTESIAN_POINT('Ctrl Pts',(7.07057502873392,-83.503019107145,4.082198396148));
#23949=CARTESIAN_POINT('Ctrl Pts',(9.42743337163542,-83.328019107145,-1.69756769845304E-11));
#23950=CARTESIAN_POINT('Ctrl Pts',(7.07057502871922,-83.153019107145,-4.08219839617346));
#23951=CARTESIAN_POINT('Ctrl Pts',(4.71371668580301,-82.978019107145,-8.16439679232994));
#23952=CARTESIAN_POINT('Ctrl Pts',(-1.4702867290402E-11,-82.803019107145,
-8.16439679232146));
#23953=CARTESIAN_POINT('Ctrl Pts',(-4.71371668583241,-82.628019107145,-8.16439679231297));
#23954=CARTESIAN_POINT('Ctrl Pts',(-7.07057502873392,-82.453019107145,-4.082198396148));
#23955=CARTESIAN_POINT('Ctrl Pts',(-9.42743337163542,-82.278019107145,1.69768315121407E-11));
#23956=CARTESIAN_POINT('Ctrl Pts',(-7.07057502871922,-82.103019107145,4.08219839617346));
#23957=CARTESIAN_POINT('Ctrl Pts',(-4.71371668580301,-81.928019107145,8.16439679232994));
#23958=CARTESIAN_POINT('Ctrl Pts',(1.47018674401621E-11,-81.753019107145,
8.16439679232146));
#23959=CARTESIAN_POINT('Ctrl Pts',(4.71371668583241,-81.578019107145,8.16439679231297));
#23960=CARTESIAN_POINT('Ctrl Pts',(7.07057502873392,-81.403019107145,4.082198396148));
#23961=CARTESIAN_POINT('Ctrl Pts',(9.42743337163542,-81.228019107145,-1.69756769845304E-11));
#23962=CARTESIAN_POINT('Ctrl Pts',(7.07057502871922,-81.053019107145,-4.08219839617346));
#23963=CARTESIAN_POINT('Ctrl Pts',(4.71371668580301,-80.878019107145,-8.16439679232994));
#23964=CARTESIAN_POINT('Ctrl Pts',(-1.4702867290402E-11,-80.703019107145,
-8.16439679232146));
#23965=CARTESIAN_POINT('Ctrl Pts',(-4.71371668583241,-80.528019107145,-8.16439679231297));
#23966=CARTESIAN_POINT('Ctrl Pts',(-7.07057502873392,-80.353019107145,-4.082198396148));
#23967=CARTESIAN_POINT('Ctrl Pts',(-9.42743337163542,-80.178019107145,1.69768315121407E-11));
#23968=CARTESIAN_POINT('Ctrl Pts',(-7.07057502871922,-80.003019107145,4.08219839617346));
#23969=CARTESIAN_POINT('Ctrl Pts',(-4.71371668580301,-79.828019107145,8.16439679232994));
#23970=CARTESIAN_POINT('Ctrl Pts',(1.47018674401621E-11,-79.653019107145,
8.16439679232146));
#23971=CARTESIAN_POINT('Ctrl Pts',(4.71371668583241,-79.478019107145,8.16439679231297));
#23972=CARTESIAN_POINT('Ctrl Pts',(7.07057502873392,-79.303019107145,4.082198396148));
#23973=CARTESIAN_POINT('Ctrl Pts',(9.42743337163542,-79.128019107145,-1.69756769845304E-11));
#23974=CARTESIAN_POINT('Ctrl Pts',(7.07057502871922,-78.953019107145,-4.08219839617346));
#23975=CARTESIAN_POINT('Ctrl Pts',(4.71371668580301,-78.778019107145,-8.16439679232994));
#23976=CARTESIAN_POINT('Ctrl Pts',(-1.4702867290402E-11,-78.603019107145,
-8.16439679232146));
#23977=CARTESIAN_POINT('Ctrl Pts',(-4.71371668583241,-78.428019107145,-8.16439679231297));
#23978=CARTESIAN_POINT('Ctrl Pts',(-7.07057502873392,-78.253019107145,-4.082198396148));
#23979=CARTESIAN_POINT('Ctrl Pts',(-9.42743337163542,-78.078019107145,1.69768315121407E-11));
#23980=CARTESIAN_POINT('Ctrl Pts',(-7.07057502871922,-77.903019107145,4.08219839617346));
#23981=CARTESIAN_POINT('Ctrl Pts',(-4.71371668580301,-77.728019107145,8.16439679232994));
#23982=CARTESIAN_POINT('Ctrl Pts',(1.47018674401621E-11,-77.553019107145,
8.16439679232146));
#23983=CARTESIAN_POINT('Ctrl Pts',(4.71371668583241,-77.378019107145,8.16439679231297));
#23984=CARTESIAN_POINT('Ctrl Pts',(7.07057502873392,-77.203019107145,4.082198396148));
#23985=CARTESIAN_POINT('Ctrl Pts',(9.42743337163542,-77.028019107145,-1.69756769845304E-11));
#23986=CARTESIAN_POINT('Ctrl Pts',(7.07057502871922,-76.853019107145,-4.08219839617346));
#23987=CARTESIAN_POINT('Ctrl Pts',(4.71371668580301,-76.678019107145,-8.16439679232994));
#23988=CARTESIAN_POINT('Ctrl Pts',(-1.4702867290402E-11,-76.503019107145,
-8.16439679232146));
#23989=CARTESIAN_POINT('Ctrl Pts',(-4.71371668583241,-76.328019107145,-8.16439679231297));
#23990=CARTESIAN_POINT('Ctrl Pts',(-7.07057502873392,-76.153019107145,-4.082198396148));
#23991=CARTESIAN_POINT('Ctrl Pts',(-9.42743337163542,-75.978019107145,1.69768315121407E-11));
#23992=CARTESIAN_POINT('Ctrl Pts',(-7.07057502871922,-75.803019107145,4.08219839617346));
#23993=CARTESIAN_POINT('Ctrl Pts',(-4.71371668580301,-75.628019107145,8.16439679232994));
#23994=CARTESIAN_POINT('Ctrl Pts',(1.47018674401621E-11,-75.453019107145,
8.16439679232146));
#23995=CARTESIAN_POINT('Ctrl Pts',(4.71371668583241,-75.278019107145,8.16439679231297));
#23996=CARTESIAN_POINT('Ctrl Pts',(7.07057502873392,-75.103019107145,4.082198396148));
#23997=CARTESIAN_POINT('Ctrl Pts',(9.42743337163542,-74.928019107145,-1.69756769845304E-11));
#23998=CARTESIAN_POINT('Ctrl Pts',(7.07057502871922,-74.753019107145,-4.08219839617346));
#23999=CARTESIAN_POINT('Ctrl Pts',(4.71371668580301,-74.578019107145,-8.16439679232994));
#24000=CARTESIAN_POINT('Ctrl Pts',(-1.4702867290402E-11,-74.403019107145,
-8.16439679232146));
#24001=CARTESIAN_POINT('Ctrl Pts',(-4.71371668583241,-74.228019107145,-8.16439679231297));
#24002=CARTESIAN_POINT('Ctrl Pts',(-7.07057502873392,-74.053019107145,-4.082198396148));
#24003=CARTESIAN_POINT('Ctrl Pts',(-9.42743337163542,-73.878019107145,1.69768315121407E-11));
#24004=CARTESIAN_POINT('Ctrl Pts',(-7.07057502871922,-73.703019107145,4.08219839617346));
#24005=CARTESIAN_POINT('Ctrl Pts',(-4.71371668580301,-73.528019107145,8.16439679232994));
#24006=CARTESIAN_POINT('Ctrl Pts',(1.47018674401621E-11,-73.353019107145,
8.16439679232146));
#24007=CARTESIAN_POINT('Ctrl Pts',(4.71371668583241,-73.178019107145,8.16439679231297));
#24008=CARTESIAN_POINT('Ctrl Pts',(7.07057502873392,-73.003019107145,4.082198396148));
#24009=CARTESIAN_POINT('Ctrl Pts',(9.42743337163542,-72.828019107145,-1.69756769845304E-11));
#24010=CARTESIAN_POINT('Ctrl Pts',(7.07057502871922,-72.653019107145,-4.08219839617346));
#24011=CARTESIAN_POINT('Ctrl Pts',(4.71371668580301,-72.478019107145,-8.16439679232994));
#24012=CARTESIAN_POINT('Ctrl Pts',(-1.4702867290402E-11,-72.303019107145,
-8.16439679232146));
#24013=CARTESIAN_POINT('Ctrl Pts',(-4.71371668583241,-72.128019107145,-8.16439679231297));
#24014=CARTESIAN_POINT('Ctrl Pts',(-7.07057502873392,-71.953019107145,-4.082198396148));
#24015=CARTESIAN_POINT('Ctrl Pts',(-9.42743337163542,-71.778019107145,1.69768315121407E-11));
#24016=CARTESIAN_POINT('Ctrl Pts',(-7.07057502871922,-71.603019107145,4.08219839617346));
#24017=CARTESIAN_POINT('Ctrl Pts',(-4.71371668580301,-71.428019107145,8.16439679232994));
#24018=CARTESIAN_POINT('Ctrl Pts',(1.47018674401621E-11,-71.253019107145,
8.16439679232146));
#24019=CARTESIAN_POINT('Ctrl Pts',(4.71371668583241,-71.078019107145,8.16439679231297));
#24020=CARTESIAN_POINT('Ctrl Pts',(7.07057502873392,-70.903019107145,4.082198396148));
#24021=CARTESIAN_POINT('Ctrl Pts',(9.42743337163542,-70.728019107145,-1.69756769845304E-11));
#24022=CARTESIAN_POINT('Ctrl Pts',(7.07057502871922,-70.553019107145,-4.08219839617346));
#24023=CARTESIAN_POINT('Ctrl Pts',(4.71371668580301,-70.378019107145,-8.16439679232994));
#24024=CARTESIAN_POINT('Ctrl Pts',(-1.4702867290402E-11,-70.203019107145,
-8.16439679232146));
#24025=CARTESIAN_POINT('Ctrl Pts',(-4.71371668583241,-70.028019107145,-8.16439679231297));
#24026=CARTESIAN_POINT('Ctrl Pts',(-7.07057502873392,-69.853019107145,-4.082198396148));
#24027=CARTESIAN_POINT('Ctrl Pts',(-9.42743337163542,-69.678019107145,1.69768315121407E-11));
#24028=CARTESIAN_POINT('Ctrl Pts',(-7.07057502871922,-69.503019107145,4.08219839617346));
#24029=CARTESIAN_POINT('Ctrl Pts',(-4.71371668580301,-69.328019107145,8.16439679232994));
#24030=CARTESIAN_POINT('Ctrl Pts',(1.47018674401621E-11,-69.153019107145,
8.16439679232146));
#24031=CARTESIAN_POINT('Ctrl Pts',(4.71371668583241,-68.978019107145,8.16439679231297));
#24032=CARTESIAN_POINT('Ctrl Pts',(7.07057502873392,-68.803019107145,4.082198396148));
#24033=CARTESIAN_POINT('Ctrl Pts',(9.42743337163542,-68.6280191071451,-1.69756769845304E-11));
#24034=CARTESIAN_POINT('Ctrl Pts',(7.07057502871922,-68.453019107145,-4.08219839617346));
#24035=CARTESIAN_POINT('Ctrl Pts',(4.71371668580301,-68.278019107145,-8.16439679232994));
#24036=CARTESIAN_POINT('Ctrl Pts',(-1.4702867290402E-11,-68.103019107145,
-8.16439679232146));
#24037=CARTESIAN_POINT('Ctrl Pts',(-4.71371668583241,-67.928019107145,-8.16439679231297));
#24038=CARTESIAN_POINT('Ctrl Pts',(-7.07057502873392,-67.753019107145,-4.082198396148));
#24039=CARTESIAN_POINT('Ctrl Pts',(-9.42743337163542,-67.5780191071451,
1.69768315121407E-11));
#24040=CARTESIAN_POINT('Ctrl Pts',(-7.07057502871922,-67.403019107145,4.08219839617346));
#24041=CARTESIAN_POINT('Ctrl Pts',(-4.71371668580301,-67.228019107145,8.16439679232994));
#24042=CARTESIAN_POINT('Ctrl Pts',(1.47018674401621E-11,-67.053019107145,
8.16439679232146));
#24043=CARTESIAN_POINT('Ctrl Pts',(4.71371668583241,-66.878019107145,8.16439679231297));
#24044=CARTESIAN_POINT('Ctrl Pts',(7.07057502873392,-66.703019107145,4.082198396148));
#24045=CARTESIAN_POINT('Ctrl Pts',(9.42743337163542,-66.5280191071451,-1.69756769845304E-11));
#24046=CARTESIAN_POINT('Ctrl Pts',(7.07057502871922,-66.353019107145,-4.08219839617346));
#24047=CARTESIAN_POINT('Ctrl Pts',(4.71371668580301,-66.178019107145,-8.16439679232994));
#24048=CARTESIAN_POINT('Ctrl Pts',(-1.4702867290402E-11,-66.003019107145,
-8.16439679232146));
#24049=CARTESIAN_POINT('Ctrl Pts',(-4.71371668583241,-65.828019107145,-8.16439679231297));
#24050=CARTESIAN_POINT('Ctrl Pts',(-7.07057502873392,-65.653019107145,-4.082198396148));
#24051=CARTESIAN_POINT('Ctrl Pts',(-9.42743337163542,-65.478019107145,1.69768315121407E-11));
#24052=CARTESIAN_POINT('Ctrl Pts',(-7.07057502871922,-65.303019107145,4.08219839617346));
#24053=CARTESIAN_POINT('Ctrl Pts',(-4.71371668580301,-65.1280191071451,
8.16439679232994));
#24054=CARTESIAN_POINT('Ctrl Pts',(1.47018674401621E-11,-64.953019107145,
8.16439679232146));
#24055=CARTESIAN_POINT('Ctrl Pts',(4.71371668583241,-64.778019107145,8.16439679231297));
#24056=CARTESIAN_POINT('Ctrl Pts',(7.07057502873392,-64.603019107145,4.082198396148));
#24057=CARTESIAN_POINT('Ctrl Pts',(9.42743337163542,-64.428019107145,-1.69756769845304E-11));
#24058=CARTESIAN_POINT('Ctrl Pts',(7.07057502871922,-64.253019107145,-4.08219839617346));
#24059=CARTESIAN_POINT('Ctrl Pts',(4.71371668580301,-64.0780191071451,-8.16439679232994));
#24060=CARTESIAN_POINT('Ctrl Pts',(-1.4702867290402E-11,-63.903019107145,
-8.16439679232146));
#24061=CARTESIAN_POINT('Ctrl Pts',(-4.71371668583241,-63.728019107145,-8.16439679231297));
#24062=CARTESIAN_POINT('Ctrl Pts',(-7.07057502873392,-63.553019107145,-4.082198396148));
#24063=CARTESIAN_POINT('Ctrl Pts',(-9.42743337163542,-63.378019107145,1.69768315121407E-11));
#24064=CARTESIAN_POINT('Ctrl Pts',(-7.07057502871922,-63.203019107145,4.08219839617346));
#24065=CARTESIAN_POINT('Ctrl Pts',(-4.71371668580301,-63.028019107145,8.16439679232994));
#24066=CARTESIAN_POINT('Ctrl Pts',(1.47018674401621E-11,-62.853019107145,
8.16439679232146));
#24067=CARTESIAN_POINT('Ctrl Pts',(4.71371668583241,-62.678019107145,8.16439679231297));
#24068=CARTESIAN_POINT('Ctrl Pts',(7.07057502873392,-62.503019107145,4.082198396148));
#24069=CARTESIAN_POINT('Ctrl Pts',(9.42743337163542,-62.328019107145,-1.69756769845304E-11));
#24070=CARTESIAN_POINT('Ctrl Pts',(7.07057502871922,-62.153019107145,-4.08219839617346));
#24071=CARTESIAN_POINT('Ctrl Pts',(4.71371668580301,-61.978019107145,-8.16439679232994));
#24072=CARTESIAN_POINT('Ctrl Pts',(-1.4702867290402E-11,-61.803019107145,
-8.16439679232146));
#24073=CARTESIAN_POINT('Ctrl Pts',(-4.71371668583241,-61.628019107145,-8.16439679231297));
#24074=CARTESIAN_POINT('Ctrl Pts',(-7.07057502873392,-61.453019107145,-4.082198396148));
#24075=CARTESIAN_POINT('Ctrl Pts',(-9.42743337163542,-61.278019107145,1.69768315121407E-11));
#24076=CARTESIAN_POINT('Ctrl Pts',(-7.07057502871922,-61.103019107145,4.08219839617346));
#24077=CARTESIAN_POINT('Ctrl Pts',(-4.71371668580301,-60.9280191071451,
8.16439679232994));
#24078=CARTESIAN_POINT('Ctrl Pts',(1.47018674401621E-11,-60.753019107145,
8.16439679232146));
#24079=CARTESIAN_POINT('Ctrl Pts',(4.71371668583241,-60.578019107145,8.16439679231297));
#24080=CARTESIAN_POINT('Ctrl Pts',(7.07057502873392,-60.403019107145,4.082198396148));
#24081=CARTESIAN_POINT('Ctrl Pts',(9.42743337163542,-60.228019107145,-1.69756769845304E-11));
#24082=CARTESIAN_POINT('Ctrl Pts',(7.07057502871922,-60.053019107145,-4.08219839617346));
#24083=CARTESIAN_POINT('Ctrl Pts',(4.71371668580301,-59.8780191071451,-8.16439679232994));
#24084=CARTESIAN_POINT('Ctrl Pts',(-1.4702867290402E-11,-59.703019107145,
-8.16439679232146));
#24085=CARTESIAN_POINT('Ctrl Pts',(-4.71371668583241,-59.528019107145,-8.16439679231297));
#24086=CARTESIAN_POINT('Ctrl Pts',(-7.07057502873392,-59.3530191071451,
-4.082198396148));
#24087=CARTESIAN_POINT('Ctrl Pts',(-9.42743337163542,-59.178019107145,1.69768315121407E-11));
#24088=CARTESIAN_POINT('Ctrl Pts',(-7.07057502871922,-59.003019107145,4.08219839617346));
#24089=CARTESIAN_POINT('Ctrl Pts',(-4.71371668580301,-58.8280191071451,
8.16439679232994));
#24090=CARTESIAN_POINT('Ctrl Pts',(1.47018674401621E-11,-58.653019107145,
8.16439679232146));
#24091=CARTESIAN_POINT('Ctrl Pts',(4.71371668583241,-58.478019107145,8.16439679231297));
#24092=CARTESIAN_POINT('Ctrl Pts',(7.07057502873392,-58.303019107145,4.082198396148));
#24093=CARTESIAN_POINT('Ctrl Pts',(9.42743337163542,-58.128019107145,-1.69756769845304E-11));
#24094=CARTESIAN_POINT('Ctrl Pts',(7.07057502871922,-57.953019107145,-4.08219839617346));
#24095=CARTESIAN_POINT('Ctrl Pts',(4.71371668580301,-57.7780191071451,-8.16439679232994));
#24096=CARTESIAN_POINT('Ctrl Pts',(-1.4702867290402E-11,-57.603019107145,
-8.16439679232146));
#24097=CARTESIAN_POINT('Ctrl Pts',(-4.71371668583241,-57.428019107145,-8.16439679231297));
#24098=CARTESIAN_POINT('Ctrl Pts',(-7.07057502873392,-57.253019107145,-4.082198396148));
#24099=CARTESIAN_POINT('Ctrl Pts',(-9.42743337163542,-57.078019107145,1.69768315121407E-11));
#24100=CARTESIAN_POINT('Ctrl Pts',(-7.07057502871922,-56.903019107145,4.08219839617346));
#24101=CARTESIAN_POINT('Ctrl Pts',(-4.71371668580301,-56.728019107145,8.16439679232994));
#24102=CARTESIAN_POINT('Ctrl Pts',(1.47018674401621E-11,-56.553019107145,
8.16439679232146));
#24103=CARTESIAN_POINT('Ctrl Pts',(4.71371668583241,-56.3780191071451,8.16439679231297));
#24104=CARTESIAN_POINT('Ctrl Pts',(7.07057502873392,-56.203019107145,4.082198396148));
#24105=CARTESIAN_POINT('Ctrl Pts',(9.42743337163542,-56.028019107145,-1.69756769845304E-11));
#24106=CARTESIAN_POINT('Ctrl Pts',(7.07057502871922,-55.8530191071451,-4.08219839617346));
#24107=CARTESIAN_POINT('Ctrl Pts',(4.71371668580301,-55.678019107145,-8.16439679232994));
#24108=CARTESIAN_POINT('Ctrl Pts',(-1.4702867290402E-11,-55.503019107145,
-8.16439679232146));
#24109=CARTESIAN_POINT('Ctrl Pts',(-4.71371668583241,-55.3280191071451,
-8.16439679231297));
#24110=CARTESIAN_POINT('Ctrl Pts',(-7.07057502873392,-55.153019107145,-4.082198396148));
#24111=CARTESIAN_POINT('Ctrl Pts',(-9.42743337163542,-54.9780191071451,
1.69768315121407E-11));
#24112=CARTESIAN_POINT('Ctrl Pts',(-7.07057502871922,-54.8030191071451,
4.08219839617346));
#24113=CARTESIAN_POINT('Ctrl Pts',(-4.71371668580301,-54.628019107145,8.16439679232994));
#24114=CARTESIAN_POINT('Ctrl Pts',(1.47018674401621E-11,-54.453019107145,
8.16439679232146));
#24115=CARTESIAN_POINT('Ctrl Pts',(4.71371668583241,-54.278019107145,8.16439679231297));
#24116=CARTESIAN_POINT('Ctrl Pts',(7.07057502873392,-54.1030191071451,4.082198396148));
#24117=CARTESIAN_POINT('Ctrl Pts',(9.42743337163542,-53.9280191071451,-1.69756769845304E-11));
#24118=CARTESIAN_POINT('Ctrl Pts',(7.07057502871922,-53.7530191071451,-4.08219839617346));
#24119=CARTESIAN_POINT('Ctrl Pts',(4.71371668580301,-53.5780191071451,-8.16439679232994));
#24120=CARTESIAN_POINT('Ctrl Pts',(-1.4702867290402E-11,-53.403019107145,
-8.16439679232146));
#24121=CARTESIAN_POINT('Ctrl Pts',(-4.71371668583241,-53.228019107145,-8.16439679231297));
#24122=CARTESIAN_POINT('Ctrl Pts',(-7.07057502873392,-53.0530191071451,
-4.082198396148));
#24123=CARTESIAN_POINT('Ctrl Pts',(-9.42743337163542,-52.878019107145,1.69768315121407E-11));
#24124=CARTESIAN_POINT('Ctrl Pts',(-7.07057502871922,-52.703019107145,4.08219839617346));
#24125=CARTESIAN_POINT('Ctrl Pts',(-4.71371668580301,-52.528019107145,8.16439679232994));
#24126=CARTESIAN_POINT('Ctrl Pts',(1.47018674401621E-11,-52.3530191071451,
8.16439679232146));
#24127=CARTESIAN_POINT('Ctrl Pts',(4.71371668583241,-52.178019107145,8.16439679231297));
#24128=CARTESIAN_POINT('Ctrl Pts',(7.07057502873392,-52.0030191071451,4.082198396148));
#24129=CARTESIAN_POINT('Ctrl Pts',(9.42743337163542,-51.828019107145,-1.69756769845304E-11));
#24130=CARTESIAN_POINT('Ctrl Pts',(7.07057502871922,-51.6530191071451,-4.08219839617346));
#24131=CARTESIAN_POINT('Ctrl Pts',(4.71371668580301,-51.4780191071451,-8.16439679232994));
#24132=CARTESIAN_POINT('Ctrl Pts',(-1.4702867290402E-11,-51.303019107145,
-8.16439679232146));
#24133=CARTESIAN_POINT('Ctrl Pts',(-4.71371668583241,-51.1280191071451,
-8.16439679231297));
#24134=CARTESIAN_POINT('Ctrl Pts',(-7.07057502873392,-50.9530191071451,
-4.082198396148));
#24135=CARTESIAN_POINT('Ctrl Pts',(-9.42743337163542,-50.778019107145,1.69768315121407E-11));
#24136=CARTESIAN_POINT('Ctrl Pts',(-7.07057502871922,-50.6030191071451,
4.08219839617346));
#24137=CARTESIAN_POINT('Ctrl Pts',(-4.71371668580301,-50.4280191071451,
8.16439679232994));
#24138=CARTESIAN_POINT('Ctrl Pts',(1.47018674401621E-11,-50.253019107145,
8.16439679232146));
#24139=CARTESIAN_POINT('Ctrl Pts',(4.71371668583241,-50.0780191071451,8.16439679231297));
#24140=CARTESIAN_POINT('Ctrl Pts',(7.07057502873392,-49.9030191071451,4.082198396148));
#24141=CARTESIAN_POINT('Ctrl Pts',(9.42743337163542,-49.728019107145,-1.69756769845304E-11));
#24142=CARTESIAN_POINT('Ctrl Pts',(7.07057502871922,-49.5530191071451,-4.08219839617346));
#24143=CARTESIAN_POINT('Ctrl Pts',(4.71371668580301,-49.3780191071451,-8.16439679232994));
#24144=CARTESIAN_POINT('Ctrl Pts',(-1.4702867290402E-11,-49.2030191071451,
-8.16439679232146));
#24145=CARTESIAN_POINT('Ctrl Pts',(-4.71371668583241,-49.028019107145,-8.16439679231297));
#24146=CARTESIAN_POINT('Ctrl Pts',(-7.07057502873392,-48.853019107145,-4.082198396148));
#24147=CARTESIAN_POINT('Ctrl Pts',(-9.42743337163542,-48.6780191071451,
1.69768315121407E-11));
#24148=CARTESIAN_POINT('Ctrl Pts',(-7.07057502871922,-48.5030191071451,
4.08219839617346));
#24149=CARTESIAN_POINT('Ctrl Pts',(-4.71371668580301,-48.3280191071451,
8.16439679232994));
#24150=CARTESIAN_POINT('Ctrl Pts',(1.47018674401621E-11,-48.1530191071451,
8.16439679232146));
#24151=CARTESIAN_POINT('Ctrl Pts',(4.71371668583241,-47.9780191071451,8.16439679231297));
#24152=CARTESIAN_POINT('Ctrl Pts',(7.07057502873392,-47.8030191071451,4.082198396148));
#24153=CARTESIAN_POINT('Ctrl Pts',(9.42743337163542,-47.6280191071451,-1.69756769845304E-11));
#24154=CARTESIAN_POINT('Ctrl Pts',(7.07057502871922,-47.4530191071451,-4.08219839617346));
#24155=CARTESIAN_POINT('Ctrl Pts',(4.71371668580301,-47.2780191071451,-8.16439679232994));
#24156=CARTESIAN_POINT('Ctrl Pts',(-1.4702867290402E-11,-47.1030191071451,
-8.16439679232146));
#24157=CARTESIAN_POINT('Ctrl Pts',(-4.71371668583241,-46.9280191071451,
-8.16439679231297));
#24158=CARTESIAN_POINT('Ctrl Pts',(-7.07057502873392,-46.7530191071451,
-4.082198396148));
#24159=CARTESIAN_POINT('Ctrl Pts',(-9.42743337163542,-46.5780191071451,
1.69768315121407E-11));
#24160=CARTESIAN_POINT('Ctrl Pts',(-7.07057502871922,-46.4030191071451,
4.08219839617346));
#24161=CARTESIAN_POINT('Ctrl Pts',(-4.71371668580301,-46.2280191071451,
8.16439679232994));
#24162=CARTESIAN_POINT('Ctrl Pts',(1.47018674401621E-11,-46.0530191071451,
8.16439679232146));
#24163=CARTESIAN_POINT('Ctrl Pts',(4.71371668583241,-45.8780191071451,8.16439679231297));
#24164=CARTESIAN_POINT('Ctrl Pts',(7.07057502873392,-45.7030191071451,4.082198396148));
#24165=CARTESIAN_POINT('Ctrl Pts',(9.42743337163542,-45.5280191071451,-1.69756769845304E-11));
#24166=CARTESIAN_POINT('Ctrl Pts',(7.07057502871922,-45.3530191071451,-4.08219839617346));
#24167=CARTESIAN_POINT('Ctrl Pts',(4.71371668580301,-45.1780191071451,-8.16439679232994));
#24168=CARTESIAN_POINT('Ctrl Pts',(-1.4702867290402E-11,-45.0030191071451,
-8.16439679232146));
#24169=CARTESIAN_POINT('Ctrl Pts',(-4.71371668583241,-44.8280191071451,
-8.16439679231297));
#24170=CARTESIAN_POINT('Ctrl Pts',(-7.07057502873392,-44.6530191071451,
-4.082198396148));
#24171=CARTESIAN_POINT('Ctrl Pts',(-9.42743337163542,-44.4780191071451,
1.69768315121407E-11));
#24172=CARTESIAN_POINT('Ctrl Pts',(-7.07057502871922,-44.3030191071451,
4.08219839617346));
#24173=CARTESIAN_POINT('Ctrl Pts',(-4.71371668580301,-44.1280191071451,
8.16439679232994));
#24174=CARTESIAN_POINT('Ctrl Pts',(1.47018674401621E-11,-43.9530191071451,
8.16439679232146));
#24175=CARTESIAN_POINT('Ctrl Pts',(4.71371668583241,-43.7780191071451,8.16439679231297));
#24176=CARTESIAN_POINT('Ctrl Pts',(7.07057502873392,-43.6030191071451,4.082198396148));
#24177=CARTESIAN_POINT('Ctrl Pts',(9.42743337163542,-43.4280191071451,-1.69756769845304E-11));
#24178=CARTESIAN_POINT('Ctrl Pts',(7.07057502871922,-43.2530191071451,-4.08219839617346));
#24179=CARTESIAN_POINT('Ctrl Pts',(4.71371668580301,-43.0780191071451,-8.16439679232994));
#24180=CARTESIAN_POINT('Ctrl Pts',(-1.4702867290402E-11,-42.9030191071451,
-8.16439679232146));
#24181=CARTESIAN_POINT('Ctrl Pts',(-4.71371668583241,-42.7280191071451,
-8.16439679231297));
#24182=CARTESIAN_POINT('Ctrl Pts',(-7.07057502873392,-42.5530191071451,
-4.082198396148));
#24183=CARTESIAN_POINT('Ctrl Pts',(-9.42743337163542,-42.3780191071451,
1.69768315121407E-11));
#24184=CARTESIAN_POINT('Ctrl Pts',(-7.07057502871922,-42.2030191071451,
4.08219839617346));
#24185=CARTESIAN_POINT('Ctrl Pts',(-4.71371668580301,-42.0280191071451,
8.16439679232994));
#24186=CARTESIAN_POINT('Ctrl Pts',(1.47018674401621E-11,-41.8530191071451,
8.16439679232146));
#24187=CARTESIAN_POINT('Ctrl Pts',(4.71371668583241,-41.6780191071451,8.16439679231297));
#24188=CARTESIAN_POINT('Ctrl Pts',(7.07057502873392,-41.5030191071451,4.082198396148));
#24189=CARTESIAN_POINT('Ctrl Pts',(9.42743337163542,-41.3280191071451,-1.69756769845304E-11));
#24190=CARTESIAN_POINT('Ctrl Pts',(7.07057502871922,-41.1530191071451,-4.08219839617346));
#24191=CARTESIAN_POINT('Ctrl Pts',(4.71371668580301,-40.9780191071451,-8.16439679232994));
#24192=CARTESIAN_POINT('Ctrl Pts',(-1.4702867290402E-11,-40.8030191071451,
-8.16439679232146));
#24193=CARTESIAN_POINT('Ctrl Pts',(-4.71371668583241,-40.6280191071451,
-8.16439679231297));
#24194=CARTESIAN_POINT('Ctrl Pts',(-7.07057502873392,-40.4530191071451,
-4.082198396148));
#24195=CARTESIAN_POINT('Ctrl Pts',(-9.42743337163542,-40.2780191071451,
1.69768315121407E-11));
#24196=CARTESIAN_POINT('Ctrl Pts',(-7.07057502871922,-40.1030191071451,
4.08219839617346));
#24197=CARTESIAN_POINT('Ctrl Pts',(-4.71371668580301,-39.9280191071451,
8.16439679232994));
#24198=CARTESIAN_POINT('Ctrl Pts',(1.47018674401621E-11,-39.7530191071451,
8.16439679232146));
#24199=CARTESIAN_POINT('Ctrl Pts',(4.71371668583241,-39.5780191071451,8.16439679231297));
#24200=CARTESIAN_POINT('Ctrl Pts',(7.07057502873392,-39.4030191071451,4.082198396148));
#24201=CARTESIAN_POINT('Ctrl Pts',(9.42743337163542,-39.2280191071451,-1.69756769845304E-11));
#24202=CARTESIAN_POINT('Ctrl Pts',(7.07057502871922,-39.0530191071451,-4.08219839617346));
#24203=CARTESIAN_POINT('Ctrl Pts',(4.71371668580301,-38.8780191071451,-8.16439679232994));
#24204=CARTESIAN_POINT('Ctrl Pts',(-1.4702867290402E-11,-38.7030191071451,
-8.16439679232146));
#24205=CARTESIAN_POINT('Ctrl Pts',(-4.71371668583241,-38.5280191071451,
-8.16439679231297));
#24206=CARTESIAN_POINT('Ctrl Pts',(-7.07057502873392,-38.3530191071451,
-4.082198396148));
#24207=CARTESIAN_POINT('Ctrl Pts',(-9.42743337163542,-38.1780191071451,
1.69768315121407E-11));
#24208=CARTESIAN_POINT('Ctrl Pts',(-7.07057502871922,-38.0030191071451,
4.08219839617346));
#24209=CARTESIAN_POINT('Ctrl Pts',(-4.71371668580301,-37.8280191071451,
8.16439679232994));
#24210=CARTESIAN_POINT('Ctrl Pts',(1.47018674401621E-11,-37.6530191071451,
8.16439679232146));
#24211=CARTESIAN_POINT('Ctrl Pts',(4.71371668583241,-37.4780191071451,8.16439679231297));
#24212=CARTESIAN_POINT('Ctrl Pts',(7.07057502873392,-37.3030191071451,4.082198396148));
#24213=CARTESIAN_POINT('Ctrl Pts',(9.42743337163542,-37.1280191071451,-1.69756769845304E-11));
#24214=CARTESIAN_POINT('Ctrl Pts',(7.07057502871922,-36.9530191071451,-4.08219839617346));
#24215=CARTESIAN_POINT('Ctrl Pts',(4.71371668580301,-36.7780191071451,-8.16439679232994));
#24216=CARTESIAN_POINT('Ctrl Pts',(-1.4702867290402E-11,-36.6030191071451,
-8.16439679232146));
#24217=CARTESIAN_POINT('Ctrl Pts',(-4.71371668583241,-36.4280191071451,
-8.16439679231297));
#24218=CARTESIAN_POINT('Ctrl Pts',(-7.07057502873392,-36.2530191071451,
-4.082198396148));
#24219=CARTESIAN_POINT('Ctrl Pts',(-9.42743337163542,-36.0780191071451,
1.69768315121407E-11));
#24220=CARTESIAN_POINT('Ctrl Pts',(-7.07057502871922,-35.9030191071451,
4.08219839617346));
#24221=CARTESIAN_POINT('Ctrl Pts',(-4.71371668580301,-35.7280191071451,
8.16439679232994));
#24222=CARTESIAN_POINT('Ctrl Pts',(1.47018674401621E-11,-35.5530191071451,
8.16439679232146));
#24223=CARTESIAN_POINT('Ctrl Pts',(4.71371668583241,-35.3780191071451,8.16439679231297));
#24224=CARTESIAN_POINT('Ctrl Pts',(7.07057502873392,-35.2030191071451,4.082198396148));
#24225=CARTESIAN_POINT('Ctrl Pts',(9.42743337163542,-35.0280191071451,-1.69756769845304E-11));
#24226=CARTESIAN_POINT('Ctrl Pts',(7.07057502871922,-34.8530191071451,-4.08219839617346));
#24227=CARTESIAN_POINT('Ctrl Pts',(4.71371668580301,-34.6780191071451,-8.16439679232994));
#24228=CARTESIAN_POINT('Ctrl Pts',(-1.4702867290402E-11,-34.5030191071451,
-8.16439679232146));
#24229=CARTESIAN_POINT('Ctrl Pts',(-4.71371668583241,-34.3280191071451,
-8.16439679231297));
#24230=CARTESIAN_POINT('Ctrl Pts',(-7.07057502873392,-34.1530191071451,
-4.082198396148));
#24231=CARTESIAN_POINT('Ctrl Pts',(-9.42743337163542,-33.9780191071451,
1.69768315121407E-11));
#24232=CARTESIAN_POINT('Ctrl Pts',(-7.07057502871922,-33.8030191071451,
4.08219839617346));
#24233=CARTESIAN_POINT('Ctrl Pts',(-4.71371668580301,-33.6280191071451,
8.16439679232994));
#24234=CARTESIAN_POINT('Ctrl Pts',(1.47018674401621E-11,-33.4530191071451,
8.16439679232146));
#24235=CARTESIAN_POINT('Ctrl Pts',(4.71371668583241,-33.2780191071451,8.16439679231297));
#24236=CARTESIAN_POINT('Ctrl Pts',(7.07057502873392,-33.1030191071451,4.082198396148));
#24237=CARTESIAN_POINT('Ctrl Pts',(9.42743337163542,-32.9280191071451,-1.69756769845304E-11));
#24238=CARTESIAN_POINT('Ctrl Pts',(7.07057502871922,-32.7530191071451,-4.08219839617346));
#24239=CARTESIAN_POINT('Ctrl Pts',(4.71371668580301,-32.5780191071451,-8.16439679232994));
#24240=CARTESIAN_POINT('Ctrl Pts',(-1.4702867290402E-11,-32.4030191071451,
-8.16439679232146));
#24241=CARTESIAN_POINT('Ctrl Pts',(-4.71371668583241,-32.2280191071451,
-8.16439679231297));
#24242=CARTESIAN_POINT('Ctrl Pts',(-7.07057502873392,-32.0530191071451,
-4.082198396148));
#24243=CARTESIAN_POINT('Ctrl Pts',(-9.42743337163542,-31.8780191071451,
1.69768315121407E-11));
#24244=CARTESIAN_POINT('Ctrl Pts',(-7.07057502871922,-31.7030191071451,
4.08219839617346));
#24245=CARTESIAN_POINT('Ctrl Pts',(-4.71371668580301,-31.5280191071451,
8.16439679232994));
#24246=CARTESIAN_POINT('Ctrl Pts',(1.47018674401621E-11,-31.3530191071451,
8.16439679232146));
#24247=CARTESIAN_POINT('Ctrl Pts',(4.71371668583241,-31.1780191071451,8.16439679231297));
#24248=CARTESIAN_POINT('Ctrl Pts',(7.07057502873392,-31.0030191071451,4.082198396148));
#24249=CARTESIAN_POINT('Ctrl Pts',(9.42743337163542,-30.8280191071451,-1.69756769845304E-11));
#24250=CARTESIAN_POINT('Ctrl Pts',(7.07057502871922,-30.6530191071451,-4.08219839617346));
#24251=CARTESIAN_POINT('Ctrl Pts',(4.71371668580301,-30.4780191071451,-8.16439679232994));
#24252=CARTESIAN_POINT('Ctrl Pts',(-1.4702867290402E-11,-30.3030191071451,
-8.16439679232146));
#24253=CARTESIAN_POINT('Ctrl Pts',(-4.71371668583241,-30.1280191071451,
-8.16439679231297));
#24254=CARTESIAN_POINT('Ctrl Pts',(-7.07057502873392,-29.9530191071451,
-4.082198396148));
#24255=CARTESIAN_POINT('Ctrl Pts',(-9.42743337163542,-29.7780191071451,
1.69768315121407E-11));
#24256=CARTESIAN_POINT('Ctrl Pts',(-7.07057502871922,-29.6030191071451,
4.08219839617346));
#24257=CARTESIAN_POINT('Ctrl Pts',(-4.71371668580301,-29.4280191071451,
8.16439679232994));
#24258=CARTESIAN_POINT('Ctrl Pts',(1.47018674401621E-11,-29.2530191071451,
8.16439679232146));
#24259=CARTESIAN_POINT('Ctrl Pts',(4.71371668583241,-29.0780191071451,8.16439679231297));
#24260=CARTESIAN_POINT('Ctrl Pts',(7.07057502873392,-28.9030191071451,4.082198396148));
#24261=CARTESIAN_POINT('Ctrl Pts',(9.42743337163542,-28.7280191071451,-1.69756769845304E-11));
#24262=CARTESIAN_POINT('Ctrl Pts',(7.07057502871922,-28.5530191071451,-4.08219839617346));
#24263=CARTESIAN_POINT('Ctrl Pts',(4.71371668580301,-28.3780191071451,-8.16439679232994));
#24264=CARTESIAN_POINT('Ctrl Pts',(-1.4702867290402E-11,-28.2030191071451,
-8.16439679232146));
#24265=CARTESIAN_POINT('Ctrl Pts',(-4.71371668583241,-28.0280191071451,
-8.16439679231297));
#24266=CARTESIAN_POINT('Ctrl Pts',(-7.07057502873392,-27.8530191071451,
-4.082198396148));
#24267=CARTESIAN_POINT('Ctrl Pts',(-9.42743337163542,-27.6780191071451,
1.69768315121407E-11));
#24268=CARTESIAN_POINT('Ctrl Pts',(-7.07057502871922,-27.5030191071451,
4.08219839617346));
#24269=CARTESIAN_POINT('Ctrl Pts',(-4.71371668580301,-27.3280191071451,
8.16439679232994));
#24270=CARTESIAN_POINT('Ctrl Pts',(1.47018674401621E-11,-27.1530191071451,
8.16439679232146));
#24271=CARTESIAN_POINT('Ctrl Pts',(4.71371668583241,-26.9780191071451,8.16439679231297));
#24272=CARTESIAN_POINT('Ctrl Pts',(7.07057502873392,-26.8030191071451,4.082198396148));
#24273=CARTESIAN_POINT('Ctrl Pts',(9.42743337163542,-26.6280191071451,-1.69756769845304E-11));
#24274=CARTESIAN_POINT('Ctrl Pts',(7.07057502871922,-26.4530191071451,-4.08219839617346));
#24275=CARTESIAN_POINT('Ctrl Pts',(4.71371668580301,-26.2780191071451,-8.16439679232994));
#24276=CARTESIAN_POINT('Ctrl Pts',(-1.4702867290402E-11,-26.1030191071451,
-8.16439679232146));
#24277=CARTESIAN_POINT('Ctrl Pts',(-4.71371668583241,-25.9280191071451,
-8.16439679231297));
#24278=CARTESIAN_POINT('Ctrl Pts',(-7.07057502873392,-25.7530191071451,
-4.082198396148));
#24279=CARTESIAN_POINT('Ctrl Pts',(-9.42743337163542,-25.5780191071451,
1.69768315121407E-11));
#24280=CARTESIAN_POINT('Ctrl Pts',(-7.07057502871922,-25.4030191071451,
4.08219839617346));
#24281=CARTESIAN_POINT('Ctrl Pts',(-4.71371668580301,-25.2280191071451,
8.16439679232994));
#24282=CARTESIAN_POINT('Ctrl Pts',(1.47018674401621E-11,-25.0530191071451,
8.16439679232146));
#24283=CARTESIAN_POINT('Ctrl Pts',(4.71371668583241,-24.8780191071451,8.16439679231297));
#24284=CARTESIAN_POINT('Ctrl Pts',(7.07057502873392,-24.7030191071451,4.082198396148));
#24285=CARTESIAN_POINT('Ctrl Pts',(9.42743337163542,-24.5280191071451,-1.69756769845304E-11));
#24286=CARTESIAN_POINT('Ctrl Pts',(7.07057502871922,-24.3530191071451,-4.08219839617346));
#24287=CARTESIAN_POINT('Ctrl Pts',(4.71371668580301,-24.1780191071451,-8.16439679232994));
#24288=CARTESIAN_POINT('Ctrl Pts',(-1.4702867290402E-11,-24.0030191071451,
-8.16439679232146));
#24289=CARTESIAN_POINT('Ctrl Pts',(-4.71371668583241,-23.8280191071451,
-8.16439679231297));
#24290=CARTESIAN_POINT('Ctrl Pts',(-7.07057502873392,-23.6530191071451,
-4.082198396148));
#24291=CARTESIAN_POINT('Ctrl Pts',(-9.42743337163542,-23.4780191071451,
1.69768315121407E-11));
#24292=CARTESIAN_POINT('Ctrl Pts',(-7.07057502871922,-23.3030191071451,
4.08219839617346));
#24293=CARTESIAN_POINT('Ctrl Pts',(-4.71371668580301,-23.1280191071451,
8.16439679232994));
#24294=CARTESIAN_POINT('Ctrl Pts',(1.47018674401621E-11,-22.9530191071451,
8.16439679232146));
#24295=CARTESIAN_POINT('Ctrl Pts',(4.71371668583241,-22.7780191071451,8.16439679231297));
#24296=CARTESIAN_POINT('Ctrl Pts',(7.07057502873392,-22.6030191071451,4.082198396148));
#24297=CARTESIAN_POINT('Ctrl Pts',(9.42743337163542,-22.4280191071451,-1.69756769845304E-11));
#24298=CARTESIAN_POINT('Ctrl Pts',(7.07057502871922,-22.2530191071451,-4.08219839617346));
#24299=CARTESIAN_POINT('Ctrl Pts',(4.71371668580301,-22.0780191071451,-8.16439679232994));
#24300=CARTESIAN_POINT('Ctrl Pts',(-1.4702867290402E-11,-21.9030191071451,
-8.16439679232146));
#24301=CARTESIAN_POINT('Ctrl Pts',(-4.71371668583241,-21.7280191071451,
-8.16439679231297));
#24302=CARTESIAN_POINT('Ctrl Pts',(-7.07057502873392,-21.5530191071451,
-4.082198396148));
#24303=CARTESIAN_POINT('Ctrl Pts',(-9.42743337163542,-21.3780191071451,
1.69768315121407E-11));
#24304=CARTESIAN_POINT('Ctrl Pts',(-7.07057502871922,-21.2030191071451,
4.08219839617346));
#24305=CARTESIAN_POINT('Ctrl Pts',(-4.71371668580301,-21.0280191071451,
8.16439679232994));
#24306=CARTESIAN_POINT('Ctrl Pts',(1.47018674401621E-11,-20.8530191071451,
8.16439679232146));
#24307=CARTESIAN_POINT('Ctrl Pts',(4.71371668583241,-20.6780191071451,8.16439679231297));
#24308=CARTESIAN_POINT('Ctrl Pts',(7.07057502873392,-20.5030191071451,4.082198396148));
#24309=CARTESIAN_POINT('Ctrl Pts',(9.42743337163542,-20.3280191071451,-1.69756769845304E-11));
#24310=CARTESIAN_POINT('Ctrl Pts',(7.07057502871922,-20.1530191071451,-4.08219839617346));
#24311=CARTESIAN_POINT('Ctrl Pts',(4.71371668580301,-19.9780191071451,-8.16439679232994));
#24312=CARTESIAN_POINT('Ctrl Pts',(-1.4702867290402E-11,-19.8030191071451,
-8.16439679232146));
#24313=CARTESIAN_POINT('Ctrl Pts',(-4.71371668583241,-19.6280191071451,
-8.16439679231297));
#24314=CARTESIAN_POINT('Ctrl Pts',(-7.07057502873392,-19.4530191071451,
-4.082198396148));
#24315=CARTESIAN_POINT('Ctrl Pts',(-9.42743337163542,-19.2780191071451,
1.69768315121407E-11));
#24316=CARTESIAN_POINT('Ctrl Pts',(-7.07057502871922,-19.1030191071451,
4.08219839617346));
#24317=CARTESIAN_POINT('Ctrl Pts',(-4.71371668580301,-18.9280191071451,
8.16439679232994));
#24318=CARTESIAN_POINT('Ctrl Pts',(1.47018674401621E-11,-18.7530191071451,
8.16439679232146));
#24319=CARTESIAN_POINT('Ctrl Pts',(4.71371668583241,-18.5780191071451,8.16439679231297));
#24320=CARTESIAN_POINT('Ctrl Pts',(7.07057502873392,-18.4030191071451,4.082198396148));
#24321=CARTESIAN_POINT('Ctrl Pts',(9.42743337163542,-18.2280191071451,-1.69756769845304E-11));
#24322=CARTESIAN_POINT('Ctrl Pts',(7.07057502871922,-18.0530191071451,-4.08219839617346));
#24323=CARTESIAN_POINT('Ctrl Pts',(4.71371668580301,-17.8780191071451,-8.16439679232994));
#24324=CARTESIAN_POINT('Ctrl Pts',(-1.4702867290402E-11,-17.7030191071451,
-8.16439679232146));
#24325=CARTESIAN_POINT('Ctrl Pts',(-4.71371668583241,-17.5280191071451,
-8.16439679231297));
#24326=CARTESIAN_POINT('Ctrl Pts',(-7.07057502873392,-17.3530191071451,
-4.082198396148));
#24327=CARTESIAN_POINT('Ctrl Pts',(-9.42743337163542,-17.1780191071451,
1.69768315121407E-11));
#24328=CARTESIAN_POINT('Ctrl Pts',(-7.07057502871922,-17.0030191071451,
4.08219839617346));
#24329=CARTESIAN_POINT('Ctrl Pts',(-4.71371668580301,-16.8280191071451,
8.16439679232994));
#24330=CARTESIAN_POINT('Ctrl Pts',(1.47018674401621E-11,-16.6530191071451,
8.16439679232146));
#24331=CARTESIAN_POINT('Ctrl Pts',(4.71371668583241,-16.4780191071451,8.16439679231297));
#24332=CARTESIAN_POINT('Ctrl Pts',(7.07057502873392,-16.3030191071451,4.082198396148));
#24333=CARTESIAN_POINT('Ctrl Pts',(9.42743337163542,-16.1280191071451,-1.69756769845304E-11));
#24334=CARTESIAN_POINT('Ctrl Pts',(7.07057502871922,-15.9530191071451,-4.08219839617346));
#24335=CARTESIAN_POINT('Ctrl Pts',(4.71371668580301,-15.7780191071451,-8.16439679232994));
#24336=CARTESIAN_POINT('Ctrl Pts',(-1.4702867290402E-11,-15.6030191071451,
-8.16439679232146));
#24337=CARTESIAN_POINT('Ctrl Pts',(-4.71371668583241,-15.4280191071451,
-8.16439679231297));
#24338=CARTESIAN_POINT('Ctrl Pts',(-7.07057502873392,-15.2530191071451,
-4.082198396148));
#24339=CARTESIAN_POINT('Ctrl Pts',(-9.42743337163542,-15.0780191071451,
1.69768315121407E-11));
#24340=CARTESIAN_POINT('Ctrl Pts',(-7.07057502871922,-14.9030191071451,
4.08219839617346));
#24341=CARTESIAN_POINT('Ctrl Pts',(-4.71371668580301,-14.7280191071451,
8.16439679232994));
#24342=CARTESIAN_POINT('Ctrl Pts',(1.47018674401621E-11,-14.5530191071451,
8.16439679232146));
#24343=CARTESIAN_POINT('Ctrl Pts',(4.71371668583241,-14.3780191071451,8.16439679231297));
#24344=CARTESIAN_POINT('Ctrl Pts',(7.07057502873392,-14.2030191071451,4.082198396148));
#24345=CARTESIAN_POINT('Ctrl Pts',(9.42743337163542,-14.0280191071451,-1.69756769845304E-11));
#24346=CARTESIAN_POINT('Ctrl Pts',(7.07057502871922,-13.8530191071451,-4.08219839617346));
#24347=CARTESIAN_POINT('Ctrl Pts',(4.71371668580301,-13.6780191071451,-8.16439679232994));
#24348=CARTESIAN_POINT('Ctrl Pts',(-1.4702867290402E-11,-13.5030191071451,
-8.16439679232146));
#24349=CARTESIAN_POINT('Ctrl Pts',(-4.71371668583241,-13.3280191071452,
-8.16439679231297));
#24350=CARTESIAN_POINT('Ctrl Pts',(-7.07057502873392,-13.1530191071451,
-4.082198396148));
#24351=CARTESIAN_POINT('Ctrl Pts',(-9.42743337163542,-12.9780191071451,
1.69768315121407E-11));
#24352=CARTESIAN_POINT('Ctrl Pts',(-7.07057502871922,-12.8030191071452,
4.08219839617346));
#24353=CARTESIAN_POINT('Ctrl Pts',(-4.71371668580301,-12.6280191071451,
8.16439679232994));
#24354=CARTESIAN_POINT('Ctrl Pts',(1.47018674401621E-11,-12.4530191071451,
8.16439679232146));
#24355=CARTESIAN_POINT('Ctrl Pts',(4.71371668583241,-12.2780191071452,8.16439679231297));
#24356=CARTESIAN_POINT('Ctrl Pts',(7.07057502873392,-12.1030191071451,4.082198396148));
#24357=CARTESIAN_POINT('Ctrl Pts',(9.42743337163542,-11.9280191071451,-1.69756769845304E-11));
#24358=CARTESIAN_POINT('Ctrl Pts',(7.07057502871922,-11.7530191071452,-4.08219839617346));
#24359=CARTESIAN_POINT('Ctrl Pts',(4.71371668580301,-11.5780191071452,-8.16439679232994));
#24360=CARTESIAN_POINT('Ctrl Pts',(-1.4702867290402E-11,-11.4030191071451,
-8.16439679232146));
#24361=CARTESIAN_POINT('Ctrl Pts',(-4.71371668583241,-11.2280191071451,
-8.16439679231297));
#24362=CARTESIAN_POINT('Ctrl Pts',(-7.07057502873392,-11.0530191071452,
-4.082198396148));
#24363=CARTESIAN_POINT('Ctrl Pts',(-9.42743337163542,-10.8780191071451,
1.69768315121407E-11));
#24364=CARTESIAN_POINT('Ctrl Pts',(-7.07057502871922,-10.7030191071451,
4.08219839617346));
#24365=CARTESIAN_POINT('Ctrl Pts',(-4.71371668580301,-10.5280191071452,
8.16439679232994));
#24366=CARTESIAN_POINT('Ctrl Pts',(1.47018674401621E-11,-10.3530191071451,
8.16439679232146));
#24367=CARTESIAN_POINT('Ctrl Pts',(4.71371668583241,-10.1780191071451,8.16439679231297));
#24368=CARTESIAN_POINT('Ctrl Pts',(7.07057502873392,-10.0030191071452,4.082198396148));
#24369=CARTESIAN_POINT('Ctrl Pts',(9.42743337163542,-9.82801910714514,-1.69756769845304E-11));
#24370=CARTESIAN_POINT('Ctrl Pts',(7.07057502871922,-9.65301910714514,-4.08219839617346));
#24371=CARTESIAN_POINT('Ctrl Pts',(4.71371668580301,-9.47801910714516,-8.16439679232994));
#24372=CARTESIAN_POINT('Ctrl Pts',(-1.4702867290402E-11,-9.30301910714514,
-8.16439679232146));
#24373=CARTESIAN_POINT('Ctrl Pts',(-4.71371668583241,-9.12801910714515,
-8.16439679231297));
#24374=CARTESIAN_POINT('Ctrl Pts',(-7.07057502873392,-8.95301910714516,
-4.082198396148));
#24375=CARTESIAN_POINT('Ctrl Pts',(-9.42743337163542,-8.77801910714516,
1.69768315121407E-11));
#24376=CARTESIAN_POINT('Ctrl Pts',(-7.07057502871922,-8.60301910714514,
4.08219839617346));
#24377=CARTESIAN_POINT('Ctrl Pts',(-4.71371668580301,-8.42801910714516,
8.16439679232994));
#24378=CARTESIAN_POINT('Ctrl Pts',(1.47018674401621E-11,-8.25301910714516,
8.16439679232146));
#24379=CARTESIAN_POINT('Ctrl Pts',(4.71371668583241,-8.07801910714515,8.16439679231297));
#24380=CARTESIAN_POINT('Ctrl Pts',(7.07057502873392,-7.90301910714516,4.082198396148));
#24381=CARTESIAN_POINT('Ctrl Pts',(9.42743337163542,-7.72801910714516,-1.69756769845304E-11));
#24382=CARTESIAN_POINT('Ctrl Pts',(7.07057502871922,-7.55301910714514,-4.08219839617346));
#24383=CARTESIAN_POINT('Ctrl Pts',(4.71371668580301,-7.37801910714516,-8.16439679232994));
#24384=CARTESIAN_POINT('Ctrl Pts',(-1.4702867290402E-11,-7.20301910714516,
-8.16439679232146));
#24385=CARTESIAN_POINT('Ctrl Pts',(-4.71371668583241,-7.02801910714516,
-8.16439679231297));
#24386=CARTESIAN_POINT('Ctrl Pts',(-7.07057502873392,-6.85301910714514,
-4.082198396148));
#24387=CARTESIAN_POINT('Ctrl Pts',(-9.42743337163542,-6.67801910714516,
1.69768315121407E-11));
#24388=CARTESIAN_POINT('Ctrl Pts',(-7.07057502871922,-6.50301910714514,
4.08219839617346));
#24389=CARTESIAN_POINT('Ctrl Pts',(-4.71371668580301,-6.32801910714515,
8.16439679232994));
#24390=CARTESIAN_POINT('Ctrl Pts',(1.47018674401621E-11,-6.15301910714516,
8.16439679232146));
#24391=CARTESIAN_POINT('Ctrl Pts',(4.71371668583241,-5.97801910714516,8.16439679231297));
#24392=CARTESIAN_POINT('Ctrl Pts',(7.07057502873392,-5.80301910714515,4.082198396148));
#24393=CARTESIAN_POINT('Ctrl Pts',(9.42743337163542,-5.62801910714516,-1.69756769845304E-11));
#24394=CARTESIAN_POINT('Ctrl Pts',(7.07057502871922,-5.45301910714515,-4.08219839617346));
#24395=CARTESIAN_POINT('Ctrl Pts',(4.71371668580301,-5.27801910714516,-8.16439679232994));
#24396=CARTESIAN_POINT('Ctrl Pts',(-1.4702867290402E-11,-5.10301910714516,
-8.16439679232146));
#24397=CARTESIAN_POINT('Ctrl Pts',(-4.71371668583241,-4.92801910714516,
-8.16439679231297));
#24398=CARTESIAN_POINT('Ctrl Pts',(-7.07057502873392,-4.75301910714515,
-4.082198396148));
#24399=CARTESIAN_POINT('Ctrl Pts',(-9.42743337163542,-4.57801910714517,
1.69768315121407E-11));
#24400=CARTESIAN_POINT('Ctrl Pts',(-7.07057502871922,-4.40301910714516,
4.08219839617346));
#24401=CARTESIAN_POINT('Ctrl Pts',(-4.71371668580301,-4.22801910714516,
8.16439679232994));
#24402=CARTESIAN_POINT('Ctrl Pts',(1.47018674401621E-11,-4.05301910714517,
8.16439679232146));
#24403=CARTESIAN_POINT('Ctrl Pts',(4.71371668583241,-3.87801910714518,8.16439679231297));
#24404=CARTESIAN_POINT('Ctrl Pts',(7.07057502873392,-3.70301910714515,4.082198396148));
#24405=CARTESIAN_POINT('Ctrl Pts',(9.42743337163542,-3.52801910714518,-1.69756769845304E-11));
#24406=CARTESIAN_POINT('Ctrl Pts',(7.07057502871922,-3.35301910714517,-4.08219839617346));
#24407=CARTESIAN_POINT('Ctrl Pts',(4.71371668580301,-3.17801910714516,-8.16439679232994));
#24408=CARTESIAN_POINT('Ctrl Pts',(-1.4702867290402E-11,-3.00301910714517,
-8.16439679232146));
#24409=CARTESIAN_POINT('Ctrl Pts',(-4.71371668583241,-2.82801910714518,
-8.16439679231297));
#24410=CARTESIAN_POINT('Ctrl Pts',(-7.07057502873392,-2.65301910714515,
-4.082198396148));
#24411=CARTESIAN_POINT('Ctrl Pts',(-9.42743337163542,-2.47801910714516,
1.69768315121407E-11));
#24412=CARTESIAN_POINT('Ctrl Pts',(-7.07057502871922,-2.30301910714517,
4.08219839617346));
#24413=CARTESIAN_POINT('Ctrl Pts',(-4.71371668580301,-2.12801910714516,
8.16439679232994));
#24414=CARTESIAN_POINT('Ctrl Pts',(1.47018674401621E-11,-1.95301910714515,
8.16439679232146));
#24415=CARTESIAN_POINT('Ctrl Pts',(4.71371668583241,-1.77801910714518,8.16439679231297));
#24416=CARTESIAN_POINT('Ctrl Pts',(7.07057502873392,-1.60301910714516,4.082198396148));
#24417=CARTESIAN_POINT('Ctrl Pts',(9.42743337163542,-1.42801910714516,-1.69756769845304E-11));
#24418=CARTESIAN_POINT('Ctrl Pts',(7.07057502871922,-1.25301910714517,-4.08219839617346));
#24419=CARTESIAN_POINT('Ctrl Pts',(4.71371668580301,-1.07801910714517,-8.16439679232994));
#24420=CARTESIAN_POINT('Ctrl Pts',(-1.4702867290402E-11,-0.903019107145155,
-8.16439679232146));
#24421=CARTESIAN_POINT('Ctrl Pts',(-4.71371668583241,-0.728019107145183,
-8.16439679231297));
#24422=CARTESIAN_POINT('Ctrl Pts',(-7.07057502873392,-0.553019107145171,
-4.082198396148));
#24423=CARTESIAN_POINT('Ctrl Pts',(-9.42743337163542,-0.378019107145163,
1.69768315121407E-11));
#24424=CARTESIAN_POINT('Ctrl Pts',(-7.07057502871922,-0.203019107145175,
4.08219839617346));
#24425=CARTESIAN_POINT('Ctrl Pts',(-4.71371668580301,-0.0280191071451809,
8.16439679232994));
#24426=CARTESIAN_POINT('Ctrl Pts',(1.47018674401621E-11,0.146980892854842,
8.16439679232146));
#24427=CARTESIAN_POINT('Ctrl Pts',(4.71371668583241,0.321980892854814,8.16439679231297));
#24428=CARTESIAN_POINT('Ctrl Pts',(7.07057502873392,0.496980892854826,4.082198396148));
#24429=CARTESIAN_POINT('Ctrl Pts',(9.42743337163542,0.671980892854834,-1.69756769845304E-11));
#24430=CARTESIAN_POINT('Ctrl Pts',(7.07057502871922,0.846980892854822,-4.08219839617346));
#24431=CARTESIAN_POINT('Ctrl Pts',(4.71371668580301,1.02198089285482,-8.16439679232994));
#24432=CARTESIAN_POINT('Ctrl Pts',(-1.4702867290402E-11,1.19698089285484,
-8.16439679232146));
#24433=CARTESIAN_POINT('Ctrl Pts',(-4.71371668583241,1.37198089285481,-8.16439679231297));
#24434=CARTESIAN_POINT('Ctrl Pts',(-7.07057502873392,1.54698089285482,-4.082198396148));
#24435=CARTESIAN_POINT('Ctrl Pts',(-9.42743337163542,1.72198089285483,1.69768315121407E-11));
#24436=CARTESIAN_POINT('Ctrl Pts',(-7.07057502871922,1.89698089285484,4.08219839617346));
#24437=CARTESIAN_POINT('Ctrl Pts',(-4.71371668580301,2.07198089285481,8.16439679232994));
#24438=CARTESIAN_POINT('Ctrl Pts',(1.47018674401621E-11,2.24698089285484,
8.16439679232146));
#24439=CARTESIAN_POINT('Ctrl Pts',(4.71371668583241,2.42198089285483,8.16439679231297));
#24440=CARTESIAN_POINT('Ctrl Pts',(7.07057502873392,2.59698089285482,4.082198396148));
#24441=CARTESIAN_POINT('Ctrl Pts',(9.42743337163542,2.77198089285483,-1.69756769845304E-11));
#24442=CARTESIAN_POINT('Ctrl Pts',(7.07057502871922,2.94698089285484,-4.08219839617346));
#24443=CARTESIAN_POINT('Ctrl Pts',(4.71371668580301,3.12198089285481,-8.16439679232994));
#24444=CARTESIAN_POINT('Ctrl Pts',(-1.4702867290402E-11,3.29698089285482,
-8.16439679232146));
#24445=CARTESIAN_POINT('Ctrl Pts',(-4.71371668583241,3.47198089285483,-8.16439679231297));
#24446=CARTESIAN_POINT('Ctrl Pts',(-7.07057502873392,3.64698089285482,-4.082198396148));
#24447=CARTESIAN_POINT('Ctrl Pts',(-9.42743337163542,3.82198089285481,1.69768315121407E-11));
#24448=CARTESIAN_POINT('Ctrl Pts',(-7.07057502871922,3.99698089285483,4.08219839617346));
#24449=CARTESIAN_POINT('Ctrl Pts',(-4.71371668580301,4.17198089285481,8.16439679232994));
#24450=CARTESIAN_POINT('Ctrl Pts',(1.47018674401621E-11,4.34698089285482,
8.16439679232146));
#24451=CARTESIAN_POINT('Ctrl Pts',(4.71371668583241,4.52198089285483,8.16439679231297));
#24452=CARTESIAN_POINT('Ctrl Pts',(7.07057502873392,4.69698089285481,4.082198396148));
#24453=CARTESIAN_POINT('Ctrl Pts',(9.42743337163542,4.87198089285481,-1.69756769845304E-11));
#24454=CARTESIAN_POINT('Ctrl Pts',(7.07057502871922,5.04698089285483,-4.08219839617346));
#24455=CARTESIAN_POINT('Ctrl Pts',(4.71371668580301,5.22198089285481,-8.16439679232994));
#24456=CARTESIAN_POINT('Ctrl Pts',(-1.4702867290402E-11,5.39698089285482,
-8.16439679232146));
#24457=CARTESIAN_POINT('Ctrl Pts',(-4.71371668583241,5.57198089285483,-8.16439679231297));
#24458=CARTESIAN_POINT('Ctrl Pts',(-7.07057502873392,5.74698089285481,-4.082198396148));
#24459=CARTESIAN_POINT('Ctrl Pts',(-9.42743337163542,5.92198089285481,1.69768315121407E-11));
#24460=CARTESIAN_POINT('Ctrl Pts',(-7.07057502871922,6.09698089285483,4.08219839617346));
#24461=CARTESIAN_POINT('Ctrl Pts',(-4.71371668580301,6.2719808928548,8.16439679232994));
#24462=CARTESIAN_POINT('Ctrl Pts',(1.47018674401621E-11,6.44698089285481,
8.16439679232146));
#24463=CARTESIAN_POINT('Ctrl Pts',(4.71371668583241,6.62198089285482,8.16439679231297));
#24464=CARTESIAN_POINT('Ctrl Pts',(7.07057502873392,6.79698089285483,4.082198396148));
#24465=CARTESIAN_POINT('Ctrl Pts',(9.42743337163542,6.97198089285481,-1.69756769845304E-11));
#24466=CARTESIAN_POINT('Ctrl Pts',(7.07057502871922,7.14698089285482,-4.08219839617346));
#24467=CARTESIAN_POINT('Ctrl Pts',(4.71371668580301,7.32198089285482,-8.16439679232994));
#24468=CARTESIAN_POINT('Ctrl Pts',(-1.4702867290402E-11,7.49698089285481,
-8.16439679232146));
#24469=CARTESIAN_POINT('Ctrl Pts',(-4.71371668583241,7.67198089285481,-8.16439679231297));
#24470=CARTESIAN_POINT('Ctrl Pts',(-7.07057502873392,7.84698089285483,-4.082198396148));
#24471=CARTESIAN_POINT('Ctrl Pts',(-9.42743337163542,8.0219808928548,1.69768315121407E-11));
#24472=CARTESIAN_POINT('Ctrl Pts',(-7.07057502871922,8.19698089285481,4.08219839617346));
#24473=CARTESIAN_POINT('Ctrl Pts',(-4.71371668580301,8.37198089285483,8.16439679232994));
#24474=CARTESIAN_POINT('Ctrl Pts',(1.47018674401621E-11,8.54698089285481,
8.16439679232146));
#24475=CARTESIAN_POINT('Ctrl Pts',(4.71371668583241,8.72198089285481,8.16439679231297));
#24476=CARTESIAN_POINT('Ctrl Pts',(7.07057502873392,8.89698089285482,4.082198396148));
#24477=CARTESIAN_POINT('Ctrl Pts',(9.42743337163542,9.0719808928548,-1.69756769845304E-11));
#24478=CARTESIAN_POINT('Ctrl Pts',(7.07057502871922,9.24698089285481,-4.08219839617346));
#24479=CARTESIAN_POINT('Ctrl Pts',(4.71371668580301,9.42198089285482,-8.16439679232994));
#24480=CARTESIAN_POINT('Ctrl Pts',(-1.4702867290402E-11,9.5969808928548,
-8.16439679232146));
#24481=CARTESIAN_POINT('Ctrl Pts',(-4.71371668583241,9.7719808928548,-8.16439679231297));
#24482=CARTESIAN_POINT('Ctrl Pts',(-7.07057502873392,9.94698089285482,-4.082198396148));
#24483=CARTESIAN_POINT('Ctrl Pts',(-9.42743337163542,10.1219808928548,1.69768315121407E-11));
#24484=CARTESIAN_POINT('Ctrl Pts',(-7.07057502871922,10.2969808928548,4.08219839617346));
#24485=CARTESIAN_POINT('Ctrl Pts',(-4.71371668580301,10.4719808928548,8.16439679232994));
#24486=CARTESIAN_POINT('Ctrl Pts',(1.47018674401621E-11,10.6469808928548,
8.16439679232146));
#24487=CARTESIAN_POINT('Ctrl Pts',(4.71371668583241,10.8219808928548,8.16439679231297));
#24488=CARTESIAN_POINT('Ctrl Pts',(7.07057502873392,10.9969808928548,4.082198396148));
#24489=CARTESIAN_POINT('Ctrl Pts',(9.42743337163542,11.1719808928548,-1.69756769845304E-11));
#24490=CARTESIAN_POINT('Ctrl Pts',(7.07057502871922,11.3469808928548,-4.08219839617346));
#24491=CARTESIAN_POINT('Ctrl Pts',(4.71371668580301,11.5219808928548,-8.16439679232994));
#24492=CARTESIAN_POINT('Ctrl Pts',(-1.4702867290402E-11,11.6969808928548,
-8.16439679232146));
#24493=CARTESIAN_POINT('Ctrl Pts',(-4.71371668583241,11.8719808928548,-8.16439679231297));
#24494=CARTESIAN_POINT('Ctrl Pts',(-7.07057502873392,12.0469808928548,-4.082198396148));
#24495=CARTESIAN_POINT('Ctrl Pts',(-9.42743337163542,12.2219808928548,1.69768315121407E-11));
#24496=CARTESIAN_POINT('Ctrl Pts',(-7.07057502871922,12.3969808928548,4.08219839617346));
#24497=CARTESIAN_POINT('Ctrl Pts',(-4.71371668580301,12.5719808928548,8.16439679232994));
#24498=CARTESIAN_POINT('Ctrl Pts',(1.47018674401621E-11,12.7469808928548,
8.16439679232146));
#24499=CARTESIAN_POINT('Ctrl Pts',(4.71371668583241,12.9219808928548,8.16439679231297));
#24500=CARTESIAN_POINT('Ctrl Pts',(7.07057502873392,13.0969808928548,4.082198396148));
#24501=CARTESIAN_POINT('Ctrl Pts',(9.42743337163542,13.2719808928548,-1.69756769845304E-11));
#24502=CARTESIAN_POINT('Ctrl Pts',(7.07057502871922,13.4469808928548,-4.08219839617346));
#24503=CARTESIAN_POINT('Ctrl Pts',(4.71371668580301,13.6219808928548,-8.16439679232994));
#24504=CARTESIAN_POINT('Ctrl Pts',(-1.4702867290402E-11,13.7969808928548,
-8.16439679232146));
#24505=CARTESIAN_POINT('Ctrl Pts',(-4.71371668583241,13.9719808928548,-8.16439679231297));
#24506=CARTESIAN_POINT('Ctrl Pts',(-7.07057502873392,14.1469808928548,-4.082198396148));
#24507=CARTESIAN_POINT('Ctrl Pts',(-9.42743337163542,14.3219808928548,1.69768315121407E-11));
#24508=CARTESIAN_POINT('Ctrl Pts',(-7.07057502871922,14.4969808928548,4.08219839617346));
#24509=CARTESIAN_POINT('Ctrl Pts',(-4.71371668580301,14.6719808928548,8.16439679232994));
#24510=CARTESIAN_POINT('Ctrl Pts',(1.47018674401621E-11,14.8469808928548,
8.16439679232146));
#24511=CARTESIAN_POINT('Ctrl Pts',(4.71371668583241,15.0219808928548,8.16439679231297));
#24512=CARTESIAN_POINT('Ctrl Pts',(7.07057502873392,15.1969808928548,4.082198396148));
#24513=CARTESIAN_POINT('Ctrl Pts',(9.42743337163542,15.3719808928548,-1.69756769845304E-11));
#24514=CARTESIAN_POINT('Ctrl Pts',(7.07057502871922,15.5469808928548,-4.08219839617346));
#24515=CARTESIAN_POINT('Ctrl Pts',(4.71371668580301,15.7219808928548,-8.16439679232994));
#24516=CARTESIAN_POINT('Ctrl Pts',(-1.4702867290402E-11,15.8969808928548,
-8.16439679232146));
#24517=CARTESIAN_POINT('Ctrl Pts',(-4.71371668583241,16.0719808928548,-8.16439679231297));
#24518=CARTESIAN_POINT('Ctrl Pts',(-7.07057502873392,16.2469808928548,-4.082198396148));
#24519=CARTESIAN_POINT('Ctrl Pts',(-9.42743337163542,16.4219808928548,1.69768315121407E-11));
#24520=CARTESIAN_POINT('Ctrl Pts',(-7.07057502871922,16.5969808928548,4.08219839617346));
#24521=CARTESIAN_POINT('Ctrl Pts',(-4.71371668580301,16.7719808928548,8.16439679232994));
#24522=CARTESIAN_POINT('Ctrl Pts',(1.47018674401621E-11,16.9469808928548,
8.16439679232146));
#24523=CARTESIAN_POINT('Ctrl Pts',(4.71371668583241,17.1219808928548,8.16439679231297));
#24524=CARTESIAN_POINT('Ctrl Pts',(7.07057502873392,17.2969808928548,4.082198396148));
#24525=CARTESIAN_POINT('Ctrl Pts',(9.42743337163542,17.4719808928548,-1.69756769845304E-11));
#24526=CARTESIAN_POINT('Ctrl Pts',(7.07057502871922,17.6469808928548,-4.08219839617346));
#24527=CARTESIAN_POINT('Ctrl Pts',(4.71371668580301,17.8219808928548,-8.16439679232994));
#24528=CARTESIAN_POINT('Ctrl Pts',(-1.4702867290402E-11,17.9969808928548,
-8.16439679232146));
#24529=CARTESIAN_POINT('Ctrl Pts',(-4.71371668583241,18.1719808928548,-8.16439679231297));
#24530=CARTESIAN_POINT('Ctrl Pts',(-7.07057502873392,18.3469808928548,-4.082198396148));
#24531=CARTESIAN_POINT('Ctrl Pts',(-9.42743337163542,18.5219808928548,1.69768315121407E-11));
#24532=CARTESIAN_POINT('Ctrl Pts',(-7.07057502871922,18.6969808928548,4.08219839617346));
#24533=CARTESIAN_POINT('Ctrl Pts',(-4.71371668580301,18.8719808928548,8.16439679232994));
#24534=CARTESIAN_POINT('Ctrl Pts',(1.47018674401621E-11,19.0469808928548,
8.16439679232146));
#24535=CARTESIAN_POINT('Ctrl Pts',(4.71371668583241,19.2219808928548,8.16439679231297));
#24536=CARTESIAN_POINT('Ctrl Pts',(7.07057502873392,19.3969808928548,4.082198396148));
#24537=CARTESIAN_POINT('Ctrl Pts',(9.42743337163542,19.5719808928548,-1.69756769845304E-11));
#24538=CARTESIAN_POINT('Ctrl Pts',(7.07057502871922,19.7469808928548,-4.08219839617346));
#24539=CARTESIAN_POINT('Ctrl Pts',(4.71371668580301,19.9219808928548,-8.16439679232994));
#24540=CARTESIAN_POINT('Ctrl Pts',(-1.4702867290402E-11,20.0969808928548,
-8.16439679232146));
#24541=CARTESIAN_POINT('Ctrl Pts',(-4.71371668583241,20.2719808928548,-8.16439679231297));
#24542=CARTESIAN_POINT('Ctrl Pts',(-7.07057502873392,20.4469808928548,-4.082198396148));
#24543=CARTESIAN_POINT('Ctrl Pts',(-9.42743337163542,20.6219808928548,1.69768315121407E-11));
#24544=CARTESIAN_POINT('Ctrl Pts',(-7.07057502871922,20.7969808928548,4.08219839617346));
#24545=CARTESIAN_POINT('Ctrl Pts',(-4.71371668580301,20.9719808928548,8.16439679232994));
#24546=CARTESIAN_POINT('Ctrl Pts',(1.47018674401621E-11,21.1469808928548,
8.16439679232146));
#24547=CARTESIAN_POINT('Ctrl Pts',(4.71371668583241,21.3219808928548,8.16439679231297));
#24548=CARTESIAN_POINT('Ctrl Pts',(7.07057502873392,21.4969808928548,4.082198396148));
#24549=CARTESIAN_POINT('Ctrl Pts',(9.42743337163542,21.6719808928548,-1.69756769845304E-11));
#24550=CARTESIAN_POINT('Ctrl Pts',(7.07057502871922,21.8469808928548,-4.08219839617346));
#24551=CARTESIAN_POINT('Ctrl Pts',(4.71371668580301,22.0219808928548,-8.16439679232994));
#24552=CARTESIAN_POINT('Ctrl Pts',(-1.4702867290402E-11,22.1969808928548,
-8.16439679232146));
#24553=CARTESIAN_POINT('Ctrl Pts',(-4.71371668583241,22.3719808928548,-8.16439679231297));
#24554=CARTESIAN_POINT('Ctrl Pts',(-7.07057502873392,22.5469808928548,-4.082198396148));
#24555=CARTESIAN_POINT('Ctrl Pts',(-9.42743337163542,22.7219808928548,1.69768315121407E-11));
#24556=CARTESIAN_POINT('Ctrl Pts',(-7.07057502871922,22.8969808928548,4.08219839617346));
#24557=CARTESIAN_POINT('Ctrl Pts',(-4.71371668580301,23.0719808928548,8.16439679232994));
#24558=CARTESIAN_POINT('Ctrl Pts',(1.47018674401621E-11,23.2469808928548,
8.16439679232146));
#24559=CARTESIAN_POINT('Ctrl Pts',(4.71371668583241,23.4219808928548,8.16439679231297));
#24560=CARTESIAN_POINT('Ctrl Pts',(7.07057502873392,23.5969808928548,4.082198396148));
#24561=CARTESIAN_POINT('Ctrl Pts',(9.42743337163542,23.7719808928548,-1.69756769845304E-11));
#24562=CARTESIAN_POINT('Ctrl Pts',(7.07057502871922,23.9469808928548,-4.08219839617346));
#24563=CARTESIAN_POINT('Ctrl Pts',(4.71371668580301,24.1219808928548,-8.16439679232994));
#24564=CARTESIAN_POINT('Ctrl Pts',(-1.4702867290402E-11,24.2969808928548,
-8.16439679232146));
#24565=CARTESIAN_POINT('Ctrl Pts',(-4.71371668583241,24.4719808928548,-8.16439679231297));
#24566=CARTESIAN_POINT('Ctrl Pts',(-7.07057502873392,24.6469808928548,-4.082198396148));
#24567=CARTESIAN_POINT('Ctrl Pts',(-9.42743337163542,24.8219808928548,1.69768315121407E-11));
#24568=CARTESIAN_POINT('Ctrl Pts',(-7.07057502871922,24.9969808928548,4.08219839617346));
#24569=CARTESIAN_POINT('Ctrl Pts',(-4.71371668580301,25.1719808928548,8.16439679232994));
#24570=CARTESIAN_POINT('Ctrl Pts',(1.47018674401621E-11,25.3469808928548,
8.16439679232146));
#24571=CARTESIAN_POINT('Ctrl Pts',(4.71371668583241,25.5219808928548,8.16439679231297));
#24572=CARTESIAN_POINT('Ctrl Pts',(7.07057502873392,25.6969808928548,4.082198396148));
#24573=CARTESIAN_POINT('Ctrl Pts',(9.42743337163542,25.8719808928548,-1.69756769845304E-11));
#24574=CARTESIAN_POINT('Ctrl Pts',(7.07057502871922,26.0469808928548,-4.08219839617346));
#24575=CARTESIAN_POINT('Ctrl Pts',(4.71371668580301,26.2219808928548,-8.16439679232994));
#24576=CARTESIAN_POINT('Ctrl Pts',(-1.4702867290402E-11,26.3969808928548,
-8.16439679232146));
#24577=CARTESIAN_POINT('Ctrl Pts',(-1.51301075899711E-11,-143.579517970998,
-8.40164026751963));
#24578=CARTESIAN_POINT('Ctrl Pts',(-4.85068927010199,-143.404517970998,
-8.4016402675109));
#24579=CARTESIAN_POINT('Ctrl Pts',(-7.27603390513785,-143.229517970998,
-4.20082013374671));
#24580=CARTESIAN_POINT('Ctrl Pts',(-9.70137854017372,-143.054517970998,
1.74701493417668E-11));
#24581=CARTESIAN_POINT('Ctrl Pts',(-7.27603390512272,-142.879517970998,
4.20082013377292));
#24582=CARTESIAN_POINT('Ctrl Pts',(-4.85068927007173,-142.704517970998,
8.40164026752836));
#24583=CARTESIAN_POINT('Ctrl Pts',(1.5129078685785E-11,-142.529517970998,
8.40164026751963));
#24584=CARTESIAN_POINT('Ctrl Pts',(4.85068927010198,-142.354517970998,8.4016402675109));
#24585=CARTESIAN_POINT('Ctrl Pts',(7.27603390513785,-142.179517970998,4.20082013374672));
#24586=CARTESIAN_POINT('Ctrl Pts',(9.70137854017372,-142.004517970998,-1.74689612655491E-11));
#24587=CARTESIAN_POINT('Ctrl Pts',(7.27603390512273,-141.829517970998,-4.20082013377291));
#24588=CARTESIAN_POINT('Ctrl Pts',(4.85068927007173,-141.654517970998,-8.40164026752836));
#24589=CARTESIAN_POINT('Ctrl Pts',(-1.51301075899711E-11,-141.479517970998,
-8.40164026751963));
#24590=CARTESIAN_POINT('Ctrl Pts',(-4.85068927010199,-141.304517970998,
-8.4016402675109));
#24591=CARTESIAN_POINT('Ctrl Pts',(-7.27603390513785,-141.129517970998,
-4.20082013374671));
#24592=CARTESIAN_POINT('Ctrl Pts',(-9.70137854017372,-140.954517970998,
1.74701493417668E-11));
#24593=CARTESIAN_POINT('Ctrl Pts',(-7.27603390512272,-140.779517970998,
4.20082013377292));
#24594=CARTESIAN_POINT('Ctrl Pts',(-4.85068927007173,-140.604517970998,
8.40164026752836));
#24595=CARTESIAN_POINT('Ctrl Pts',(1.5129078685785E-11,-140.429517970998,
8.40164026751963));
#24596=CARTESIAN_POINT('Ctrl Pts',(4.85068927010198,-140.254517970998,8.4016402675109));
#24597=CARTESIAN_POINT('Ctrl Pts',(7.27603390513785,-140.079517970998,4.20082013374672));
#24598=CARTESIAN_POINT('Ctrl Pts',(9.70137854017372,-139.904517970998,-1.74689612655491E-11));
#24599=CARTESIAN_POINT('Ctrl Pts',(7.27603390512273,-139.729517970998,-4.20082013377291));
#24600=CARTESIAN_POINT('Ctrl Pts',(4.85068927007173,-139.554517970998,-8.40164026752836));
#24601=CARTESIAN_POINT('Ctrl Pts',(-1.51301075899711E-11,-139.379517970998,
-8.40164026751963));
#24602=CARTESIAN_POINT('Ctrl Pts',(-4.85068927010199,-139.204517970998,
-8.4016402675109));
#24603=CARTESIAN_POINT('Ctrl Pts',(-7.27603390513785,-139.029517970998,
-4.20082013374671));
#24604=CARTESIAN_POINT('Ctrl Pts',(-9.70137854017372,-138.854517970998,
1.74701493417668E-11));
#24605=CARTESIAN_POINT('Ctrl Pts',(-7.27603390512272,-138.679517970998,
4.20082013377292));
#24606=CARTESIAN_POINT('Ctrl Pts',(-4.85068927007173,-138.504517970998,
8.40164026752836));
#24607=CARTESIAN_POINT('Ctrl Pts',(1.5129078685785E-11,-138.329517970998,
8.40164026751963));
#24608=CARTESIAN_POINT('Ctrl Pts',(4.85068927010198,-138.154517970998,8.4016402675109));
#24609=CARTESIAN_POINT('Ctrl Pts',(7.27603390513785,-137.979517970998,4.20082013374672));
#24610=CARTESIAN_POINT('Ctrl Pts',(9.70137854017372,-137.804517970998,-1.74689612655491E-11));
#24611=CARTESIAN_POINT('Ctrl Pts',(7.27603390512273,-137.629517970998,-4.20082013377291));
#24612=CARTESIAN_POINT('Ctrl Pts',(4.85068927007173,-137.454517970998,-8.40164026752836));
#24613=CARTESIAN_POINT('Ctrl Pts',(-1.51301075899711E-11,-137.279517970998,
-8.40164026751963));
#24614=CARTESIAN_POINT('Ctrl Pts',(-4.85068927010199,-137.104517970998,
-8.4016402675109));
#24615=CARTESIAN_POINT('Ctrl Pts',(-7.27603390513785,-136.929517970998,
-4.20082013374671));
#24616=CARTESIAN_POINT('Ctrl Pts',(-9.70137854017372,-136.754517970998,
1.74701493417668E-11));
#24617=CARTESIAN_POINT('Ctrl Pts',(-7.27603390512272,-136.579517970998,
4.20082013377292));
#24618=CARTESIAN_POINT('Ctrl Pts',(-4.85068927007173,-136.404517970998,
8.40164026752836));
#24619=CARTESIAN_POINT('Ctrl Pts',(1.5129078685785E-11,-136.229517970998,
8.40164026751963));
#24620=CARTESIAN_POINT('Ctrl Pts',(4.85068927010198,-136.054517970998,8.4016402675109));
#24621=CARTESIAN_POINT('Ctrl Pts',(7.27603390513785,-135.879517970998,4.20082013374672));
#24622=CARTESIAN_POINT('Ctrl Pts',(9.70137854017372,-135.704517970998,-1.74689612655491E-11));
#24623=CARTESIAN_POINT('Ctrl Pts',(7.27603390512273,-135.529517970998,-4.20082013377291));
#24624=CARTESIAN_POINT('Ctrl Pts',(4.85068927007173,-135.354517970998,-8.40164026752836));
#24625=CARTESIAN_POINT('Ctrl Pts',(-1.51301075899711E-11,-135.179517970998,
-8.40164026751963));
#24626=CARTESIAN_POINT('Ctrl Pts',(-4.85068927010199,-135.004517970998,
-8.4016402675109));
#24627=CARTESIAN_POINT('Ctrl Pts',(-7.27603390513785,-134.829517970998,
-4.20082013374671));
#24628=CARTESIAN_POINT('Ctrl Pts',(-9.70137854017372,-134.654517970998,
1.74701493417668E-11));
#24629=CARTESIAN_POINT('Ctrl Pts',(-7.27603390512272,-134.479517970998,
4.20082013377292));
#24630=CARTESIAN_POINT('Ctrl Pts',(-4.85068927007173,-134.304517970998,
8.40164026752836));
#24631=CARTESIAN_POINT('Ctrl Pts',(1.5129078685785E-11,-134.129517970998,
8.40164026751963));
#24632=CARTESIAN_POINT('Ctrl Pts',(4.85068927010198,-133.954517970998,8.4016402675109));
#24633=CARTESIAN_POINT('Ctrl Pts',(7.27603390513785,-133.779517970998,4.20082013374672));
#24634=CARTESIAN_POINT('Ctrl Pts',(9.70137854017372,-133.604517970998,-1.74689612655491E-11));
#24635=CARTESIAN_POINT('Ctrl Pts',(7.27603390512273,-133.429517970998,-4.20082013377291));
#24636=CARTESIAN_POINT('Ctrl Pts',(4.85068927007173,-133.254517970998,-8.40164026752836));
#24637=CARTESIAN_POINT('Ctrl Pts',(-1.51301075899711E-11,-133.079517970998,
-8.40164026751963));
#24638=CARTESIAN_POINT('Ctrl Pts',(-4.85068927010199,-132.904517970998,
-8.4016402675109));
#24639=CARTESIAN_POINT('Ctrl Pts',(-7.27603390513785,-132.729517970998,
-4.20082013374671));
#24640=CARTESIAN_POINT('Ctrl Pts',(-9.70137854017372,-132.554517970998,
1.74701493417668E-11));
#24641=CARTESIAN_POINT('Ctrl Pts',(-7.27603390512272,-132.379517970998,
4.20082013377292));
#24642=CARTESIAN_POINT('Ctrl Pts',(-4.85068927007173,-132.204517970998,
8.40164026752836));
#24643=CARTESIAN_POINT('Ctrl Pts',(1.5129078685785E-11,-132.029517970998,
8.40164026751963));
#24644=CARTESIAN_POINT('Ctrl Pts',(4.85068927010198,-131.854517970998,8.4016402675109));
#24645=CARTESIAN_POINT('Ctrl Pts',(7.27603390513785,-131.679517970998,4.20082013374672));
#24646=CARTESIAN_POINT('Ctrl Pts',(9.70137854017372,-131.504517970998,-1.74689612655491E-11));
#24647=CARTESIAN_POINT('Ctrl Pts',(7.27603390512273,-131.329517970998,-4.20082013377291));
#24648=CARTESIAN_POINT('Ctrl Pts',(4.85068927007173,-131.154517970998,-8.40164026752836));
#24649=CARTESIAN_POINT('Ctrl Pts',(-1.51301075899711E-11,-130.979517970998,
-8.40164026751963));
#24650=CARTESIAN_POINT('Ctrl Pts',(-4.85068927010199,-130.804517970998,
-8.4016402675109));
#24651=CARTESIAN_POINT('Ctrl Pts',(-7.27603390513785,-130.629517970998,
-4.20082013374671));
#24652=CARTESIAN_POINT('Ctrl Pts',(-9.70137854017372,-130.454517970998,
1.74701493417668E-11));
#24653=CARTESIAN_POINT('Ctrl Pts',(-7.27603390512272,-130.279517970998,
4.20082013377292));
#24654=CARTESIAN_POINT('Ctrl Pts',(-4.85068927007173,-130.104517970998,
8.40164026752836));
#24655=CARTESIAN_POINT('Ctrl Pts',(1.5129078685785E-11,-129.929517970998,
8.40164026751963));
#24656=CARTESIAN_POINT('Ctrl Pts',(4.85068927010198,-129.754517970998,8.4016402675109));
#24657=CARTESIAN_POINT('Ctrl Pts',(7.27603390513785,-129.579517970998,4.20082013374672));
#24658=CARTESIAN_POINT('Ctrl Pts',(9.70137854017372,-129.404517970998,-1.74689612655491E-11));
#24659=CARTESIAN_POINT('Ctrl Pts',(7.27603390512273,-129.229517970998,-4.20082013377291));
#24660=CARTESIAN_POINT('Ctrl Pts',(4.85068927007173,-129.054517970998,-8.40164026752836));
#24661=CARTESIAN_POINT('Ctrl Pts',(-1.51301075899711E-11,-128.879517970998,
-8.40164026751963));
#24662=CARTESIAN_POINT('Ctrl Pts',(-4.85068927010199,-128.704517970998,
-8.4016402675109));
#24663=CARTESIAN_POINT('Ctrl Pts',(-7.27603390513785,-128.529517970998,
-4.20082013374671));
#24664=CARTESIAN_POINT('Ctrl Pts',(-9.70137854017372,-128.354517970998,
1.74701493417668E-11));
#24665=CARTESIAN_POINT('Ctrl Pts',(-7.27603390512272,-128.179517970998,
4.20082013377292));
#24666=CARTESIAN_POINT('Ctrl Pts',(-4.85068927007173,-128.004517970998,
8.40164026752836));
#24667=CARTESIAN_POINT('Ctrl Pts',(1.5129078685785E-11,-127.829517970998,
8.40164026751963));
#24668=CARTESIAN_POINT('Ctrl Pts',(4.85068927010198,-127.654517970998,8.4016402675109));
#24669=CARTESIAN_POINT('Ctrl Pts',(7.27603390513785,-127.479517970998,4.20082013374672));
#24670=CARTESIAN_POINT('Ctrl Pts',(9.70137854017372,-127.304517970998,-1.74689612655491E-11));
#24671=CARTESIAN_POINT('Ctrl Pts',(7.27603390512273,-127.129517970998,-4.20082013377291));
#24672=CARTESIAN_POINT('Ctrl Pts',(4.85068927007173,-126.954517970998,-8.40164026752836));
#24673=CARTESIAN_POINT('Ctrl Pts',(-1.51301075899711E-11,-126.779517970998,
-8.40164026751963));
#24674=CARTESIAN_POINT('Ctrl Pts',(-4.85068927010199,-126.604517970998,
-8.4016402675109));
#24675=CARTESIAN_POINT('Ctrl Pts',(-7.27603390513785,-126.429517970998,
-4.20082013374671));
#24676=CARTESIAN_POINT('Ctrl Pts',(-9.70137854017372,-126.254517970998,
1.74701493417668E-11));
#24677=CARTESIAN_POINT('Ctrl Pts',(-7.27603390512272,-126.079517970998,
4.20082013377292));
#24678=CARTESIAN_POINT('Ctrl Pts',(-4.85068927007173,-125.904517970998,
8.40164026752836));
#24679=CARTESIAN_POINT('Ctrl Pts',(1.5129078685785E-11,-125.729517970998,
8.40164026751963));
#24680=CARTESIAN_POINT('Ctrl Pts',(4.85068927010198,-125.554517970998,8.4016402675109));
#24681=CARTESIAN_POINT('Ctrl Pts',(7.27603390513785,-125.379517970998,4.20082013374672));
#24682=CARTESIAN_POINT('Ctrl Pts',(9.70137854017372,-125.204517970998,-1.74689612655491E-11));
#24683=CARTESIAN_POINT('Ctrl Pts',(7.27603390512273,-125.029517970998,-4.20082013377291));
#24684=CARTESIAN_POINT('Ctrl Pts',(4.85068927007173,-124.854517970998,-8.40164026752836));
#24685=CARTESIAN_POINT('Ctrl Pts',(-1.51301075899711E-11,-124.679517970998,
-8.40164026751963));
#24686=CARTESIAN_POINT('Ctrl Pts',(-4.85068927010199,-124.504517970998,
-8.4016402675109));
#24687=CARTESIAN_POINT('Ctrl Pts',(-7.27603390513785,-124.329517970998,
-4.20082013374671));
#24688=CARTESIAN_POINT('Ctrl Pts',(-9.70137854017372,-124.154517970998,
1.74701493417668E-11));
#24689=CARTESIAN_POINT('Ctrl Pts',(-7.27603390512272,-123.979517970998,
4.20082013377292));
#24690=CARTESIAN_POINT('Ctrl Pts',(-4.85068927007173,-123.804517970998,
8.40164026752836));
#24691=CARTESIAN_POINT('Ctrl Pts',(1.5129078685785E-11,-123.629517970998,
8.40164026751963));
#24692=CARTESIAN_POINT('Ctrl Pts',(4.85068927010198,-123.454517970998,8.4016402675109));
#24693=CARTESIAN_POINT('Ctrl Pts',(7.27603390513785,-123.279517970998,4.20082013374672));
#24694=CARTESIAN_POINT('Ctrl Pts',(9.70137854017372,-123.104517970998,-1.74689612655491E-11));
#24695=CARTESIAN_POINT('Ctrl Pts',(7.27603390512273,-122.929517970998,-4.20082013377291));
#24696=CARTESIAN_POINT('Ctrl Pts',(4.85068927007173,-122.754517970998,-8.40164026752836));
#24697=CARTESIAN_POINT('Ctrl Pts',(-1.51301075899711E-11,-122.579517970998,
-8.40164026751963));
#24698=CARTESIAN_POINT('Ctrl Pts',(-4.85068927010199,-122.404517970998,
-8.4016402675109));
#24699=CARTESIAN_POINT('Ctrl Pts',(-7.27603390513785,-122.229517970998,
-4.20082013374671));
#24700=CARTESIAN_POINT('Ctrl Pts',(-9.70137854017372,-122.054517970998,
1.74701493417668E-11));
#24701=CARTESIAN_POINT('Ctrl Pts',(-7.27603390512272,-121.879517970998,
4.20082013377292));
#24702=CARTESIAN_POINT('Ctrl Pts',(-4.85068927007173,-121.704517970998,
8.40164026752836));
#24703=CARTESIAN_POINT('Ctrl Pts',(1.5129078685785E-11,-121.529517970998,
8.40164026751963));
#24704=CARTESIAN_POINT('Ctrl Pts',(4.85068927010198,-121.354517970998,8.4016402675109));
#24705=CARTESIAN_POINT('Ctrl Pts',(7.27603390513785,-121.179517970998,4.20082013374672));
#24706=CARTESIAN_POINT('Ctrl Pts',(9.70137854017372,-121.004517970998,-1.74689612655491E-11));
#24707=CARTESIAN_POINT('Ctrl Pts',(7.27603390512273,-120.829517970998,-4.20082013377291));
#24708=CARTESIAN_POINT('Ctrl Pts',(4.85068927007173,-120.654517970998,-8.40164026752836));
#24709=CARTESIAN_POINT('Ctrl Pts',(-1.51301075899711E-11,-120.479517970998,
-8.40164026751963));
#24710=CARTESIAN_POINT('Ctrl Pts',(-4.85068927010199,-120.304517970998,
-8.4016402675109));
#24711=CARTESIAN_POINT('Ctrl Pts',(-7.27603390513785,-120.129517970998,
-4.20082013374671));
#24712=CARTESIAN_POINT('Ctrl Pts',(-9.70137854017372,-119.954517970998,
1.74701493417668E-11));
#24713=CARTESIAN_POINT('Ctrl Pts',(-7.27603390512272,-119.779517970998,
4.20082013377292));
#24714=CARTESIAN_POINT('Ctrl Pts',(-4.85068927007173,-119.604517970998,
8.40164026752836));
#24715=CARTESIAN_POINT('Ctrl Pts',(1.5129078685785E-11,-119.429517970998,
8.40164026751963));
#24716=CARTESIAN_POINT('Ctrl Pts',(4.85068927010198,-119.254517970998,8.4016402675109));
#24717=CARTESIAN_POINT('Ctrl Pts',(7.27603390513785,-119.079517970998,4.20082013374672));
#24718=CARTESIAN_POINT('Ctrl Pts',(9.70137854017372,-118.904517970998,-1.74689612655491E-11));
#24719=CARTESIAN_POINT('Ctrl Pts',(7.27603390512273,-118.729517970998,-4.20082013377291));
#24720=CARTESIAN_POINT('Ctrl Pts',(4.85068927007173,-118.554517970998,-8.40164026752836));
#24721=CARTESIAN_POINT('Ctrl Pts',(-1.51301075899711E-11,-118.379517970998,
-8.40164026751963));
#24722=CARTESIAN_POINT('Ctrl Pts',(-4.85068927010199,-118.204517970998,
-8.4016402675109));
#24723=CARTESIAN_POINT('Ctrl Pts',(-7.27603390513785,-118.029517970998,
-4.20082013374671));
#24724=CARTESIAN_POINT('Ctrl Pts',(-9.70137854017372,-117.854517970998,
1.74701493417668E-11));
#24725=CARTESIAN_POINT('Ctrl Pts',(-7.27603390512272,-117.679517970998,
4.20082013377292));
#24726=CARTESIAN_POINT('Ctrl Pts',(-4.85068927007173,-117.504517970998,
8.40164026752836));
#24727=CARTESIAN_POINT('Ctrl Pts',(1.5129078685785E-11,-117.329517970998,
8.40164026751963));
#24728=CARTESIAN_POINT('Ctrl Pts',(4.85068927010198,-117.154517970998,8.4016402675109));
#24729=CARTESIAN_POINT('Ctrl Pts',(7.27603390513785,-116.979517970998,4.20082013374672));
#24730=CARTESIAN_POINT('Ctrl Pts',(9.70137854017372,-116.804517970998,-1.74689612655491E-11));
#24731=CARTESIAN_POINT('Ctrl Pts',(7.27603390512273,-116.629517970998,-4.20082013377291));
#24732=CARTESIAN_POINT('Ctrl Pts',(4.85068927007173,-116.454517970998,-8.40164026752836));
#24733=CARTESIAN_POINT('Ctrl Pts',(-1.51301075899711E-11,-116.279517970998,
-8.40164026751963));
#24734=CARTESIAN_POINT('Ctrl Pts',(-4.85068927010199,-116.104517970998,
-8.4016402675109));
#24735=CARTESIAN_POINT('Ctrl Pts',(-7.27603390513785,-115.929517970998,
-4.20082013374671));
#24736=CARTESIAN_POINT('Ctrl Pts',(-9.70137854017372,-115.754517970998,
1.74701493417668E-11));
#24737=CARTESIAN_POINT('Ctrl Pts',(-7.27603390512272,-115.579517970998,
4.20082013377292));
#24738=CARTESIAN_POINT('Ctrl Pts',(-4.85068927007173,-115.404517970998,
8.40164026752836));
#24739=CARTESIAN_POINT('Ctrl Pts',(1.5129078685785E-11,-115.229517970998,
8.40164026751963));
#24740=CARTESIAN_POINT('Ctrl Pts',(4.85068927010198,-115.054517970998,8.4016402675109));
#24741=CARTESIAN_POINT('Ctrl Pts',(7.27603390513785,-114.879517970998,4.20082013374672));
#24742=CARTESIAN_POINT('Ctrl Pts',(9.70137854017372,-114.704517970998,-1.74689612655491E-11));
#24743=CARTESIAN_POINT('Ctrl Pts',(7.27603390512273,-114.529517970998,-4.20082013377291));
#24744=CARTESIAN_POINT('Ctrl Pts',(4.85068927007173,-114.354517970998,-8.40164026752836));
#24745=CARTESIAN_POINT('Ctrl Pts',(-1.51301075899711E-11,-114.179517970998,
-8.40164026751963));
#24746=CARTESIAN_POINT('Ctrl Pts',(-4.85068927010199,-114.004517970998,
-8.4016402675109));
#24747=CARTESIAN_POINT('Ctrl Pts',(-7.27603390513785,-113.829517970998,
-4.20082013374671));
#24748=CARTESIAN_POINT('Ctrl Pts',(-9.70137854017372,-113.654517970998,
1.74701493417668E-11));
#24749=CARTESIAN_POINT('Ctrl Pts',(-7.27603390512272,-113.479517970998,
4.20082013377292));
#24750=CARTESIAN_POINT('Ctrl Pts',(-4.85068927007173,-113.304517970998,
8.40164026752836));
#24751=CARTESIAN_POINT('Ctrl Pts',(1.5129078685785E-11,-113.129517970998,
8.40164026751963));
#24752=CARTESIAN_POINT('Ctrl Pts',(4.85068927010198,-112.954517970998,8.4016402675109));
#24753=CARTESIAN_POINT('Ctrl Pts',(7.27603390513785,-112.779517970998,4.20082013374672));
#24754=CARTESIAN_POINT('Ctrl Pts',(9.70137854017372,-112.604517970998,-1.74689612655491E-11));
#24755=CARTESIAN_POINT('Ctrl Pts',(7.27603390512273,-112.429517970998,-4.20082013377291));
#24756=CARTESIAN_POINT('Ctrl Pts',(4.85068927007173,-112.254517970998,-8.40164026752836));
#24757=CARTESIAN_POINT('Ctrl Pts',(-1.51301075899711E-11,-112.079517970998,
-8.40164026751963));
#24758=CARTESIAN_POINT('Ctrl Pts',(-4.85068927010199,-111.904517970998,
-8.4016402675109));
#24759=CARTESIAN_POINT('Ctrl Pts',(-7.27603390513785,-111.729517970998,
-4.20082013374671));
#24760=CARTESIAN_POINT('Ctrl Pts',(-9.70137854017372,-111.554517970998,
1.74701493417668E-11));
#24761=CARTESIAN_POINT('Ctrl Pts',(-7.27603390512272,-111.379517970998,
4.20082013377292));
#24762=CARTESIAN_POINT('Ctrl Pts',(-4.85068927007173,-111.204517970998,
8.40164026752836));
#24763=CARTESIAN_POINT('Ctrl Pts',(1.5129078685785E-11,-111.029517970998,
8.40164026751963));
#24764=CARTESIAN_POINT('Ctrl Pts',(4.85068927010198,-110.854517970998,8.4016402675109));
#24765=CARTESIAN_POINT('Ctrl Pts',(7.27603390513785,-110.679517970998,4.20082013374672));
#24766=CARTESIAN_POINT('Ctrl Pts',(9.70137854017372,-110.504517970998,-1.74689612655491E-11));
#24767=CARTESIAN_POINT('Ctrl Pts',(7.27603390512273,-110.329517970998,-4.20082013377291));
#24768=CARTESIAN_POINT('Ctrl Pts',(4.85068927007173,-110.154517970998,-8.40164026752836));
#24769=CARTESIAN_POINT('Ctrl Pts',(-1.51301075899711E-11,-109.979517970998,
-8.40164026751963));
#24770=CARTESIAN_POINT('Ctrl Pts',(-4.85068927010199,-109.804517970998,
-8.4016402675109));
#24771=CARTESIAN_POINT('Ctrl Pts',(-7.27603390513785,-109.629517970998,
-4.20082013374671));
#24772=CARTESIAN_POINT('Ctrl Pts',(-9.70137854017372,-109.454517970998,
1.74701493417668E-11));
#24773=CARTESIAN_POINT('Ctrl Pts',(-7.27603390512272,-109.279517970998,
4.20082013377292));
#24774=CARTESIAN_POINT('Ctrl Pts',(-4.85068927007173,-109.104517970998,
8.40164026752836));
#24775=CARTESIAN_POINT('Ctrl Pts',(1.5129078685785E-11,-108.929517970998,
8.40164026751963));
#24776=CARTESIAN_POINT('Ctrl Pts',(4.85068927010198,-108.754517970998,8.4016402675109));
#24777=CARTESIAN_POINT('Ctrl Pts',(7.27603390513785,-108.579517970998,4.20082013374672));
#24778=CARTESIAN_POINT('Ctrl Pts',(9.70137854017372,-108.404517970998,-1.74689612655491E-11));
#24779=CARTESIAN_POINT('Ctrl Pts',(7.27603390512273,-108.229517970998,-4.20082013377291));
#24780=CARTESIAN_POINT('Ctrl Pts',(4.85068927007173,-108.054517970998,-8.40164026752836));
#24781=CARTESIAN_POINT('Ctrl Pts',(-1.51301075899711E-11,-107.879517970998,
-8.40164026751963));
#24782=CARTESIAN_POINT('Ctrl Pts',(-4.85068927010199,-107.704517970998,
-8.4016402675109));
#24783=CARTESIAN_POINT('Ctrl Pts',(-7.27603390513785,-107.529517970998,
-4.20082013374671));
#24784=CARTESIAN_POINT('Ctrl Pts',(-9.70137854017372,-107.354517970998,
1.74701493417668E-11));
#24785=CARTESIAN_POINT('Ctrl Pts',(-7.27603390512272,-107.179517970998,
4.20082013377292));
#24786=CARTESIAN_POINT('Ctrl Pts',(-4.85068927007173,-107.004517970998,
8.40164026752836));
#24787=CARTESIAN_POINT('Ctrl Pts',(1.5129078685785E-11,-106.829517970998,
8.40164026751963));
#24788=CARTESIAN_POINT('Ctrl Pts',(4.85068927010198,-106.654517970998,8.4016402675109));
#24789=CARTESIAN_POINT('Ctrl Pts',(7.27603390513785,-106.479517970998,4.20082013374672));
#24790=CARTESIAN_POINT('Ctrl Pts',(9.70137854017372,-106.304517970998,-1.74689612655491E-11));
#24791=CARTESIAN_POINT('Ctrl Pts',(7.27603390512273,-106.129517970998,-4.20082013377291));
#24792=CARTESIAN_POINT('Ctrl Pts',(4.85068927007173,-105.954517970998,-8.40164026752836));
#24793=CARTESIAN_POINT('Ctrl Pts',(-1.51301075899711E-11,-105.779517970998,
-8.40164026751963));
#24794=CARTESIAN_POINT('Ctrl Pts',(-4.85068927010199,-105.604517970998,
-8.4016402675109));
#24795=CARTESIAN_POINT('Ctrl Pts',(-7.27603390513785,-105.429517970998,
-4.20082013374671));
#24796=CARTESIAN_POINT('Ctrl Pts',(-9.70137854017372,-105.254517970998,
1.74701493417668E-11));
#24797=CARTESIAN_POINT('Ctrl Pts',(-7.27603390512272,-105.079517970998,
4.20082013377292));
#24798=CARTESIAN_POINT('Ctrl Pts',(-4.85068927007173,-104.904517970998,
8.40164026752836));
#24799=CARTESIAN_POINT('Ctrl Pts',(1.5129078685785E-11,-104.729517970998,
8.40164026751963));
#24800=CARTESIAN_POINT('Ctrl Pts',(4.85068927010198,-104.554517970998,8.4016402675109));
#24801=CARTESIAN_POINT('Ctrl Pts',(7.27603390513785,-104.379517970998,4.20082013374672));
#24802=CARTESIAN_POINT('Ctrl Pts',(9.70137854017372,-104.204517970998,-1.74689612655491E-11));
#24803=CARTESIAN_POINT('Ctrl Pts',(7.27603390512273,-104.029517970998,-4.20082013377291));
#24804=CARTESIAN_POINT('Ctrl Pts',(4.85068927007173,-103.854517970998,-8.40164026752836));
#24805=CARTESIAN_POINT('Ctrl Pts',(-1.51301075899711E-11,-103.679517970998,
-8.40164026751963));
#24806=CARTESIAN_POINT('Ctrl Pts',(-4.85068927010199,-103.504517970998,
-8.4016402675109));
#24807=CARTESIAN_POINT('Ctrl Pts',(-7.27603390513785,-103.329517970998,
-4.20082013374671));
#24808=CARTESIAN_POINT('Ctrl Pts',(-9.70137854017372,-103.154517970998,
1.74701493417668E-11));
#24809=CARTESIAN_POINT('Ctrl Pts',(-7.27603390512272,-102.979517970998,
4.20082013377292));
#24810=CARTESIAN_POINT('Ctrl Pts',(-4.85068927007173,-102.804517970998,
8.40164026752836));
#24811=CARTESIAN_POINT('Ctrl Pts',(1.5129078685785E-11,-102.629517970998,
8.40164026751963));
#24812=CARTESIAN_POINT('Ctrl Pts',(4.85068927010198,-102.454517970998,8.4016402675109));
#24813=CARTESIAN_POINT('Ctrl Pts',(7.27603390513785,-102.279517970998,4.20082013374672));
#24814=CARTESIAN_POINT('Ctrl Pts',(9.70137854017372,-102.104517970998,-1.74689612655491E-11));
#24815=CARTESIAN_POINT('Ctrl Pts',(7.27603390512273,-101.929517970998,-4.20082013377291));
#24816=CARTESIAN_POINT('Ctrl Pts',(4.85068927007173,-101.754517970998,-8.40164026752836));
#24817=CARTESIAN_POINT('Ctrl Pts',(-1.51301075899711E-11,-101.579517970998,
-8.40164026751963));
#24818=CARTESIAN_POINT('Ctrl Pts',(-4.85068927010199,-101.404517970998,
-8.4016402675109));
#24819=CARTESIAN_POINT('Ctrl Pts',(-7.27603390513785,-101.229517970998,
-4.20082013374671));
#24820=CARTESIAN_POINT('Ctrl Pts',(-9.70137854017372,-101.054517970998,
1.74701493417668E-11));
#24821=CARTESIAN_POINT('Ctrl Pts',(-7.27603390512272,-100.879517970998,
4.20082013377292));
#24822=CARTESIAN_POINT('Ctrl Pts',(-4.85068927007173,-100.704517970998,
8.40164026752836));
#24823=CARTESIAN_POINT('Ctrl Pts',(1.5129078685785E-11,-100.529517970998,
8.40164026751963));
#24824=CARTESIAN_POINT('Ctrl Pts',(4.85068927010198,-100.354517970998,8.4016402675109));
#24825=CARTESIAN_POINT('Ctrl Pts',(7.27603390513785,-100.179517970998,4.20082013374672));
#24826=CARTESIAN_POINT('Ctrl Pts',(9.70137854017372,-100.004517970998,-1.74689612655491E-11));
#24827=CARTESIAN_POINT('Ctrl Pts',(7.27603390512273,-99.8295179709984,-4.20082013377291));
#24828=CARTESIAN_POINT('Ctrl Pts',(4.85068927007173,-99.6545179709984,-8.40164026752836));
#24829=CARTESIAN_POINT('Ctrl Pts',(-1.51301075899711E-11,-99.4795179709984,
-8.40164026751963));
#24830=CARTESIAN_POINT('Ctrl Pts',(-4.85068927010199,-99.3045179709984,
-8.4016402675109));
#24831=CARTESIAN_POINT('Ctrl Pts',(-7.27603390513785,-99.1295179709984,
-4.20082013374671));
#24832=CARTESIAN_POINT('Ctrl Pts',(-9.70137854017372,-98.9545179709984,
1.74701493417668E-11));
#24833=CARTESIAN_POINT('Ctrl Pts',(-7.27603390512272,-98.7795179709984,
4.20082013377292));
#24834=CARTESIAN_POINT('Ctrl Pts',(-4.85068927007173,-98.6045179709984,
8.40164026752836));
#24835=CARTESIAN_POINT('Ctrl Pts',(1.5129078685785E-11,-98.4295179709984,
8.40164026751963));
#24836=CARTESIAN_POINT('Ctrl Pts',(4.85068927010198,-98.2545179709984,8.4016402675109));
#24837=CARTESIAN_POINT('Ctrl Pts',(7.27603390513785,-98.0795179709984,4.20082013374672));
#24838=CARTESIAN_POINT('Ctrl Pts',(9.70137854017372,-97.9045179709984,-1.74689612655491E-11));
#24839=CARTESIAN_POINT('Ctrl Pts',(7.27603390512273,-97.7295179709984,-4.20082013377291));
#24840=CARTESIAN_POINT('Ctrl Pts',(4.85068927007173,-97.5545179709984,-8.40164026752836));
#24841=CARTESIAN_POINT('Ctrl Pts',(-1.51301075899711E-11,-97.3795179709984,
-8.40164026751963));
#24842=CARTESIAN_POINT('Ctrl Pts',(-4.85068927010199,-97.2045179709984,
-8.4016402675109));
#24843=CARTESIAN_POINT('Ctrl Pts',(-7.27603390513785,-97.0295179709984,
-4.20082013374671));
#24844=CARTESIAN_POINT('Ctrl Pts',(-9.70137854017372,-96.8545179709984,
1.74701493417668E-11));
#24845=CARTESIAN_POINT('Ctrl Pts',(-7.27603390512272,-96.6795179709984,
4.20082013377292));
#24846=CARTESIAN_POINT('Ctrl Pts',(-4.85068927007173,-96.5045179709984,
8.40164026752836));
#24847=CARTESIAN_POINT('Ctrl Pts',(1.5129078685785E-11,-96.3295179709984,
8.40164026751963));
#24848=CARTESIAN_POINT('Ctrl Pts',(4.85068927010198,-96.1545179709984,8.4016402675109));
#24849=CARTESIAN_POINT('Ctrl Pts',(7.27603390513785,-95.9795179709984,4.20082013374672));
#24850=CARTESIAN_POINT('Ctrl Pts',(9.70137854017372,-95.8045179709984,-1.74689612655491E-11));
#24851=CARTESIAN_POINT('Ctrl Pts',(7.27603390512273,-95.6295179709984,-4.20082013377291));
#24852=CARTESIAN_POINT('Ctrl Pts',(4.85068927007173,-95.4545179709984,-8.40164026752836));
#24853=CARTESIAN_POINT('Ctrl Pts',(-1.51301075899711E-11,-95.2795179709984,
-8.40164026751963));
#24854=CARTESIAN_POINT('Ctrl Pts',(-4.85068927010199,-95.1045179709984,
-8.4016402675109));
#24855=CARTESIAN_POINT('Ctrl Pts',(-7.27603390513785,-94.9295179709984,
-4.20082013374671));
#24856=CARTESIAN_POINT('Ctrl Pts',(-9.70137854017372,-94.7545179709984,
1.74701493417668E-11));
#24857=CARTESIAN_POINT('Ctrl Pts',(-7.27603390512272,-94.5795179709984,
4.20082013377292));
#24858=CARTESIAN_POINT('Ctrl Pts',(-4.85068927007173,-94.4045179709984,
8.40164026752836));
#24859=CARTESIAN_POINT('Ctrl Pts',(1.5129078685785E-11,-94.2295179709984,
8.40164026751963));
#24860=CARTESIAN_POINT('Ctrl Pts',(4.85068927010198,-94.0545179709984,8.4016402675109));
#24861=CARTESIAN_POINT('Ctrl Pts',(7.27603390513785,-93.8795179709984,4.20082013374672));
#24862=CARTESIAN_POINT('Ctrl Pts',(9.70137854017372,-93.7045179709984,-1.74689612655491E-11));
#24863=CARTESIAN_POINT('Ctrl Pts',(7.27603390512273,-93.5295179709984,-4.20082013377291));
#24864=CARTESIAN_POINT('Ctrl Pts',(4.85068927007173,-93.3545179709984,-8.40164026752836));
#24865=CARTESIAN_POINT('Ctrl Pts',(-1.51301075899711E-11,-93.1795179709984,
-8.40164026751963));
#24866=CARTESIAN_POINT('Ctrl Pts',(-4.85068927010199,-93.0045179709984,
-8.4016402675109));
#24867=CARTESIAN_POINT('Ctrl Pts',(-7.27603390513785,-92.8295179709984,
-4.20082013374671));
#24868=CARTESIAN_POINT('Ctrl Pts',(-9.70137854017372,-92.6545179709984,
1.74701493417668E-11));
#24869=CARTESIAN_POINT('Ctrl Pts',(-7.27603390512272,-92.4795179709984,
4.20082013377292));
#24870=CARTESIAN_POINT('Ctrl Pts',(-4.85068927007173,-92.3045179709984,
8.40164026752836));
#24871=CARTESIAN_POINT('Ctrl Pts',(1.5129078685785E-11,-92.1295179709984,
8.40164026751963));
#24872=CARTESIAN_POINT('Ctrl Pts',(4.85068927010198,-91.9545179709984,8.4016402675109));
#24873=CARTESIAN_POINT('Ctrl Pts',(7.27603390513785,-91.7795179709984,4.20082013374672));
#24874=CARTESIAN_POINT('Ctrl Pts',(9.70137854017372,-91.6045179709984,-1.74689612655491E-11));
#24875=CARTESIAN_POINT('Ctrl Pts',(7.27603390512273,-91.4295179709984,-4.20082013377291));
#24876=CARTESIAN_POINT('Ctrl Pts',(4.85068927007173,-91.2545179709984,-8.40164026752836));
#24877=CARTESIAN_POINT('Ctrl Pts',(-1.51301075899711E-11,-91.0795179709984,
-8.40164026751963));
#24878=CARTESIAN_POINT('Ctrl Pts',(-4.85068927010199,-90.9045179709984,
-8.4016402675109));
#24879=CARTESIAN_POINT('Ctrl Pts',(-7.27603390513785,-90.7295179709984,
-4.20082013374671));
#24880=CARTESIAN_POINT('Ctrl Pts',(-9.70137854017372,-90.5545179709984,
1.74701493417668E-11));
#24881=CARTESIAN_POINT('Ctrl Pts',(-7.27603390512272,-90.3795179709984,
4.20082013377292));
#24882=CARTESIAN_POINT('Ctrl Pts',(-4.85068927007173,-90.2045179709984,
8.40164026752836));
#24883=CARTESIAN_POINT('Ctrl Pts',(1.5129078685785E-11,-90.0295179709984,
8.40164026751963));
#24884=CARTESIAN_POINT('Ctrl Pts',(4.85068927010198,-89.8545179709984,8.4016402675109));
#24885=CARTESIAN_POINT('Ctrl Pts',(7.27603390513785,-89.6795179709984,4.20082013374672));
#24886=CARTESIAN_POINT('Ctrl Pts',(9.70137854017372,-89.5045179709984,-1.74689612655491E-11));
#24887=CARTESIAN_POINT('Ctrl Pts',(7.27603390512273,-89.3295179709984,-4.20082013377291));
#24888=CARTESIAN_POINT('Ctrl Pts',(4.85068927007173,-89.1545179709984,-8.40164026752836));
#24889=CARTESIAN_POINT('Ctrl Pts',(-1.51301075899711E-11,-88.9795179709984,
-8.40164026751963));
#24890=CARTESIAN_POINT('Ctrl Pts',(-4.85068927010199,-88.8045179709984,
-8.4016402675109));
#24891=CARTESIAN_POINT('Ctrl Pts',(-7.27603390513785,-88.6295179709984,
-4.20082013374671));
#24892=CARTESIAN_POINT('Ctrl Pts',(-9.70137854017372,-88.4545179709984,
1.74701493417668E-11));
#24893=CARTESIAN_POINT('Ctrl Pts',(-7.27603390512272,-88.2795179709984,
4.20082013377292));
#24894=CARTESIAN_POINT('Ctrl Pts',(-4.85068927007173,-88.1045179709984,
8.40164026752836));
#24895=CARTESIAN_POINT('Ctrl Pts',(1.5129078685785E-11,-87.9295179709984,
8.40164026751963));
#24896=CARTESIAN_POINT('Ctrl Pts',(4.85068927010198,-87.7545179709984,8.4016402675109));
#24897=CARTESIAN_POINT('Ctrl Pts',(7.27603390513785,-87.5795179709984,4.20082013374672));
#24898=CARTESIAN_POINT('Ctrl Pts',(9.70137854017372,-87.4045179709984,-1.74689612655491E-11));
#24899=CARTESIAN_POINT('Ctrl Pts',(7.27603390512273,-87.2295179709984,-4.20082013377291));
#24900=CARTESIAN_POINT('Ctrl Pts',(4.85068927007173,-87.0545179709984,-8.40164026752836));
#24901=CARTESIAN_POINT('Ctrl Pts',(-1.51301075899711E-11,-86.8795179709984,
-8.40164026751963));
#24902=CARTESIAN_POINT('Ctrl Pts',(-4.85068927010199,-86.7045179709984,
-8.4016402675109));
#24903=CARTESIAN_POINT('Ctrl Pts',(-7.27603390513785,-86.5295179709984,
-4.20082013374671));
#24904=CARTESIAN_POINT('Ctrl Pts',(-9.70137854017372,-86.3545179709984,
1.74701493417668E-11));
#24905=CARTESIAN_POINT('Ctrl Pts',(-7.27603390512272,-86.1795179709984,
4.20082013377292));
#24906=CARTESIAN_POINT('Ctrl Pts',(-4.85068927007173,-86.0045179709984,
8.40164026752836));
#24907=CARTESIAN_POINT('Ctrl Pts',(1.5129078685785E-11,-85.8295179709984,
8.40164026751963));
#24908=CARTESIAN_POINT('Ctrl Pts',(4.85068927010198,-85.6545179709984,8.4016402675109));
#24909=CARTESIAN_POINT('Ctrl Pts',(7.27603390513785,-85.4795179709984,4.20082013374672));
#24910=CARTESIAN_POINT('Ctrl Pts',(9.70137854017372,-85.3045179709984,-1.74689612655491E-11));
#24911=CARTESIAN_POINT('Ctrl Pts',(7.27603390512273,-85.1295179709984,-4.20082013377291));
#24912=CARTESIAN_POINT('Ctrl Pts',(4.85068927007173,-84.9545179709984,-8.40164026752836));
#24913=CARTESIAN_POINT('Ctrl Pts',(-1.51301075899711E-11,-84.7795179709984,
-8.40164026751963));
#24914=CARTESIAN_POINT('Ctrl Pts',(-4.85068927010199,-84.6045179709984,
-8.4016402675109));
#24915=CARTESIAN_POINT('Ctrl Pts',(-7.27603390513785,-84.4295179709984,
-4.20082013374671));
#24916=CARTESIAN_POINT('Ctrl Pts',(-9.70137854017372,-84.2545179709984,
1.74701493417668E-11));
#24917=CARTESIAN_POINT('Ctrl Pts',(-7.27603390512272,-84.0795179709984,
4.20082013377292));
#24918=CARTESIAN_POINT('Ctrl Pts',(-4.85068927007173,-83.9045179709984,
8.40164026752836));
#24919=CARTESIAN_POINT('Ctrl Pts',(1.5129078685785E-11,-83.7295179709984,
8.40164026751963));
#24920=CARTESIAN_POINT('Ctrl Pts',(4.85068927010198,-83.5545179709984,8.4016402675109));
#24921=CARTESIAN_POINT('Ctrl Pts',(7.27603390513785,-83.3795179709984,4.20082013374672));
#24922=CARTESIAN_POINT('Ctrl Pts',(9.70137854017372,-83.2045179709984,-1.74689612655491E-11));
#24923=CARTESIAN_POINT('Ctrl Pts',(7.27603390512273,-83.0295179709984,-4.20082013377291));
#24924=CARTESIAN_POINT('Ctrl Pts',(4.85068927007173,-82.8545179709984,-8.40164026752836));
#24925=CARTESIAN_POINT('Ctrl Pts',(-1.51301075899711E-11,-82.6795179709984,
-8.40164026751963));
#24926=CARTESIAN_POINT('Ctrl Pts',(-4.85068927010199,-82.5045179709984,
-8.4016402675109));
#24927=CARTESIAN_POINT('Ctrl Pts',(-7.27603390513785,-82.3295179709984,
-4.20082013374671));
#24928=CARTESIAN_POINT('Ctrl Pts',(-9.70137854017372,-82.1545179709984,
1.74701493417668E-11));
#24929=CARTESIAN_POINT('Ctrl Pts',(-7.27603390512272,-81.9795179709984,
4.20082013377292));
#24930=CARTESIAN_POINT('Ctrl Pts',(-4.85068927007173,-81.8045179709984,
8.40164026752836));
#24931=CARTESIAN_POINT('Ctrl Pts',(1.5129078685785E-11,-81.6295179709984,
8.40164026751963));
#24932=CARTESIAN_POINT('Ctrl Pts',(4.85068927010198,-81.4545179709984,8.4016402675109));
#24933=CARTESIAN_POINT('Ctrl Pts',(7.27603390513785,-81.2795179709984,4.20082013374672));
#24934=CARTESIAN_POINT('Ctrl Pts',(9.70137854017372,-81.1045179709984,-1.74689612655491E-11));
#24935=CARTESIAN_POINT('Ctrl Pts',(7.27603390512273,-80.9295179709984,-4.20082013377291));
#24936=CARTESIAN_POINT('Ctrl Pts',(4.85068927007173,-80.7545179709984,-8.40164026752836));
#24937=CARTESIAN_POINT('Ctrl Pts',(-1.51301075899711E-11,-80.5795179709984,
-8.40164026751963));
#24938=CARTESIAN_POINT('Ctrl Pts',(-4.85068927010199,-80.4045179709985,
-8.4016402675109));
#24939=CARTESIAN_POINT('Ctrl Pts',(-7.27603390513785,-80.2295179709984,
-4.20082013374671));
#24940=CARTESIAN_POINT('Ctrl Pts',(-9.70137854017372,-80.0545179709984,
1.74701493417668E-11));
#24941=CARTESIAN_POINT('Ctrl Pts',(-7.27603390512272,-79.8795179709984,
4.20082013377292));
#24942=CARTESIAN_POINT('Ctrl Pts',(-4.85068927007173,-79.7045179709984,
8.40164026752836));
#24943=CARTESIAN_POINT('Ctrl Pts',(1.5129078685785E-11,-79.5295179709984,
8.40164026751963));
#24944=CARTESIAN_POINT('Ctrl Pts',(4.85068927010198,-79.3545179709984,8.4016402675109));
#24945=CARTESIAN_POINT('Ctrl Pts',(7.27603390513785,-79.1795179709984,4.20082013374672));
#24946=CARTESIAN_POINT('Ctrl Pts',(9.70137854017372,-79.0045179709984,-1.74689612655491E-11));
#24947=CARTESIAN_POINT('Ctrl Pts',(7.27603390512273,-78.8295179709984,-4.20082013377291));
#24948=CARTESIAN_POINT('Ctrl Pts',(4.85068927007173,-78.6545179709984,-8.40164026752836));
#24949=CARTESIAN_POINT('Ctrl Pts',(-1.51301075899711E-11,-78.4795179709984,
-8.40164026751963));
#24950=CARTESIAN_POINT('Ctrl Pts',(-4.85068927010199,-78.3045179709985,
-8.4016402675109));
#24951=CARTESIAN_POINT('Ctrl Pts',(-7.27603390513785,-78.1295179709984,
-4.20082013374671));
#24952=CARTESIAN_POINT('Ctrl Pts',(-9.70137854017372,-77.9545179709984,
1.74701493417668E-11));
#24953=CARTESIAN_POINT('Ctrl Pts',(-7.27603390512272,-77.7795179709984,
4.20082013377292));
#24954=CARTESIAN_POINT('Ctrl Pts',(-4.85068927007173,-77.6045179709984,
8.40164026752836));
#24955=CARTESIAN_POINT('Ctrl Pts',(1.5129078685785E-11,-77.4295179709984,
8.40164026751963));
#24956=CARTESIAN_POINT('Ctrl Pts',(4.85068927010198,-77.2545179709984,8.4016402675109));
#24957=CARTESIAN_POINT('Ctrl Pts',(7.27603390513785,-77.0795179709984,4.20082013374672));
#24958=CARTESIAN_POINT('Ctrl Pts',(9.70137854017372,-76.9045179709984,-1.74689612655491E-11));
#24959=CARTESIAN_POINT('Ctrl Pts',(7.27603390512273,-76.7295179709984,-4.20082013377291));
#24960=CARTESIAN_POINT('Ctrl Pts',(4.85068927007173,-76.5545179709984,-8.40164026752836));
#24961=CARTESIAN_POINT('Ctrl Pts',(-1.51301075899711E-11,-76.3795179709984,
-8.40164026751963));
#24962=CARTESIAN_POINT('Ctrl Pts',(-4.85068927010199,-76.2045179709985,
-8.4016402675109));
#24963=CARTESIAN_POINT('Ctrl Pts',(-7.27603390513785,-76.0295179709984,
-4.20082013374671));
#24964=CARTESIAN_POINT('Ctrl Pts',(-9.70137854017372,-75.8545179709985,
1.74701493417668E-11));
#24965=CARTESIAN_POINT('Ctrl Pts',(-7.27603390512272,-75.6795179709984,
4.20082013377292));
#24966=CARTESIAN_POINT('Ctrl Pts',(-4.85068927007173,-75.5045179709984,
8.40164026752836));
#24967=CARTESIAN_POINT('Ctrl Pts',(1.5129078685785E-11,-75.3295179709984,
8.40164026751963));
#24968=CARTESIAN_POINT('Ctrl Pts',(4.85068927010198,-75.1545179709984,8.4016402675109));
#24969=CARTESIAN_POINT('Ctrl Pts',(7.27603390513785,-74.9795179709984,4.20082013374672));
#24970=CARTESIAN_POINT('Ctrl Pts',(9.70137854017372,-74.8045179709984,-1.74689612655491E-11));
#24971=CARTESIAN_POINT('Ctrl Pts',(7.27603390512273,-74.6295179709984,-4.20082013377291));
#24972=CARTESIAN_POINT('Ctrl Pts',(4.85068927007173,-74.4545179709984,-8.40164026752836));
#24973=CARTESIAN_POINT('Ctrl Pts',(-1.51301075899711E-11,-74.2795179709984,
-8.40164026751963));
#24974=CARTESIAN_POINT('Ctrl Pts',(-4.85068927010199,-74.1045179709984,
-8.4016402675109));
#24975=CARTESIAN_POINT('Ctrl Pts',(-7.27603390513785,-73.9295179709984,
-4.20082013374671));
#24976=CARTESIAN_POINT('Ctrl Pts',(-9.70137854017372,-73.7545179709984,
1.74701493417668E-11));
#24977=CARTESIAN_POINT('Ctrl Pts',(-7.27603390512272,-73.5795179709984,
4.20082013377292));
#24978=CARTESIAN_POINT('Ctrl Pts',(-4.85068927007173,-73.4045179709984,
8.40164026752836));
#24979=CARTESIAN_POINT('Ctrl Pts',(1.5129078685785E-11,-73.2295179709984,
8.40164026751963));
#24980=CARTESIAN_POINT('Ctrl Pts',(4.85068927010198,-73.0545179709984,8.4016402675109));
#24981=CARTESIAN_POINT('Ctrl Pts',(7.27603390513785,-72.8795179709984,4.20082013374672));
#24982=CARTESIAN_POINT('Ctrl Pts',(9.70137854017372,-72.7045179709984,-1.74689612655491E-11));
#24983=CARTESIAN_POINT('Ctrl Pts',(7.27603390512273,-72.5295179709984,-4.20082013377291));
#24984=CARTESIAN_POINT('Ctrl Pts',(4.85068927007173,-72.3545179709984,-8.40164026752836));
#24985=CARTESIAN_POINT('Ctrl Pts',(-1.51301075899711E-11,-72.1795179709984,
-8.40164026751963));
#24986=CARTESIAN_POINT('Ctrl Pts',(-4.85068927010199,-72.0045179709984,
-8.4016402675109));
#24987=CARTESIAN_POINT('Ctrl Pts',(-7.27603390513785,-71.8295179709984,
-4.20082013374671));
#24988=CARTESIAN_POINT('Ctrl Pts',(-9.70137854017372,-71.6545179709985,
1.74701493417668E-11));
#24989=CARTESIAN_POINT('Ctrl Pts',(-7.27603390512272,-71.4795179709984,
4.20082013377292));
#24990=CARTESIAN_POINT('Ctrl Pts',(-4.85068927007173,-71.3045179709984,
8.40164026752836));
#24991=CARTESIAN_POINT('Ctrl Pts',(1.5129078685785E-11,-71.1295179709984,
8.40164026751963));
#24992=CARTESIAN_POINT('Ctrl Pts',(4.85068927010198,-70.9545179709984,8.4016402675109));
#24993=CARTESIAN_POINT('Ctrl Pts',(7.27603390513785,-70.7795179709984,4.20082013374672));
#24994=CARTESIAN_POINT('Ctrl Pts',(9.70137854017372,-70.6045179709985,-1.74689612655491E-11));
#24995=CARTESIAN_POINT('Ctrl Pts',(7.27603390512273,-70.4295179709984,-4.20082013377291));
#24996=CARTESIAN_POINT('Ctrl Pts',(4.85068927007173,-70.2545179709984,-8.40164026752836));
#24997=CARTESIAN_POINT('Ctrl Pts',(-1.51301075899711E-11,-70.0795179709985,
-8.40164026751963));
#24998=CARTESIAN_POINT('Ctrl Pts',(-4.85068927010199,-69.9045179709984,
-8.4016402675109));
#24999=CARTESIAN_POINT('Ctrl Pts',(-7.27603390513785,-69.7295179709984,
-4.20082013374671));
#25000=CARTESIAN_POINT('Ctrl Pts',(-9.70137854017372,-69.5545179709985,
1.74701493417668E-11));
#25001=CARTESIAN_POINT('Ctrl Pts',(-7.27603390512272,-69.3795179709984,
4.20082013377292));
#25002=CARTESIAN_POINT('Ctrl Pts',(-4.85068927007173,-69.2045179709985,
8.40164026752836));
#25003=CARTESIAN_POINT('Ctrl Pts',(1.5129078685785E-11,-69.0295179709985,
8.40164026751963));
#25004=CARTESIAN_POINT('Ctrl Pts',(4.85068927010198,-68.8545179709984,8.4016402675109));
#25005=CARTESIAN_POINT('Ctrl Pts',(7.27603390513785,-68.6795179709985,4.20082013374672));
#25006=CARTESIAN_POINT('Ctrl Pts',(9.70137854017372,-68.5045179709985,-1.74689612655491E-11));
#25007=CARTESIAN_POINT('Ctrl Pts',(7.27603390512273,-68.3295179709984,-4.20082013377291));
#25008=CARTESIAN_POINT('Ctrl Pts',(4.85068927007173,-68.1545179709985,-8.40164026752836));
#25009=CARTESIAN_POINT('Ctrl Pts',(-1.51301075899711E-11,-67.9795179709985,
-8.40164026751963));
#25010=CARTESIAN_POINT('Ctrl Pts',(-4.85068927010199,-67.8045179709984,
-8.4016402675109));
#25011=CARTESIAN_POINT('Ctrl Pts',(-7.27603390513785,-67.6295179709984,
-4.20082013374671));
#25012=CARTESIAN_POINT('Ctrl Pts',(-9.70137854017372,-67.4545179709985,
1.74701493417668E-11));
#25013=CARTESIAN_POINT('Ctrl Pts',(-7.27603390512272,-67.2795179709984,
4.20082013377292));
#25014=CARTESIAN_POINT('Ctrl Pts',(-4.85068927007173,-67.1045179709985,
8.40164026752836));
#25015=CARTESIAN_POINT('Ctrl Pts',(1.5129078685785E-11,-66.9295179709985,
8.40164026751963));
#25016=CARTESIAN_POINT('Ctrl Pts',(4.85068927010198,-66.7545179709984,8.4016402675109));
#25017=CARTESIAN_POINT('Ctrl Pts',(7.27603390513785,-66.5795179709985,4.20082013374672));
#25018=CARTESIAN_POINT('Ctrl Pts',(9.70137854017372,-66.4045179709985,-1.74689612655491E-11));
#25019=CARTESIAN_POINT('Ctrl Pts',(7.27603390512273,-66.2295179709984,-4.20082013377291));
#25020=CARTESIAN_POINT('Ctrl Pts',(4.85068927007173,-66.0545179709985,-8.40164026752836));
#25021=CARTESIAN_POINT('Ctrl Pts',(-1.51301075899711E-11,-65.8795179709984,
-8.40164026751963));
#25022=CARTESIAN_POINT('Ctrl Pts',(-4.85068927010199,-65.7045179709985,
-8.4016402675109));
#25023=CARTESIAN_POINT('Ctrl Pts',(-7.27603390513785,-65.5295179709985,
-4.20082013374671));
#25024=CARTESIAN_POINT('Ctrl Pts',(-9.70137854017372,-65.3545179709984,
1.74701493417668E-11));
#25025=CARTESIAN_POINT('Ctrl Pts',(-7.27603390512272,-65.1795179709984,
4.20082013377292));
#25026=CARTESIAN_POINT('Ctrl Pts',(-4.85068927007173,-65.0045179709985,
8.40164026752836));
#25027=CARTESIAN_POINT('Ctrl Pts',(1.5129078685785E-11,-64.8295179709985,
8.40164026751963));
#25028=CARTESIAN_POINT('Ctrl Pts',(4.85068927010198,-64.6545179709985,8.4016402675109));
#25029=CARTESIAN_POINT('Ctrl Pts',(7.27603390513785,-64.4795179709985,4.20082013374672));
#25030=CARTESIAN_POINT('Ctrl Pts',(9.70137854017372,-64.3045179709985,-1.74689612655491E-11));
#25031=CARTESIAN_POINT('Ctrl Pts',(7.27603390512273,-64.1295179709984,-4.20082013377291));
#25032=CARTESIAN_POINT('Ctrl Pts',(4.85068927007173,-63.9545179709985,-8.40164026752836));
#25033=CARTESIAN_POINT('Ctrl Pts',(-1.51301075899711E-11,-63.7795179709985,
-8.40164026751963));
#25034=CARTESIAN_POINT('Ctrl Pts',(-4.85068927010199,-63.6045179709985,
-8.4016402675109));
#25035=CARTESIAN_POINT('Ctrl Pts',(-7.27603390513785,-63.4295179709985,
-4.20082013374671));
#25036=CARTESIAN_POINT('Ctrl Pts',(-9.70137854017372,-63.2545179709985,
1.74701493417668E-11));
#25037=CARTESIAN_POINT('Ctrl Pts',(-7.27603390512272,-63.0795179709985,
4.20082013377292));
#25038=CARTESIAN_POINT('Ctrl Pts',(-4.85068927007173,-62.9045179709985,
8.40164026752836));
#25039=CARTESIAN_POINT('Ctrl Pts',(1.5129078685785E-11,-62.7295179709985,
8.40164026751963));
#25040=CARTESIAN_POINT('Ctrl Pts',(4.85068927010198,-62.5545179709985,8.4016402675109));
#25041=CARTESIAN_POINT('Ctrl Pts',(7.27603390513785,-62.3795179709985,4.20082013374672));
#25042=CARTESIAN_POINT('Ctrl Pts',(9.70137854017372,-62.2045179709985,-1.74689612655491E-11));
#25043=CARTESIAN_POINT('Ctrl Pts',(7.27603390512273,-62.0295179709985,-4.20082013377291));
#25044=CARTESIAN_POINT('Ctrl Pts',(4.85068927007173,-61.8545179709985,-8.40164026752836));
#25045=CARTESIAN_POINT('Ctrl Pts',(-1.51301075899711E-11,-61.6795179709985,
-8.40164026751963));
#25046=CARTESIAN_POINT('Ctrl Pts',(-4.85068927010199,-61.5045179709985,
-8.4016402675109));
#25047=CARTESIAN_POINT('Ctrl Pts',(-7.27603390513785,-61.3295179709985,
-4.20082013374671));
#25048=CARTESIAN_POINT('Ctrl Pts',(-9.70137854017372,-61.1545179709985,
1.74701493417668E-11));
#25049=CARTESIAN_POINT('Ctrl Pts',(-7.27603390512272,-60.9795179709985,
4.20082013377292));
#25050=CARTESIAN_POINT('Ctrl Pts',(-4.85068927007173,-60.8045179709985,
8.40164026752836));
#25051=CARTESIAN_POINT('Ctrl Pts',(1.5129078685785E-11,-60.6295179709985,
8.40164026751963));
#25052=CARTESIAN_POINT('Ctrl Pts',(4.85068927010198,-60.4545179709985,8.4016402675109));
#25053=CARTESIAN_POINT('Ctrl Pts',(7.27603390513785,-60.2795179709985,4.20082013374672));
#25054=CARTESIAN_POINT('Ctrl Pts',(9.70137854017372,-60.1045179709985,-1.74689612655491E-11));
#25055=CARTESIAN_POINT('Ctrl Pts',(7.27603390512273,-59.9295179709985,-4.20082013377291));
#25056=CARTESIAN_POINT('Ctrl Pts',(4.85068927007173,-59.7545179709985,-8.40164026752836));
#25057=CARTESIAN_POINT('Ctrl Pts',(-1.51301075899711E-11,-59.5795179709985,
-8.40164026751963));
#25058=CARTESIAN_POINT('Ctrl Pts',(-4.85068927010199,-59.4045179709985,
-8.4016402675109));
#25059=CARTESIAN_POINT('Ctrl Pts',(-7.27603390513785,-59.2295179709985,
-4.20082013374671));
#25060=CARTESIAN_POINT('Ctrl Pts',(-9.70137854017372,-59.0545179709985,
1.74701493417668E-11));
#25061=CARTESIAN_POINT('Ctrl Pts',(-7.27603390512272,-58.8795179709985,
4.20082013377292));
#25062=CARTESIAN_POINT('Ctrl Pts',(-4.85068927007173,-58.7045179709985,
8.40164026752836));
#25063=CARTESIAN_POINT('Ctrl Pts',(1.5129078685785E-11,-58.5295179709984,
8.40164026751963));
#25064=CARTESIAN_POINT('Ctrl Pts',(4.85068927010198,-58.3545179709985,8.4016402675109));
#25065=CARTESIAN_POINT('Ctrl Pts',(7.27603390513785,-58.1795179709985,4.20082013374672));
#25066=CARTESIAN_POINT('Ctrl Pts',(9.70137854017372,-58.0045179709985,-1.74689612655491E-11));
#25067=CARTESIAN_POINT('Ctrl Pts',(7.27603390512273,-57.8295179709985,-4.20082013377291));
#25068=CARTESIAN_POINT('Ctrl Pts',(4.85068927007173,-57.6545179709985,-8.40164026752836));
#25069=CARTESIAN_POINT('Ctrl Pts',(-1.51301075899711E-11,-57.4795179709985,
-8.40164026751963));
#25070=CARTESIAN_POINT('Ctrl Pts',(-4.85068927010199,-57.3045179709985,
-8.4016402675109));
#25071=CARTESIAN_POINT('Ctrl Pts',(-7.27603390513785,-57.1295179709985,
-4.20082013374671));
#25072=CARTESIAN_POINT('Ctrl Pts',(-9.70137854017372,-56.9545179709985,
1.74701493417668E-11));
#25073=CARTESIAN_POINT('Ctrl Pts',(-7.27603390512272,-56.7795179709985,
4.20082013377292));
#25074=CARTESIAN_POINT('Ctrl Pts',(-4.85068927007173,-56.6045179709985,
8.40164026752836));
#25075=CARTESIAN_POINT('Ctrl Pts',(1.5129078685785E-11,-56.4295179709985,
8.40164026751963));
#25076=CARTESIAN_POINT('Ctrl Pts',(4.85068927010198,-56.2545179709985,8.4016402675109));
#25077=CARTESIAN_POINT('Ctrl Pts',(7.27603390513785,-56.0795179709985,4.20082013374672));
#25078=CARTESIAN_POINT('Ctrl Pts',(9.70137854017372,-55.9045179709985,-1.74689612655491E-11));
#25079=CARTESIAN_POINT('Ctrl Pts',(7.27603390512273,-55.7295179709985,-4.20082013377291));
#25080=CARTESIAN_POINT('Ctrl Pts',(4.85068927007173,-55.5545179709985,-8.40164026752836));
#25081=CARTESIAN_POINT('Ctrl Pts',(-1.51301075899711E-11,-55.3795179709985,
-8.40164026751963));
#25082=CARTESIAN_POINT('Ctrl Pts',(-4.85068927010199,-55.2045179709985,
-8.4016402675109));
#25083=CARTESIAN_POINT('Ctrl Pts',(-7.27603390513785,-55.0295179709985,
-4.20082013374671));
#25084=CARTESIAN_POINT('Ctrl Pts',(-9.70137854017372,-54.8545179709985,
1.74701493417668E-11));
#25085=CARTESIAN_POINT('Ctrl Pts',(-7.27603390512272,-54.6795179709985,
4.20082013377292));
#25086=CARTESIAN_POINT('Ctrl Pts',(-4.85068927007173,-54.5045179709985,
8.40164026752836));
#25087=CARTESIAN_POINT('Ctrl Pts',(1.5129078685785E-11,-54.3295179709985,
8.40164026751963));
#25088=CARTESIAN_POINT('Ctrl Pts',(4.85068927010198,-54.1545179709985,8.4016402675109));
#25089=CARTESIAN_POINT('Ctrl Pts',(7.27603390513785,-53.9795179709985,4.20082013374672));
#25090=CARTESIAN_POINT('Ctrl Pts',(9.70137854017372,-53.8045179709985,-1.74689612655491E-11));
#25091=CARTESIAN_POINT('Ctrl Pts',(7.27603390512273,-53.6295179709985,-4.20082013377291));
#25092=CARTESIAN_POINT('Ctrl Pts',(4.85068927007173,-53.4545179709985,-8.40164026752836));
#25093=CARTESIAN_POINT('Ctrl Pts',(-1.51301075899711E-11,-53.2795179709985,
-8.40164026751963));
#25094=CARTESIAN_POINT('Ctrl Pts',(-4.85068927010199,-53.1045179709985,
-8.4016402675109));
#25095=CARTESIAN_POINT('Ctrl Pts',(-7.27603390513785,-52.9295179709985,
-4.20082013374671));
#25096=CARTESIAN_POINT('Ctrl Pts',(-9.70137854017372,-52.7545179709985,
1.74701493417668E-11));
#25097=CARTESIAN_POINT('Ctrl Pts',(-7.27603390512272,-52.5795179709985,
4.20082013377292));
#25098=CARTESIAN_POINT('Ctrl Pts',(-4.85068927007173,-52.4045179709985,
8.40164026752836));
#25099=CARTESIAN_POINT('Ctrl Pts',(1.5129078685785E-11,-52.2295179709985,
8.40164026751963));
#25100=CARTESIAN_POINT('Ctrl Pts',(4.85068927010198,-52.0545179709985,8.4016402675109));
#25101=CARTESIAN_POINT('Ctrl Pts',(7.27603390513785,-51.8795179709985,4.20082013374672));
#25102=CARTESIAN_POINT('Ctrl Pts',(9.70137854017372,-51.7045179709985,-1.74689612655491E-11));
#25103=CARTESIAN_POINT('Ctrl Pts',(7.27603390512273,-51.5295179709985,-4.20082013377291));
#25104=CARTESIAN_POINT('Ctrl Pts',(4.85068927007173,-51.3545179709985,-8.40164026752836));
#25105=CARTESIAN_POINT('Ctrl Pts',(-1.51301075899711E-11,-51.1795179709985,
-8.40164026751963));
#25106=CARTESIAN_POINT('Ctrl Pts',(-4.85068927010199,-51.0045179709985,
-8.4016402675109));
#25107=CARTESIAN_POINT('Ctrl Pts',(-7.27603390513785,-50.8295179709985,
-4.20082013374671));
#25108=CARTESIAN_POINT('Ctrl Pts',(-9.70137854017372,-50.6545179709985,
1.74701493417668E-11));
#25109=CARTESIAN_POINT('Ctrl Pts',(-7.27603390512272,-50.4795179709985,
4.20082013377292));
#25110=CARTESIAN_POINT('Ctrl Pts',(-4.85068927007173,-50.3045179709985,
8.40164026752836));
#25111=CARTESIAN_POINT('Ctrl Pts',(1.5129078685785E-11,-50.1295179709985,
8.40164026751963));
#25112=CARTESIAN_POINT('Ctrl Pts',(4.85068927010198,-49.9545179709985,8.4016402675109));
#25113=CARTESIAN_POINT('Ctrl Pts',(7.27603390513785,-49.7795179709985,4.20082013374672));
#25114=CARTESIAN_POINT('Ctrl Pts',(9.70137854017372,-49.6045179709985,-1.74689612655491E-11));
#25115=CARTESIAN_POINT('Ctrl Pts',(7.27603390512273,-49.4295179709985,-4.20082013377291));
#25116=CARTESIAN_POINT('Ctrl Pts',(4.85068927007173,-49.2545179709985,-8.40164026752836));
#25117=CARTESIAN_POINT('Ctrl Pts',(-1.51301075899711E-11,-49.0795179709985,
-8.40164026751963));
#25118=CARTESIAN_POINT('Ctrl Pts',(-4.85068927010199,-48.9045179709985,
-8.4016402675109));
#25119=CARTESIAN_POINT('Ctrl Pts',(-7.27603390513785,-48.7295179709985,
-4.20082013374671));
#25120=CARTESIAN_POINT('Ctrl Pts',(-9.70137854017372,-48.5545179709985,
1.74701493417668E-11));
#25121=CARTESIAN_POINT('Ctrl Pts',(-7.27603390512272,-48.3795179709985,
4.20082013377292));
#25122=CARTESIAN_POINT('Ctrl Pts',(-4.85068927007173,-48.2045179709985,
8.40164026752836));
#25123=CARTESIAN_POINT('Ctrl Pts',(1.5129078685785E-11,-48.0295179709985,
8.40164026751963));
#25124=CARTESIAN_POINT('Ctrl Pts',(4.85068927010198,-47.8545179709985,8.4016402675109));
#25125=CARTESIAN_POINT('Ctrl Pts',(7.27603390513785,-47.6795179709985,4.20082013374672));
#25126=CARTESIAN_POINT('Ctrl Pts',(9.70137854017372,-47.5045179709985,-1.74689612655491E-11));
#25127=CARTESIAN_POINT('Ctrl Pts',(7.27603390512273,-47.3295179709985,-4.20082013377291));
#25128=CARTESIAN_POINT('Ctrl Pts',(4.85068927007173,-47.1545179709985,-8.40164026752836));
#25129=CARTESIAN_POINT('Ctrl Pts',(-1.51301075899711E-11,-46.9795179709985,
-8.40164026751963));
#25130=CARTESIAN_POINT('Ctrl Pts',(-4.85068927010199,-46.8045179709985,
-8.4016402675109));
#25131=CARTESIAN_POINT('Ctrl Pts',(-7.27603390513785,-46.6295179709985,
-4.20082013374671));
#25132=CARTESIAN_POINT('Ctrl Pts',(-9.70137854017372,-46.4545179709985,
1.74701493417668E-11));
#25133=CARTESIAN_POINT('Ctrl Pts',(-7.27603390512272,-46.2795179709985,
4.20082013377292));
#25134=CARTESIAN_POINT('Ctrl Pts',(-4.85068927007173,-46.1045179709985,
8.40164026752836));
#25135=CARTESIAN_POINT('Ctrl Pts',(1.5129078685785E-11,-45.9295179709985,
8.40164026751963));
#25136=CARTESIAN_POINT('Ctrl Pts',(4.85068927010198,-45.7545179709985,8.4016402675109));
#25137=CARTESIAN_POINT('Ctrl Pts',(7.27603390513785,-45.5795179709985,4.20082013374672));
#25138=CARTESIAN_POINT('Ctrl Pts',(9.70137854017372,-45.4045179709985,-1.74689612655491E-11));
#25139=CARTESIAN_POINT('Ctrl Pts',(7.27603390512273,-45.2295179709985,-4.20082013377291));
#25140=CARTESIAN_POINT('Ctrl Pts',(4.85068927007173,-45.0545179709985,-8.40164026752836));
#25141=CARTESIAN_POINT('Ctrl Pts',(-1.51301075899711E-11,-44.8795179709985,
-8.40164026751963));
#25142=CARTESIAN_POINT('Ctrl Pts',(-4.85068927010199,-44.7045179709985,
-8.4016402675109));
#25143=CARTESIAN_POINT('Ctrl Pts',(-7.27603390513785,-44.5295179709985,
-4.20082013374671));
#25144=CARTESIAN_POINT('Ctrl Pts',(-9.70137854017372,-44.3545179709985,
1.74701493417668E-11));
#25145=CARTESIAN_POINT('Ctrl Pts',(-7.27603390512272,-44.1795179709985,
4.20082013377292));
#25146=CARTESIAN_POINT('Ctrl Pts',(-4.85068927007173,-44.0045179709985,
8.40164026752836));
#25147=CARTESIAN_POINT('Ctrl Pts',(1.5129078685785E-11,-43.8295179709985,
8.40164026751963));
#25148=CARTESIAN_POINT('Ctrl Pts',(4.85068927010198,-43.6545179709985,8.4016402675109));
#25149=CARTESIAN_POINT('Ctrl Pts',(7.27603390513785,-43.4795179709985,4.20082013374672));
#25150=CARTESIAN_POINT('Ctrl Pts',(9.70137854017372,-43.3045179709985,-1.74689612655491E-11));
#25151=CARTESIAN_POINT('Ctrl Pts',(7.27603390512273,-43.1295179709985,-4.20082013377291));
#25152=CARTESIAN_POINT('Ctrl Pts',(4.85068927007173,-42.9545179709985,-8.40164026752836));
#25153=CARTESIAN_POINT('Ctrl Pts',(-1.51301075899711E-11,-42.7795179709985,
-8.40164026751963));
#25154=CARTESIAN_POINT('Ctrl Pts',(-4.85068927010199,-42.6045179709985,
-8.4016402675109));
#25155=CARTESIAN_POINT('Ctrl Pts',(-7.27603390513785,-42.4295179709985,
-4.20082013374671));
#25156=CARTESIAN_POINT('Ctrl Pts',(-9.70137854017372,-42.2545179709985,
1.74701493417668E-11));
#25157=CARTESIAN_POINT('Ctrl Pts',(-7.27603390512272,-42.0795179709985,
4.20082013377292));
#25158=CARTESIAN_POINT('Ctrl Pts',(-4.85068927007173,-41.9045179709985,
8.40164026752836));
#25159=CARTESIAN_POINT('Ctrl Pts',(1.5129078685785E-11,-41.7295179709985,
8.40164026751963));
#25160=CARTESIAN_POINT('Ctrl Pts',(4.85068927010198,-41.5545179709985,8.4016402675109));
#25161=CARTESIAN_POINT('Ctrl Pts',(7.27603390513785,-41.3795179709985,4.20082013374672));
#25162=CARTESIAN_POINT('Ctrl Pts',(9.70137854017372,-41.2045179709985,-1.74689612655491E-11));
#25163=CARTESIAN_POINT('Ctrl Pts',(7.27603390512273,-41.0295179709985,-4.20082013377291));
#25164=CARTESIAN_POINT('Ctrl Pts',(4.85068927007173,-40.8545179709985,-8.40164026752836));
#25165=CARTESIAN_POINT('Ctrl Pts',(-1.51301075899711E-11,-40.6795179709985,
-8.40164026751963));
#25166=CARTESIAN_POINT('Ctrl Pts',(-4.85068927010199,-40.5045179709985,
-8.4016402675109));
#25167=CARTESIAN_POINT('Ctrl Pts',(-7.27603390513785,-40.3295179709985,
-4.20082013374671));
#25168=CARTESIAN_POINT('Ctrl Pts',(-9.70137854017372,-40.1545179709985,
1.74701493417668E-11));
#25169=CARTESIAN_POINT('Ctrl Pts',(-7.27603390512272,-39.9795179709985,
4.20082013377292));
#25170=CARTESIAN_POINT('Ctrl Pts',(-4.85068927007173,-39.8045179709985,
8.40164026752836));
#25171=CARTESIAN_POINT('Ctrl Pts',(1.5129078685785E-11,-39.6295179709985,
8.40164026751963));
#25172=CARTESIAN_POINT('Ctrl Pts',(4.85068927010198,-39.4545179709985,8.4016402675109));
#25173=CARTESIAN_POINT('Ctrl Pts',(7.27603390513785,-39.2795179709985,4.20082013374672));
#25174=CARTESIAN_POINT('Ctrl Pts',(9.70137854017372,-39.1045179709985,-1.74689612655491E-11));
#25175=CARTESIAN_POINT('Ctrl Pts',(7.27603390512273,-38.9295179709985,-4.20082013377291));
#25176=CARTESIAN_POINT('Ctrl Pts',(4.85068927007173,-38.7545179709985,-8.40164026752836));
#25177=CARTESIAN_POINT('Ctrl Pts',(-1.51301075899711E-11,-38.5795179709985,
-8.40164026751963));
#25178=CARTESIAN_POINT('Ctrl Pts',(-4.85068927010199,-38.4045179709985,
-8.4016402675109));
#25179=CARTESIAN_POINT('Ctrl Pts',(-7.27603390513785,-38.2295179709985,
-4.20082013374671));
#25180=CARTESIAN_POINT('Ctrl Pts',(-9.70137854017372,-38.0545179709985,
1.74701493417668E-11));
#25181=CARTESIAN_POINT('Ctrl Pts',(-7.27603390512272,-37.8795179709985,
4.20082013377292));
#25182=CARTESIAN_POINT('Ctrl Pts',(-4.85068927007173,-37.7045179709985,
8.40164026752836));
#25183=CARTESIAN_POINT('Ctrl Pts',(1.5129078685785E-11,-37.5295179709985,
8.40164026751963));
#25184=CARTESIAN_POINT('Ctrl Pts',(4.85068927010198,-37.3545179709985,8.4016402675109));
#25185=CARTESIAN_POINT('Ctrl Pts',(7.27603390513785,-37.1795179709985,4.20082013374672));
#25186=CARTESIAN_POINT('Ctrl Pts',(9.70137854017372,-37.0045179709985,-1.74689612655491E-11));
#25187=CARTESIAN_POINT('Ctrl Pts',(7.27603390512273,-36.8295179709985,-4.20082013377291));
#25188=CARTESIAN_POINT('Ctrl Pts',(4.85068927007173,-36.6545179709985,-8.40164026752836));
#25189=CARTESIAN_POINT('Ctrl Pts',(-1.51301075899711E-11,-36.4795179709985,
-8.40164026751963));
#25190=CARTESIAN_POINT('Ctrl Pts',(-4.85068927010199,-36.3045179709985,
-8.4016402675109));
#25191=CARTESIAN_POINT('Ctrl Pts',(-7.27603390513785,-36.1295179709985,
-4.20082013374671));
#25192=CARTESIAN_POINT('Ctrl Pts',(-9.70137854017372,-35.9545179709985,
1.74701493417668E-11));
#25193=CARTESIAN_POINT('Ctrl Pts',(-7.27603390512272,-35.7795179709985,
4.20082013377292));
#25194=CARTESIAN_POINT('Ctrl Pts',(-4.85068927007173,-35.6045179709985,
8.40164026752836));
#25195=CARTESIAN_POINT('Ctrl Pts',(1.5129078685785E-11,-35.4295179709985,
8.40164026751963));
#25196=CARTESIAN_POINT('Ctrl Pts',(4.85068927010198,-35.2545179709985,8.4016402675109));
#25197=CARTESIAN_POINT('Ctrl Pts',(7.27603390513785,-35.0795179709985,4.20082013374672));
#25198=CARTESIAN_POINT('Ctrl Pts',(9.70137854017372,-34.9045179709985,-1.74689612655491E-11));
#25199=CARTESIAN_POINT('Ctrl Pts',(7.27603390512273,-34.7295179709985,-4.20082013377291));
#25200=CARTESIAN_POINT('Ctrl Pts',(4.85068927007173,-34.5545179709985,-8.40164026752836));
#25201=CARTESIAN_POINT('Ctrl Pts',(-1.51301075899711E-11,-34.3795179709985,
-8.40164026751963));
#25202=CARTESIAN_POINT('Ctrl Pts',(-4.85068927010199,-34.2045179709985,
-8.4016402675109));
#25203=CARTESIAN_POINT('Ctrl Pts',(-7.27603390513785,-34.0295179709985,
-4.20082013374671));
#25204=CARTESIAN_POINT('Ctrl Pts',(-9.70137854017372,-33.8545179709985,
1.74701493417668E-11));
#25205=CARTESIAN_POINT('Ctrl Pts',(-7.27603390512272,-33.6795179709985,
4.20082013377292));
#25206=CARTESIAN_POINT('Ctrl Pts',(-4.85068927007173,-33.5045179709985,
8.40164026752836));
#25207=CARTESIAN_POINT('Ctrl Pts',(1.5129078685785E-11,-33.3295179709985,
8.40164026751963));
#25208=CARTESIAN_POINT('Ctrl Pts',(4.85068927010198,-33.1545179709985,8.4016402675109));
#25209=CARTESIAN_POINT('Ctrl Pts',(7.27603390513785,-32.9795179709985,4.20082013374672));
#25210=CARTESIAN_POINT('Ctrl Pts',(9.70137854017372,-32.8045179709985,-1.74689612655491E-11));
#25211=CARTESIAN_POINT('Ctrl Pts',(7.27603390512273,-32.6295179709985,-4.20082013377291));
#25212=CARTESIAN_POINT('Ctrl Pts',(4.85068927007173,-32.4545179709985,-8.40164026752836));
#25213=CARTESIAN_POINT('Ctrl Pts',(-1.51301075899711E-11,-32.2795179709985,
-8.40164026751963));
#25214=CARTESIAN_POINT('Ctrl Pts',(-4.85068927010199,-32.1045179709985,
-8.4016402675109));
#25215=CARTESIAN_POINT('Ctrl Pts',(-7.27603390513785,-31.9295179709985,
-4.20082013374671));
#25216=CARTESIAN_POINT('Ctrl Pts',(-9.70137854017372,-31.7545179709985,
1.74701493417668E-11));
#25217=CARTESIAN_POINT('Ctrl Pts',(-7.27603390512272,-31.5795179709985,
4.20082013377292));
#25218=CARTESIAN_POINT('Ctrl Pts',(-4.85068927007173,-31.4045179709985,
8.40164026752836));
#25219=CARTESIAN_POINT('Ctrl Pts',(1.5129078685785E-11,-31.2295179709985,
8.40164026751963));
#25220=CARTESIAN_POINT('Ctrl Pts',(4.85068927010198,-31.0545179709985,8.4016402675109));
#25221=CARTESIAN_POINT('Ctrl Pts',(7.27603390513785,-30.8795179709985,4.20082013374672));
#25222=CARTESIAN_POINT('Ctrl Pts',(9.70137854017372,-30.7045179709985,-1.74689612655491E-11));
#25223=CARTESIAN_POINT('Ctrl Pts',(7.27603390512273,-30.5295179709985,-4.20082013377291));
#25224=CARTESIAN_POINT('Ctrl Pts',(4.85068927007173,-30.3545179709985,-8.40164026752836));
#25225=CARTESIAN_POINT('Ctrl Pts',(-1.51301075899711E-11,-30.1795179709985,
-8.40164026751963));
#25226=CARTESIAN_POINT('Ctrl Pts',(-4.85068927010199,-30.0045179709985,
-8.4016402675109));
#25227=CARTESIAN_POINT('Ctrl Pts',(-7.27603390513785,-29.8295179709985,
-4.20082013374671));
#25228=CARTESIAN_POINT('Ctrl Pts',(-9.70137854017372,-29.6545179709985,
1.74701493417668E-11));
#25229=CARTESIAN_POINT('Ctrl Pts',(-7.27603390512272,-29.4795179709985,
4.20082013377292));
#25230=CARTESIAN_POINT('Ctrl Pts',(-4.85068927007173,-29.3045179709985,
8.40164026752836));
#25231=CARTESIAN_POINT('Ctrl Pts',(1.5129078685785E-11,-29.1295179709985,
8.40164026751963));
#25232=CARTESIAN_POINT('Ctrl Pts',(4.85068927010198,-28.9545179709986,8.4016402675109));
#25233=CARTESIAN_POINT('Ctrl Pts',(7.27603390513785,-28.7795179709985,4.20082013374672));
#25234=CARTESIAN_POINT('Ctrl Pts',(9.70137854017372,-28.6045179709986,-1.74689612655491E-11));
#25235=CARTESIAN_POINT('Ctrl Pts',(7.27603390512273,-28.4295179709985,-4.20082013377291));
#25236=CARTESIAN_POINT('Ctrl Pts',(4.85068927007173,-28.2545179709985,-8.40164026752836));
#25237=CARTESIAN_POINT('Ctrl Pts',(-1.51301075899711E-11,-28.0795179709985,
-8.40164026751963));
#25238=CARTESIAN_POINT('Ctrl Pts',(-4.85068927010199,-27.9045179709985,
-8.4016402675109));
#25239=CARTESIAN_POINT('Ctrl Pts',(-7.27603390513785,-27.7295179709985,
-4.20082013374671));
#25240=CARTESIAN_POINT('Ctrl Pts',(-9.70137854017372,-27.5545179709986,
1.74701493417668E-11));
#25241=CARTESIAN_POINT('Ctrl Pts',(-7.27603390512272,-27.3795179709985,
4.20082013377292));
#25242=CARTESIAN_POINT('Ctrl Pts',(-4.85068927007173,-27.2045179709986,
8.40164026752836));
#25243=CARTESIAN_POINT('Ctrl Pts',(1.5129078685785E-11,-27.0295179709986,
8.40164026751963));
#25244=CARTESIAN_POINT('Ctrl Pts',(4.85068927010198,-26.8545179709985,8.4016402675109));
#25245=CARTESIAN_POINT('Ctrl Pts',(7.27603390513785,-26.6795179709985,4.20082013374672));
#25246=CARTESIAN_POINT('Ctrl Pts',(9.70137854017372,-26.5045179709986,-1.74689612655491E-11));
#25247=CARTESIAN_POINT('Ctrl Pts',(7.27603390512273,-26.3295179709985,-4.20082013377291));
#25248=CARTESIAN_POINT('Ctrl Pts',(4.85068927007173,-26.1545179709986,-8.40164026752836));
#25249=CARTESIAN_POINT('Ctrl Pts',(-1.51301075899711E-11,-25.9795179709985,
-8.40164026751963));
#25250=CARTESIAN_POINT('Ctrl Pts',(-4.85068927010199,-25.8045179709985,
-8.4016402675109));
#25251=CARTESIAN_POINT('Ctrl Pts',(-7.27603390513785,-25.6295179709985,
-4.20082013374671));
#25252=CARTESIAN_POINT('Ctrl Pts',(-9.70137854017372,-25.4545179709985,
1.74701493417668E-11));
#25253=CARTESIAN_POINT('Ctrl Pts',(-7.27603390512272,-25.2795179709985,
4.20082013377292));
#25254=CARTESIAN_POINT('Ctrl Pts',(-4.85068927007173,-25.1045179709986,
8.40164026752836));
#25255=CARTESIAN_POINT('Ctrl Pts',(1.5129078685785E-11,-24.9295179709985,
8.40164026751963));
#25256=CARTESIAN_POINT('Ctrl Pts',(4.85068927010198,-24.7545179709985,8.4016402675109));
#25257=CARTESIAN_POINT('Ctrl Pts',(7.27603390513785,-24.5795179709986,4.20082013374672));
#25258=CARTESIAN_POINT('Ctrl Pts',(9.70137854017372,-24.4045179709986,-1.74689612655491E-11));
#25259=CARTESIAN_POINT('Ctrl Pts',(7.27603390512273,-24.2295179709986,-4.20082013377291));
#25260=CARTESIAN_POINT('Ctrl Pts',(4.85068927007173,-24.0545179709986,-8.40164026752836));
#25261=CARTESIAN_POINT('Ctrl Pts',(-1.51301075899711E-11,-23.8795179709986,
-8.40164026751963));
#25262=CARTESIAN_POINT('Ctrl Pts',(-4.85068927010199,-23.7045179709986,
-8.4016402675109));
#25263=CARTESIAN_POINT('Ctrl Pts',(-7.27603390513785,-23.5295179709985,
-4.20082013374671));
#25264=CARTESIAN_POINT('Ctrl Pts',(-9.70137854017372,-23.3545179709986,
1.74701493417668E-11));
#25265=CARTESIAN_POINT('Ctrl Pts',(-7.27603390512272,-23.1795179709986,
4.20082013377292));
#25266=CARTESIAN_POINT('Ctrl Pts',(-4.85068927007173,-23.0045179709986,
8.40164026752836));
#25267=CARTESIAN_POINT('Ctrl Pts',(1.5129078685785E-11,-22.8295179709986,
8.40164026751963));
#25268=CARTESIAN_POINT('Ctrl Pts',(4.85068927010198,-22.6545179709986,8.4016402675109));
#25269=CARTESIAN_POINT('Ctrl Pts',(7.27603390513785,-22.4795179709986,4.20082013374672));
#25270=CARTESIAN_POINT('Ctrl Pts',(9.70137854017372,-22.3045179709986,-1.74689612655491E-11));
#25271=CARTESIAN_POINT('Ctrl Pts',(7.27603390512273,-22.1295179709986,-4.20082013377291));
#25272=CARTESIAN_POINT('Ctrl Pts',(4.85068927007173,-21.9545179709986,-8.40164026752836));
#25273=CARTESIAN_POINT('Ctrl Pts',(-1.51301075899711E-11,-21.7795179709986,
-8.40164026751963));
#25274=CARTESIAN_POINT('Ctrl Pts',(-4.85068927010199,-21.6045179709986,
-8.4016402675109));
#25275=CARTESIAN_POINT('Ctrl Pts',(-7.27603390513785,-21.4295179709986,
-4.20082013374671));
#25276=CARTESIAN_POINT('Ctrl Pts',(-9.70137854017372,-21.2545179709986,
1.74701493417668E-11));
#25277=CARTESIAN_POINT('Ctrl Pts',(-7.27603390512272,-21.0795179709986,
4.20082013377292));
#25278=CARTESIAN_POINT('Ctrl Pts',(-4.85068927007173,-20.9045179709986,
8.40164026752836));
#25279=CARTESIAN_POINT('Ctrl Pts',(1.5129078685785E-11,-20.7295179709986,
8.40164026751963));
#25280=CARTESIAN_POINT('Ctrl Pts',(4.85068927010198,-20.5545179709986,8.4016402675109));
#25281=CARTESIAN_POINT('Ctrl Pts',(7.27603390513785,-20.3795179709986,4.20082013374672));
#25282=CARTESIAN_POINT('Ctrl Pts',(9.70137854017372,-20.2045179709986,-1.74689612655491E-11));
#25283=CARTESIAN_POINT('Ctrl Pts',(7.27603390512273,-20.0295179709986,-4.20082013377291));
#25284=CARTESIAN_POINT('Ctrl Pts',(4.85068927007173,-19.8545179709986,-8.40164026752836));
#25285=CARTESIAN_POINT('Ctrl Pts',(-1.51301075899711E-11,-19.6795179709986,
-8.40164026751963));
#25286=CARTESIAN_POINT('Ctrl Pts',(-4.85068927010199,-19.5045179709986,
-8.4016402675109));
#25287=CARTESIAN_POINT('Ctrl Pts',(-7.27603390513785,-19.3295179709986,
-4.20082013374671));
#25288=CARTESIAN_POINT('Ctrl Pts',(-9.70137854017372,-19.1545179709986,
1.74701493417668E-11));
#25289=CARTESIAN_POINT('Ctrl Pts',(-7.27603390512272,-18.9795179709986,
4.20082013377292));
#25290=CARTESIAN_POINT('Ctrl Pts',(-4.85068927007173,-18.8045179709986,
8.40164026752836));
#25291=CARTESIAN_POINT('Ctrl Pts',(1.5129078685785E-11,-18.6295179709986,
8.40164026751963));
#25292=CARTESIAN_POINT('Ctrl Pts',(4.85068927010198,-18.4545179709986,8.4016402675109));
#25293=CARTESIAN_POINT('Ctrl Pts',(7.27603390513785,-18.2795179709986,4.20082013374672));
#25294=CARTESIAN_POINT('Ctrl Pts',(9.70137854017372,-18.1045179709986,-1.74689612655491E-11));
#25295=CARTESIAN_POINT('Ctrl Pts',(7.27603390512273,-17.9295179709986,-4.20082013377291));
#25296=CARTESIAN_POINT('Ctrl Pts',(4.85068927007173,-17.7545179709986,-8.40164026752836));
#25297=CARTESIAN_POINT('Ctrl Pts',(-1.51301075899711E-11,-17.5795179709986,
-8.40164026751963));
#25298=CARTESIAN_POINT('Ctrl Pts',(-4.85068927010199,-17.4045179709986,
-8.4016402675109));
#25299=CARTESIAN_POINT('Ctrl Pts',(-7.27603390513785,-17.2295179709986,
-4.20082013374671));
#25300=CARTESIAN_POINT('Ctrl Pts',(-9.70137854017372,-17.0545179709986,
1.74701493417668E-11));
#25301=CARTESIAN_POINT('Ctrl Pts',(-7.27603390512272,-16.8795179709986,
4.20082013377292));
#25302=CARTESIAN_POINT('Ctrl Pts',(-4.85068927007173,-16.7045179709986,
8.40164026752836));
#25303=CARTESIAN_POINT('Ctrl Pts',(1.5129078685785E-11,-16.5295179709986,
8.40164026751963));
#25304=CARTESIAN_POINT('Ctrl Pts',(4.85068927010198,-16.3545179709986,8.4016402675109));
#25305=CARTESIAN_POINT('Ctrl Pts',(7.27603390513785,-16.1795179709986,4.20082013374672));
#25306=CARTESIAN_POINT('Ctrl Pts',(9.70137854017372,-16.0045179709986,-1.74689612655491E-11));
#25307=CARTESIAN_POINT('Ctrl Pts',(7.27603390512273,-15.8295179709986,-4.20082013377291));
#25308=CARTESIAN_POINT('Ctrl Pts',(4.85068927007173,-15.6545179709986,-8.40164026752836));
#25309=CARTESIAN_POINT('Ctrl Pts',(-1.51301075899711E-11,-15.4795179709986,
-8.40164026751963));
#25310=CARTESIAN_POINT('Ctrl Pts',(-4.85068927010199,-15.3045179709986,
-8.4016402675109));
#25311=CARTESIAN_POINT('Ctrl Pts',(-7.27603390513785,-15.1295179709986,
-4.20082013374671));
#25312=CARTESIAN_POINT('Ctrl Pts',(-9.70137854017372,-14.9545179709986,
1.74701493417668E-11));
#25313=CARTESIAN_POINT('Ctrl Pts',(-7.27603390512272,-14.7795179709986,
4.20082013377292));
#25314=CARTESIAN_POINT('Ctrl Pts',(-4.85068927007173,-14.6045179709986,
8.40164026752836));
#25315=CARTESIAN_POINT('Ctrl Pts',(1.5129078685785E-11,-14.4295179709986,
8.40164026751963));
#25316=CARTESIAN_POINT('Ctrl Pts',(4.85068927010198,-14.2545179709986,8.4016402675109));
#25317=CARTESIAN_POINT('Ctrl Pts',(7.27603390513785,-14.0795179709986,4.20082013374672));
#25318=CARTESIAN_POINT('Ctrl Pts',(9.70137854017372,-13.9045179709986,-1.74689612655491E-11));
#25319=CARTESIAN_POINT('Ctrl Pts',(7.27603390512273,-13.7295179709986,-4.20082013377291));
#25320=CARTESIAN_POINT('Ctrl Pts',(4.85068927007173,-13.5545179709986,-8.40164026752836));
#25321=CARTESIAN_POINT('Ctrl Pts',(-1.51301075899711E-11,-13.3795179709986,
-8.40164026751963));
#25322=CARTESIAN_POINT('Ctrl Pts',(-4.85068927010199,-13.2045179709986,
-8.4016402675109));
#25323=CARTESIAN_POINT('Ctrl Pts',(-7.27603390513785,-13.0295179709986,
-4.20082013374671));
#25324=CARTESIAN_POINT('Ctrl Pts',(-9.70137854017372,-12.8545179709986,
1.74701493417668E-11));
#25325=CARTESIAN_POINT('Ctrl Pts',(-7.27603390512272,-12.6795179709986,
4.20082013377292));
#25326=CARTESIAN_POINT('Ctrl Pts',(-4.85068927007173,-12.5045179709986,
8.40164026752836));
#25327=CARTESIAN_POINT('Ctrl Pts',(1.5129078685785E-11,-12.3295179709986,
8.40164026751963));
#25328=CARTESIAN_POINT('Ctrl Pts',(4.85068927010198,-12.1545179709986,8.4016402675109));
#25329=CARTESIAN_POINT('Ctrl Pts',(7.27603390513785,-11.9795179709986,4.20082013374672));
#25330=CARTESIAN_POINT('Ctrl Pts',(9.70137854017372,-11.8045179709986,-1.74689612655491E-11));
#25331=CARTESIAN_POINT('Ctrl Pts',(7.27603390512273,-11.6295179709986,-4.20082013377291));
#25332=CARTESIAN_POINT('Ctrl Pts',(4.85068927007173,-11.4545179709986,-8.40164026752836));
#25333=CARTESIAN_POINT('Ctrl Pts',(-1.51301075899711E-11,-11.2795179709986,
-8.40164026751963));
#25334=CARTESIAN_POINT('Ctrl Pts',(-4.85068927010199,-11.1045179709986,
-8.4016402675109));
#25335=CARTESIAN_POINT('Ctrl Pts',(-7.27603390513785,-10.9295179709986,
-4.20082013374671));
#25336=CARTESIAN_POINT('Ctrl Pts',(-9.70137854017372,-10.7545179709986,
1.74701493417668E-11));
#25337=CARTESIAN_POINT('Ctrl Pts',(-7.27603390512272,-10.5795179709986,
4.20082013377292));
#25338=CARTESIAN_POINT('Ctrl Pts',(-4.85068927007173,-10.4045179709986,
8.40164026752836));
#25339=CARTESIAN_POINT('Ctrl Pts',(1.5129078685785E-11,-10.2295179709986,
8.40164026751963));
#25340=CARTESIAN_POINT('Ctrl Pts',(4.85068927010198,-10.0545179709986,8.4016402675109));
#25341=CARTESIAN_POINT('Ctrl Pts',(7.27603390513785,-9.87951797099859,4.20082013374672));
#25342=CARTESIAN_POINT('Ctrl Pts',(9.70137854017372,-9.70451797099858,-1.74689612655491E-11));
#25343=CARTESIAN_POINT('Ctrl Pts',(7.27603390512273,-9.52951797099857,-4.20082013377291));
#25344=CARTESIAN_POINT('Ctrl Pts',(4.85068927007173,-9.3545179709986,-8.40164026752836));
#25345=CARTESIAN_POINT('Ctrl Pts',(-1.51301075899711E-11,-9.17951797099859,
-8.40164026751963));
#25346=CARTESIAN_POINT('Ctrl Pts',(-4.85068927010199,-9.00451797099858,
-8.4016402675109));
#25347=CARTESIAN_POINT('Ctrl Pts',(-7.27603390513785,-8.8295179709986,-4.20082013374671));
#25348=CARTESIAN_POINT('Ctrl Pts',(-9.70137854017372,-8.65451797099859,
1.74701493417668E-11));
#25349=CARTESIAN_POINT('Ctrl Pts',(-7.27603390512272,-8.47951797099858,
4.20082013377292));
#25350=CARTESIAN_POINT('Ctrl Pts',(-4.85068927007173,-8.3045179709986,8.40164026752836));
#25351=CARTESIAN_POINT('Ctrl Pts',(1.5129078685785E-11,-8.12951797099859,
8.40164026751963));
#25352=CARTESIAN_POINT('Ctrl Pts',(4.85068927010198,-7.95451797099859,8.4016402675109));
#25353=CARTESIAN_POINT('Ctrl Pts',(7.27603390513785,-7.7795179709986,4.20082013374672));
#25354=CARTESIAN_POINT('Ctrl Pts',(9.70137854017372,-7.60451797099859,-1.74689612655491E-11));
#25355=CARTESIAN_POINT('Ctrl Pts',(7.27603390512273,-7.42951797099858,-4.20082013377291));
#25356=CARTESIAN_POINT('Ctrl Pts',(4.85068927007173,-7.25451797099861,-8.40164026752836));
#25357=CARTESIAN_POINT('Ctrl Pts',(-1.51301075899711E-11,-7.07951797099859,
-8.40164026751963));
#25358=CARTESIAN_POINT('Ctrl Pts',(-4.85068927010199,-6.90451797099859,
-8.4016402675109));
#25359=CARTESIAN_POINT('Ctrl Pts',(-7.27603390513785,-6.72951797099858,
-4.20082013374671));
#25360=CARTESIAN_POINT('Ctrl Pts',(-9.70137854017372,-6.5545179709986,1.74701493417668E-11));
#25361=CARTESIAN_POINT('Ctrl Pts',(-7.27603390512272,-6.37951797099859,
4.20082013377292));
#25362=CARTESIAN_POINT('Ctrl Pts',(-4.85068927007173,-6.20451797099858,
8.40164026752836));
#25363=CARTESIAN_POINT('Ctrl Pts',(1.5129078685785E-11,-6.0295179709986,
8.40164026751963));
#25364=CARTESIAN_POINT('Ctrl Pts',(4.85068927010198,-5.8545179709986,8.4016402675109));
#25365=CARTESIAN_POINT('Ctrl Pts',(7.27603390513785,-5.67951797099858,4.20082013374672));
#25366=CARTESIAN_POINT('Ctrl Pts',(9.70137854017372,-5.5045179709986,-1.74689612655491E-11));
#25367=CARTESIAN_POINT('Ctrl Pts',(7.27603390512273,-5.32951797099859,-4.20082013377291));
#25368=CARTESIAN_POINT('Ctrl Pts',(4.85068927007173,-5.15451797099859,-8.40164026752836));
#25369=CARTESIAN_POINT('Ctrl Pts',(-1.51301075899711E-11,-4.9795179709986,
-8.40164026751963));
#25370=CARTESIAN_POINT('Ctrl Pts',(-4.85068927010199,-4.8045179709986,-8.4016402675109));
#25371=CARTESIAN_POINT('Ctrl Pts',(-7.27603390513785,-4.62951797099859,
-4.20082013374671));
#25372=CARTESIAN_POINT('Ctrl Pts',(-9.70137854017372,-4.45451797099861,
1.74701493417668E-11));
#25373=CARTESIAN_POINT('Ctrl Pts',(-7.27603390512272,-4.2795179709986,4.20082013377292));
#25374=CARTESIAN_POINT('Ctrl Pts',(-4.85068927007173,-4.10451797099859,
8.40164026752836));
#25375=CARTESIAN_POINT('Ctrl Pts',(1.5129078685785E-11,-3.92951797099861,
8.40164026751963));
#25376=CARTESIAN_POINT('Ctrl Pts',(4.85068927010198,-3.75451797099861,8.4016402675109));
#25377=CARTESIAN_POINT('Ctrl Pts',(7.27603390513785,-3.57951797099859,4.20082013374672));
#25378=CARTESIAN_POINT('Ctrl Pts',(9.70137854017372,-3.40451797099861,-1.74689612655491E-11));
#25379=CARTESIAN_POINT('Ctrl Pts',(7.27603390512273,-3.2295179709986,-4.20082013377291));
#25380=CARTESIAN_POINT('Ctrl Pts',(4.85068927007173,-3.0545179709986,-8.40164026752836));
#25381=CARTESIAN_POINT('Ctrl Pts',(-1.51301075899711E-11,-2.87951797099861,
-8.40164026751963));
#25382=CARTESIAN_POINT('Ctrl Pts',(-4.85068927010199,-2.70451797099861,
-8.4016402675109));
#25383=CARTESIAN_POINT('Ctrl Pts',(-7.27603390513785,-2.5295179709986,-4.20082013374671));
#25384=CARTESIAN_POINT('Ctrl Pts',(-9.70137854017372,-2.3545179709986,1.74701493417668E-11));
#25385=CARTESIAN_POINT('Ctrl Pts',(-7.27603390512272,-2.17951797099861,
4.20082013377292));
#25386=CARTESIAN_POINT('Ctrl Pts',(-4.85068927007173,-2.0045179709986,8.40164026752836));
#25387=CARTESIAN_POINT('Ctrl Pts',(1.5129078685785E-11,-1.82951797099859,
8.40164026751963));
#25388=CARTESIAN_POINT('Ctrl Pts',(4.85068927010198,-1.65451797099861,8.4016402675109));
#25389=CARTESIAN_POINT('Ctrl Pts',(7.27603390513785,-1.4795179709986,4.20082013374672));
#25390=CARTESIAN_POINT('Ctrl Pts',(9.70137854017372,-1.3045179709986,-1.74689612655491E-11));
#25391=CARTESIAN_POINT('Ctrl Pts',(7.27603390512273,-1.12951797099861,-4.20082013377291));
#25392=CARTESIAN_POINT('Ctrl Pts',(4.85068927007173,-0.954517970998605,
-8.40164026752836));
#25393=CARTESIAN_POINT('Ctrl Pts',(-1.51301075899711E-11,-0.779517970998594,
-8.40164026751963));
#25394=CARTESIAN_POINT('Ctrl Pts',(-4.85068927010199,-0.604517970998614,
-8.4016402675109));
#25395=CARTESIAN_POINT('Ctrl Pts',(-7.27603390513785,-0.429517970998605,
-4.20082013374671));
#25396=CARTESIAN_POINT('Ctrl Pts',(-9.70137854017372,-0.2545179709986,1.74701493417668E-11));
#25397=CARTESIAN_POINT('Ctrl Pts',(-7.27603390512272,-0.079517970998616,
4.20082013377292));
#25398=CARTESIAN_POINT('Ctrl Pts',(-4.85068927007173,0.0954820290013905,
8.40164026752836));
#25399=CARTESIAN_POINT('Ctrl Pts',(1.5129078685785E-11,0.270482029001401,
8.40164026751963));
#25400=CARTESIAN_POINT('Ctrl Pts',(4.85068927010198,0.445482029001381,8.4016402675109));
#25401=CARTESIAN_POINT('Ctrl Pts',(7.27603390513785,0.62048202900139,4.20082013374672));
#25402=CARTESIAN_POINT('Ctrl Pts',(9.70137854017372,0.795482029001395,-1.74689612655491E-11));
#25403=CARTESIAN_POINT('Ctrl Pts',(7.27603390512273,0.970482029001379,-4.20082013377291));
#25404=CARTESIAN_POINT('Ctrl Pts',(4.85068927007173,1.14548202900139,-8.40164026752836));
#25405=CARTESIAN_POINT('Ctrl Pts',(-1.51301075899711E-11,1.3204820290014,
-8.40164026751963));
#25406=CARTESIAN_POINT('Ctrl Pts',(-4.85068927010199,1.49548202900138,-8.4016402675109));
#25407=CARTESIAN_POINT('Ctrl Pts',(-7.27603390513785,1.67048202900139,-4.20082013374671));
#25408=CARTESIAN_POINT('Ctrl Pts',(-9.70137854017372,1.84548202900139,1.74701493417668E-11));
#25409=CARTESIAN_POINT('Ctrl Pts',(-7.27603390512272,2.0204820290014,4.20082013377292));
#25410=CARTESIAN_POINT('Ctrl Pts',(-4.85068927007173,2.19548202900138,8.40164026752836));
#25411=CARTESIAN_POINT('Ctrl Pts',(1.5129078685785E-11,2.37048202900139,
8.40164026751963));
#25412=CARTESIAN_POINT('Ctrl Pts',(4.85068927010198,2.5454820290014,8.4016402675109));
#25413=CARTESIAN_POINT('Ctrl Pts',(7.27603390513785,2.72048202900138,4.20082013374672));
#25414=CARTESIAN_POINT('Ctrl Pts',(9.70137854017372,2.89548202900139,-1.74689612655491E-11));
#25415=CARTESIAN_POINT('Ctrl Pts',(7.27603390512273,3.0704820290014,-4.20082013377291));
#25416=CARTESIAN_POINT('Ctrl Pts',(4.85068927007173,3.24548202900138,-8.40164026752836));
#25417=CARTESIAN_POINT('Ctrl Pts',(-1.51301075899711E-11,3.42048202900139,
-8.40164026751963));
#25418=CARTESIAN_POINT('Ctrl Pts',(-4.85068927010199,3.59548202900139,-8.4016402675109));
#25419=CARTESIAN_POINT('Ctrl Pts',(-7.27603390513785,3.77048202900138,-4.20082013374671));
#25420=CARTESIAN_POINT('Ctrl Pts',(-9.70137854017372,3.94548202900138,1.74701493417668E-11));
#25421=CARTESIAN_POINT('Ctrl Pts',(-7.27603390512272,4.12048202900139,4.20082013377292));
#25422=CARTESIAN_POINT('Ctrl Pts',(-4.85068927007173,4.29548202900137,8.40164026752836));
#25423=CARTESIAN_POINT('Ctrl Pts',(1.5129078685785E-11,4.47048202900138,
8.40164026751963));
#25424=CARTESIAN_POINT('Ctrl Pts',(4.85068927010198,4.64548202900139,8.4016402675109));
#25425=CARTESIAN_POINT('Ctrl Pts',(7.27603390513785,4.82048202900137,4.20082013374672));
#25426=CARTESIAN_POINT('Ctrl Pts',(9.70137854017372,4.99548202900138,-1.74689612655491E-11));
#25427=CARTESIAN_POINT('Ctrl Pts',(7.27603390512273,5.17048202900139,-4.20082013377291));
#25428=CARTESIAN_POINT('Ctrl Pts',(4.85068927007173,5.34548202900137,-8.40164026752836));
#25429=CARTESIAN_POINT('Ctrl Pts',(-1.51301075899711E-11,5.52048202900138,
-8.40164026751963));
#25430=CARTESIAN_POINT('Ctrl Pts',(-4.85068927010199,5.69548202900138,-8.4016402675109));
#25431=CARTESIAN_POINT('Ctrl Pts',(-7.27603390513785,5.87048202900137,-4.20082013374671));
#25432=CARTESIAN_POINT('Ctrl Pts',(-9.70137854017372,6.04548202900137,1.74701493417668E-11));
#25433=CARTESIAN_POINT('Ctrl Pts',(-7.27603390512272,6.22048202900138,4.20082013377292));
#25434=CARTESIAN_POINT('Ctrl Pts',(-4.85068927007173,6.39548202900136,8.40164026752836));
#25435=CARTESIAN_POINT('Ctrl Pts',(1.5129078685785E-11,6.57048202900137,
8.40164026751963));
#25436=CARTESIAN_POINT('Ctrl Pts',(4.85068927010198,6.74548202900138,8.4016402675109));
#25437=CARTESIAN_POINT('Ctrl Pts',(7.27603390513785,6.92048202900139,4.20082013374672));
#25438=CARTESIAN_POINT('Ctrl Pts',(9.70137854017372,7.09548202900137,-1.74689612655491E-11));
#25439=CARTESIAN_POINT('Ctrl Pts',(7.27603390512273,7.27048202900138,-4.20082013377291));
#25440=CARTESIAN_POINT('Ctrl Pts',(4.85068927007173,7.44548202900138,-8.40164026752836));
#25441=CARTESIAN_POINT('Ctrl Pts',(-1.51301075899711E-11,7.62048202900137,
-8.40164026751963));
#25442=CARTESIAN_POINT('Ctrl Pts',(-4.85068927010199,7.79548202900137,-8.4016402675109));
#25443=CARTESIAN_POINT('Ctrl Pts',(-7.27603390513785,7.97048202900139,-4.20082013374671));
#25444=CARTESIAN_POINT('Ctrl Pts',(-9.70137854017372,8.14548202900136,1.74701493417668E-11));
#25445=CARTESIAN_POINT('Ctrl Pts',(-7.27603390512272,8.32048202900138,4.20082013377292));
#25446=CARTESIAN_POINT('Ctrl Pts',(-4.85068927007173,8.49548202900138,8.40164026752836));
#25447=CARTESIAN_POINT('Ctrl Pts',(1.5129078685785E-11,8.67048202900136,
8.40164026751963));
#25448=CARTESIAN_POINT('Ctrl Pts',(4.85068927010198,8.84548202900137,8.4016402675109));
#25449=CARTESIAN_POINT('Ctrl Pts',(7.27603390513785,9.02048202900138,4.20082013374672));
#25450=CARTESIAN_POINT('Ctrl Pts',(9.70137854017372,9.19548202900136,-1.74689612655491E-11));
#25451=CARTESIAN_POINT('Ctrl Pts',(7.27603390512273,9.37048202900137,-4.20082013377291));
#25452=CARTESIAN_POINT('Ctrl Pts',(4.85068927007173,9.54548202900137,-8.40164026752836));
#25453=CARTESIAN_POINT('Ctrl Pts',(-1.51301075899711E-11,9.72048202900136,
-8.40164026751963));
#25454=CARTESIAN_POINT('Ctrl Pts',(-4.85068927010199,9.89548202900136,-8.4016402675109));
#25455=CARTESIAN_POINT('Ctrl Pts',(-7.27603390513785,10.0704820290014,-4.20082013374671));
#25456=CARTESIAN_POINT('Ctrl Pts',(-9.70137854017372,10.2454820290014,1.74701493417668E-11));
#25457=CARTESIAN_POINT('Ctrl Pts',(-7.27603390512272,10.4204820290014,4.20082013377292));
#25458=CARTESIAN_POINT('Ctrl Pts',(-4.85068927007173,10.5954820290014,8.40164026752836));
#25459=CARTESIAN_POINT('Ctrl Pts',(1.5129078685785E-11,10.7704820290014,
8.40164026751963));
#25460=CARTESIAN_POINT('Ctrl Pts',(4.85068927010198,10.9454820290014,8.4016402675109));
#25461=CARTESIAN_POINT('Ctrl Pts',(7.27603390513785,11.1204820290014,4.20082013374672));
#25462=CARTESIAN_POINT('Ctrl Pts',(9.70137854017372,11.2954820290014,-1.74689612655491E-11));
#25463=CARTESIAN_POINT('Ctrl Pts',(7.27603390512273,11.4704820290014,-4.20082013377291));
#25464=CARTESIAN_POINT('Ctrl Pts',(4.85068927007173,11.6454820290014,-8.40164026752836));
#25465=CARTESIAN_POINT('Ctrl Pts',(-1.51301075899711E-11,11.8204820290014,
-8.40164026751963));
#25466=CARTESIAN_POINT('Ctrl Pts',(-4.85068927010199,11.9954820290014,-8.4016402675109));
#25467=CARTESIAN_POINT('Ctrl Pts',(-7.27603390513785,12.1704820290014,-4.20082013374671));
#25468=CARTESIAN_POINT('Ctrl Pts',(-9.70137854017372,12.3454820290014,1.74701493417668E-11));
#25469=CARTESIAN_POINT('Ctrl Pts',(-7.27603390512272,12.5204820290014,4.20082013377292));
#25470=CARTESIAN_POINT('Ctrl Pts',(-4.85068927007173,12.6954820290014,8.40164026752836));
#25471=CARTESIAN_POINT('Ctrl Pts',(1.5129078685785E-11,12.8704820290014,
8.40164026751963));
#25472=CARTESIAN_POINT('Ctrl Pts',(4.85068927010198,13.0454820290013,8.4016402675109));
#25473=CARTESIAN_POINT('Ctrl Pts',(7.27603390513785,13.2204820290014,4.20082013374672));
#25474=CARTESIAN_POINT('Ctrl Pts',(9.70137854017372,13.3954820290014,-1.74689612655491E-11));
#25475=CARTESIAN_POINT('Ctrl Pts',(7.27603390512273,13.5704820290014,-4.20082013377291));
#25476=CARTESIAN_POINT('Ctrl Pts',(4.85068927007173,13.7454820290014,-8.40164026752836));
#25477=CARTESIAN_POINT('Ctrl Pts',(-1.51301075899711E-11,13.9204820290014,
-8.40164026751963));
#25478=CARTESIAN_POINT('Ctrl Pts',(-4.85068927010199,14.0954820290013,-8.4016402675109));
#25479=CARTESIAN_POINT('Ctrl Pts',(-7.27603390513785,14.2704820290014,-4.20082013374671));
#25480=CARTESIAN_POINT('Ctrl Pts',(-9.70137854017372,14.4454820290014,1.74701493417668E-11));
#25481=CARTESIAN_POINT('Ctrl Pts',(-7.27603390512272,14.6204820290013,4.20082013377292));
#25482=CARTESIAN_POINT('Ctrl Pts',(-4.85068927007173,14.7954820290014,8.40164026752836));
#25483=CARTESIAN_POINT('Ctrl Pts',(1.5129078685785E-11,14.9704820290014,
8.40164026751963));
#25484=CARTESIAN_POINT('Ctrl Pts',(4.85068927010198,15.1454820290013,8.4016402675109));
#25485=CARTESIAN_POINT('Ctrl Pts',(7.27603390513785,15.3204820290014,4.20082013374672));
#25486=CARTESIAN_POINT('Ctrl Pts',(9.70137854017372,15.4954820290014,-1.74689612655491E-11));
#25487=CARTESIAN_POINT('Ctrl Pts',(7.27603390512273,15.6704820290014,-4.20082013377291));
#25488=CARTESIAN_POINT('Ctrl Pts',(4.85068927007173,15.8454820290013,-8.40164026752836));
#25489=CARTESIAN_POINT('Ctrl Pts',(-1.51301075899711E-11,16.0204820290014,
-8.40164026751963));
#25490=CARTESIAN_POINT('Ctrl Pts',(-4.85068927010199,16.1954820290014,-8.4016402675109));
#25491=CARTESIAN_POINT('Ctrl Pts',(-7.27603390513785,16.3704820290014,-4.20082013374671));
#25492=CARTESIAN_POINT('Ctrl Pts',(-9.70137854017372,16.5454820290013,1.74701493417668E-11));
#25493=CARTESIAN_POINT('Ctrl Pts',(-7.27603390512272,16.7204820290014,4.20082013377292));
#25494=CARTESIAN_POINT('Ctrl Pts',(-4.85068927007173,16.8954820290013,8.40164026752836));
#25495=CARTESIAN_POINT('Ctrl Pts',(1.5129078685785E-11,17.0704820290014,
8.40164026751963));
#25496=CARTESIAN_POINT('Ctrl Pts',(4.85068927010198,17.2454820290014,8.4016402675109));
#25497=CARTESIAN_POINT('Ctrl Pts',(7.27603390513785,17.4204820290013,4.20082013374672));
#25498=CARTESIAN_POINT('Ctrl Pts',(9.70137854017372,17.5954820290013,-1.74689612655491E-11));
#25499=CARTESIAN_POINT('Ctrl Pts',(7.27603390512273,17.7704820290014,-4.20082013377291));
#25500=CARTESIAN_POINT('Ctrl Pts',(4.85068927007173,17.9454820290013,-8.40164026752836));
#25501=CARTESIAN_POINT('Ctrl Pts',(-1.51301075899711E-11,18.1204820290014,
-8.40164026751963));
#25502=CARTESIAN_POINT('Ctrl Pts',(-4.85068927010199,18.2954820290014,-8.4016402675109));
#25503=CARTESIAN_POINT('Ctrl Pts',(-7.27603390513785,18.4704820290013,-4.20082013374671));
#25504=CARTESIAN_POINT('Ctrl Pts',(-9.70137854017372,18.6454820290013,1.74701493417668E-11));
#25505=CARTESIAN_POINT('Ctrl Pts',(-7.27603390512272,18.8204820290014,4.20082013377292));
#25506=CARTESIAN_POINT('Ctrl Pts',(-4.85068927007173,18.9954820290013,8.40164026752836));
#25507=CARTESIAN_POINT('Ctrl Pts',(1.5129078685785E-11,19.1704820290013,
8.40164026751963));
#25508=CARTESIAN_POINT('Ctrl Pts',(4.85068927010198,19.3454820290014,8.4016402675109));
#25509=CARTESIAN_POINT('Ctrl Pts',(7.27603390513785,19.5204820290013,4.20082013374672));
#25510=CARTESIAN_POINT('Ctrl Pts',(9.70137854017372,19.6954820290013,-1.74689612655491E-11));
#25511=CARTESIAN_POINT('Ctrl Pts',(7.27603390512273,19.8704820290014,-4.20082013377291));
#25512=CARTESIAN_POINT('Ctrl Pts',(4.85068927007173,20.0454820290014,-8.40164026752836));
#25513=CARTESIAN_POINT('Ctrl Pts',(-1.51301075899711E-11,20.2204820290013,
-8.40164026751963));
#25514=CARTESIAN_POINT('Ctrl Pts',(-4.85068927010199,20.3954820290014,-8.4016402675109));
#25515=CARTESIAN_POINT('Ctrl Pts',(-7.27603390513785,20.5704820290014,-4.20082013374671));
#25516=CARTESIAN_POINT('Ctrl Pts',(-9.70137854017372,20.7454820290013,1.74701493417668E-11));
#25517=CARTESIAN_POINT('Ctrl Pts',(-7.27603390512272,20.9204820290013,4.20082013377292));
#25518=CARTESIAN_POINT('Ctrl Pts',(-4.85068927007173,21.0954820290014,8.40164026752836));
#25519=CARTESIAN_POINT('Ctrl Pts',(1.5129078685785E-11,21.2704820290013,
8.40164026751963));
#25520=CARTESIAN_POINT('Ctrl Pts',(4.85068927010198,21.4454820290013,8.4016402675109));
#25521=CARTESIAN_POINT('Ctrl Pts',(7.27603390513785,21.6204820290014,4.20082013374672));
#25522=CARTESIAN_POINT('Ctrl Pts',(9.70137854017372,21.7954820290013,-1.74689612655491E-11));
#25523=CARTESIAN_POINT('Ctrl Pts',(7.27603390512273,21.9704820290013,-4.20082013377291));
#25524=CARTESIAN_POINT('Ctrl Pts',(4.85068927007173,22.1454820290013,-8.40164026752836));
#25525=CARTESIAN_POINT('Ctrl Pts',(-1.51301075899711E-11,22.3204820290013,
-8.40164026751963));
#25526=CARTESIAN_POINT('Ctrl Pts',(-4.85068927010199,22.4954820290013,-8.4016402675109));
#25527=CARTESIAN_POINT('Ctrl Pts',(-7.27603390513785,22.6704820290013,-4.20082013374671));
#25528=CARTESIAN_POINT('Ctrl Pts',(-9.70137854017372,22.8454820290013,1.74701493417668E-11));
#25529=CARTESIAN_POINT('Ctrl Pts',(-7.27603390512272,23.0204820290013,4.20082013377292));
#25530=CARTESIAN_POINT('Ctrl Pts',(-4.85068927007173,23.1954820290013,8.40164026752836));
#25531=CARTESIAN_POINT('Ctrl Pts',(1.5129078685785E-11,23.3704820290013,
8.40164026751963));
#25532=CARTESIAN_POINT('Ctrl Pts',(4.85068927010198,23.5454820290013,8.4016402675109));
#25533=CARTESIAN_POINT('Ctrl Pts',(7.27603390513785,23.7204820290013,4.20082013374672));
#25534=CARTESIAN_POINT('Ctrl Pts',(9.70137854017372,23.8954820290013,-1.74689612655491E-11));
#25535=CARTESIAN_POINT('Ctrl Pts',(7.27603390512273,24.0704820290013,-4.20082013377291));
#25536=CARTESIAN_POINT('Ctrl Pts',(4.85068927007173,24.2454820290013,-8.40164026752836));
#25537=CARTESIAN_POINT('Ctrl Pts',(-1.51301075899711E-11,24.4204820290013,
-8.40164026751963));
#25538=CARTESIAN_POINT('Ctrl Pts',(-4.85068927010199,24.5954820290013,-8.4016402675109));
#25539=CARTESIAN_POINT('Ctrl Pts',(-7.27603390513785,24.7704820290013,-4.20082013374671));
#25540=CARTESIAN_POINT('Ctrl Pts',(-9.70137854017372,24.9454820290013,1.74701493417668E-11));
#25541=CARTESIAN_POINT('Ctrl Pts',(-7.27603390512272,25.1204820290013,4.20082013377292));
#25542=CARTESIAN_POINT('Ctrl Pts',(-4.85068927007173,25.2954820290013,8.40164026752836));
#25543=CARTESIAN_POINT('Ctrl Pts',(1.5129078685785E-11,25.4704820290013,
8.40164026751963));
#25544=CARTESIAN_POINT('Ctrl Pts',(4.85068927010198,25.6454820290013,8.4016402675109));
#25545=CARTESIAN_POINT('Ctrl Pts',(7.27603390513785,25.8204820290013,4.20082013374672));
#25546=CARTESIAN_POINT('Ctrl Pts',(9.70137854017372,25.9954820290013,-1.74689612655491E-11));
#25547=CARTESIAN_POINT('Ctrl Pts',(7.27603390512273,26.1704820290013,-4.20082013377291));
#25548=CARTESIAN_POINT('Ctrl Pts',(4.85068927007173,26.3454820290013,-8.40164026752836));
#25549=CARTESIAN_POINT('Ctrl Pts',(-1.51301075899711E-11,26.5204820290013,
-8.40164026751963));
#25550=CARTESIAN_POINT('Origin',(0.,15.4,0.));
#25551=CARTESIAN_POINT('',(-12.9886751345948,15.4,-1.5));
#25552=CARTESIAN_POINT('',(-7.79337567297407,15.4,-10.4985226280624));
#25553=CARTESIAN_POINT('',(-7.79337567297407,15.4,-10.4985226280624));
#25554=CARTESIAN_POINT('',(-5.19529946162075,15.4,-11.9985226280624));
#25555=CARTESIAN_POINT('Origin',(-5.19529946162075,15.4,-8.99852262806237));
#25556=CARTESIAN_POINT('',(5.19529946162075,15.4,-11.9985226280624));
#25557=CARTESIAN_POINT('',(5.19529946162075,15.4,-11.9985226280624));
#25558=CARTESIAN_POINT('',(7.79337567297407,15.4,-10.4985226280624));
#25559=CARTESIAN_POINT('Origin',(5.19529946162075,15.4,-8.99852262806237));
#25560=CARTESIAN_POINT('',(12.9886751345948,15.4,-1.5));
#25561=CARTESIAN_POINT('',(12.9886751345948,15.4,-1.50000000000001));
#25562=CARTESIAN_POINT('',(12.9886751345948,15.4,1.5));
#25563=CARTESIAN_POINT('Origin',(10.3905989232415,15.4,-5.20417042793042E-15));
#25564=CARTESIAN_POINT('',(7.79337567297406,15.4,10.4985226280624));
#25565=CARTESIAN_POINT('',(7.79337567297406,15.4,10.4985226280624));
#25566=CARTESIAN_POINT('',(5.19529946162075,15.4,11.9985226280624));
#25567=CARTESIAN_POINT('Origin',(5.19529946162075,15.4,8.99852262806237));
#25568=CARTESIAN_POINT('',(-5.19529946162075,15.4,11.9985226280624));
#25569=CARTESIAN_POINT('',(-5.19529946162075,15.4,11.9985226280624));
#25570=CARTESIAN_POINT('',(-7.79337567297407,15.4,10.4985226280624));
#25571=CARTESIAN_POINT('Origin',(-5.19529946162075,15.4,8.99852262806237));
#25572=CARTESIAN_POINT('',(-12.9886751345948,15.4,1.5));
#25573=CARTESIAN_POINT('',(-12.9886751345948,15.4,1.5));
#25574=CARTESIAN_POINT('Origin',(-10.3905989232415,15.4,-1.73472347597681E-15));
#25575=CARTESIAN_POINT('Origin',(0.,25.4,0.));
#25576=CARTESIAN_POINT('Ctrl Pts',(5.19529946162075,24.727212412536,10.9985226280624));
#25577=CARTESIAN_POINT('Ctrl Pts',(5.24518280334989,24.7149115564442,10.9985226280624));
#25578=CARTESIAN_POINT('Ctrl Pts',(5.2952655533899,24.7033920689907,10.9966536241576));
#25579=CARTESIAN_POINT('Ctrl Pts',(5.64376907527105,24.629016743781,10.970436558046));
#25580=CARTESIAN_POINT('Ctrl Pts',(5.94190593321436,24.5962843762458,10.8768702574676));
#25581=CARTESIAN_POINT('Ctrl Pts',(6.44869299002713,24.5962843762458,10.5842766137949));
#25582=CARTESIAN_POINT('Ctrl Pts',(6.67879221223778,24.629016743781,10.3728656713007));
#25583=CARTESIAN_POINT('Ctrl Pts',(6.8757486184437,24.7033920689907,10.0841613010991));
#25584=CARTESIAN_POINT('Ctrl Pts',(6.90240859832505,24.7149115564442,10.0417228692255));
#25585=CARTESIAN_POINT('Ctrl Pts',(6.92735026918962,24.727212412536,9.99852262806237));
#25586=CARTESIAN_POINT('Origin',(0.,25.4,0.));
#25587=CARTESIAN_POINT('Ctrl Pts',(12.1226497308104,24.727212412536,0.999999999999993));
#25588=CARTESIAN_POINT('Ctrl Pts',(12.1475914016749,24.7149115564442,0.956799758836891));
#25589=CARTESIAN_POINT('Ctrl Pts',(12.1710141718336,24.7033920689907,0.912492323058454));
#25590=CARTESIAN_POINT('Ctrl Pts',(12.3225612875088,24.629016743781,0.597570886745228));
#25591=CARTESIAN_POINT('Ctrl Pts',(12.3905989232415,24.5962843762458,0.292593643672666));
#25592=CARTESIAN_POINT('Ctrl Pts',(12.3905989232415,24.5962843762458,-0.292593643672677));
#25593=CARTESIAN_POINT('Ctrl Pts',(12.3225612875088,24.629016743781,-0.597570886745239));
#25594=CARTESIAN_POINT('Ctrl Pts',(12.1710141718336,24.7033920689907,-0.912492323058464));
#25595=CARTESIAN_POINT('Ctrl Pts',(12.1475914016749,24.7149115564442,-0.9567997588369));
#25596=CARTESIAN_POINT('Ctrl Pts',(12.1226497308104,24.727212412536,-1.));
#25597=CARTESIAN_POINT('Origin',(0.,25.4,0.));
#25598=CARTESIAN_POINT('Ctrl Pts',(6.92735026918963,24.727212412536,-9.99852262806237));
#25599=CARTESIAN_POINT('Ctrl Pts',(6.90240859832505,24.7149115564442,-10.0417228692255));
#25600=CARTESIAN_POINT('Ctrl Pts',(6.87574861844371,24.7033920689907,-10.0841613010991));
#25601=CARTESIAN_POINT('Ctrl Pts',(6.67879221223779,24.629016743781,-10.3728656713007));
#25602=CARTESIAN_POINT('Ctrl Pts',(6.44869299002713,24.5962843762458,-10.5842766137949));
#25603=CARTESIAN_POINT('Ctrl Pts',(5.94190593321436,24.5962843762458,-10.8768702574676));
#25604=CARTESIAN_POINT('Ctrl Pts',(5.64376907527106,24.629016743781,-10.970436558046));
#25605=CARTESIAN_POINT('Ctrl Pts',(5.29526555338991,24.7033920689907,-10.9966536241576));
#25606=CARTESIAN_POINT('Ctrl Pts',(5.2451828033499,24.7149115564442,-10.9985226280624));
#25607=CARTESIAN_POINT('Ctrl Pts',(5.19529946162075,24.727212412536,-10.9985226280624));
#25608=CARTESIAN_POINT('Origin',(0.,25.4,0.));
#25609=CARTESIAN_POINT('Ctrl Pts',(-5.19529946162075,24.727212412536,-10.9985226280624));
#25610=CARTESIAN_POINT('Ctrl Pts',(-5.2451828033499,24.7149115564442,-10.9985226280624));
#25611=CARTESIAN_POINT('Ctrl Pts',(-5.2952655533899,24.7033920689907,-10.9966536241576));
#25612=CARTESIAN_POINT('Ctrl Pts',(-5.64376907527106,24.629016743781,-10.970436558046));
#25613=CARTESIAN_POINT('Ctrl Pts',(-5.94190593321436,24.5962843762458,-10.8768702574676));
#25614=CARTESIAN_POINT('Ctrl Pts',(-6.44869299002714,24.5962843762458,-10.5842766137949));
#25615=CARTESIAN_POINT('Ctrl Pts',(-6.67879221223779,24.629016743781,-10.3728656713007));
#25616=CARTESIAN_POINT('Ctrl Pts',(-6.87574861844371,24.7033920689907,-10.0841613010991));
#25617=CARTESIAN_POINT('Ctrl Pts',(-6.90240859832505,24.7149115564442,-10.0417228692255));
#25618=CARTESIAN_POINT('Ctrl Pts',(-6.92735026918963,24.727212412536,-9.99852262806237));
#25619=CARTESIAN_POINT('Origin',(0.,25.4,0.));
#25620=CARTESIAN_POINT('Ctrl Pts',(-12.1226497308104,24.727212412536,-1.));
#25621=CARTESIAN_POINT('Ctrl Pts',(-12.1475914016749,24.7149115564442,-0.956799758836898));
#25622=CARTESIAN_POINT('Ctrl Pts',(-12.1710141718336,24.7033920689907,-0.912492323058462));
#25623=CARTESIAN_POINT('Ctrl Pts',(-12.3225612875088,24.629016743781,-0.597570886745235));
#25624=CARTESIAN_POINT('Ctrl Pts',(-12.3905989232415,24.5962843762458,-0.292593643672673));
#25625=CARTESIAN_POINT('Ctrl Pts',(-12.3905989232415,24.5962843762458,0.29259364367267));
#25626=CARTESIAN_POINT('Ctrl Pts',(-12.3225612875088,24.629016743781,0.597570886745232));
#25627=CARTESIAN_POINT('Ctrl Pts',(-12.1710141718336,24.7033920689907,0.912492323058458));
#25628=CARTESIAN_POINT('Ctrl Pts',(-12.147591401675,24.7149115564442,0.956799758836896));
#25629=CARTESIAN_POINT('Ctrl Pts',(-12.1226497308104,24.727212412536,0.999999999999997));
#25630=CARTESIAN_POINT('Origin',(0.,25.4,0.));
#25631=CARTESIAN_POINT('Ctrl Pts',(-6.92735026918963,24.727212412536,9.99852262806237));
#25632=CARTESIAN_POINT('Ctrl Pts',(-6.90240859832505,24.7149115564442,10.0417228692255));
#25633=CARTESIAN_POINT('Ctrl Pts',(-6.87574861844371,24.7033920689907,10.0841613010991));
#25634=CARTESIAN_POINT('Ctrl Pts',(-6.67879221223779,24.629016743781,10.3728656713007));
#25635=CARTESIAN_POINT('Ctrl Pts',(-6.44869299002713,24.5962843762458,10.5842766137949));
#25636=CARTESIAN_POINT('Ctrl Pts',(-5.94190593321436,24.5962843762458,10.8768702574676));
#25637=CARTESIAN_POINT('Ctrl Pts',(-5.64376907527106,24.629016743781,10.970436558046));
#25638=CARTESIAN_POINT('Ctrl Pts',(-5.2952655533899,24.7033920689907,10.9966536241576));
#25639=CARTESIAN_POINT('Ctrl Pts',(-5.2451828033499,24.7149115564442,10.9985226280624));
#25640=CARTESIAN_POINT('Ctrl Pts',(-5.19529946162075,24.727212412536,10.9985226280624));
#25641=CARTESIAN_POINT('Origin',(-10.3905989232415,15.4,-1.73472347597681E-15));
#25642=CARTESIAN_POINT('Origin',(-10.3905989232415,16.4,-1.73472347597681E-15));
#25643=CARTESIAN_POINT('Origin',(-5.19529946162075,15.4,-8.99852262806237));
#25644=CARTESIAN_POINT('Origin',(-5.19529946162075,16.4,-8.99852262806237));
#25645=CARTESIAN_POINT('Origin',(5.19529946162075,15.4,-8.99852262806237));
#25646=CARTESIAN_POINT('Origin',(5.19529946162075,16.4,-8.99852262806237));
#25647=CARTESIAN_POINT('Origin',(10.3905989232415,15.4,-5.20417042793042E-15));
#25648=CARTESIAN_POINT('Origin',(10.3905989232415,16.4,-5.20417042793042E-15));
#25649=CARTESIAN_POINT('Origin',(5.19529946162075,15.4,8.99852262806237));
#25650=CARTESIAN_POINT('Origin',(5.19529946162075,16.4,8.99852262806237));
#25651=CARTESIAN_POINT('Origin',(-5.19529946162075,15.4,8.99852262806237));
#25652=CARTESIAN_POINT('Origin',(-5.19529946162075,16.4,8.99852262806237));
#25653=CARTESIAN_POINT('Origin',(5.19529946162075,16.4,8.99852262806237));
#25654=CARTESIAN_POINT('Origin',(7.79337567297406,16.4,10.4985226280624));
#25655=CARTESIAN_POINT('Origin',(5.19529946162075,16.4,11.9985226280624));
#25656=CARTESIAN_POINT('Origin',(-6.35,16.4,11.9985226280624));
#25657=CARTESIAN_POINT('Origin',(-5.19529946162075,16.4,11.9985226280624));
#25658=CARTESIAN_POINT('Origin',(7.21602540378444,16.4,11.4985226280624));
#25659=CARTESIAN_POINT('Origin',(12.9886751345948,16.4,1.5));
#25660=CARTESIAN_POINT('Origin',(-5.19529946162075,16.4,8.99852262806237));
#25661=CARTESIAN_POINT('Origin',(-7.79337567297407,16.4,10.4985226280624));
#25662=CARTESIAN_POINT('Origin',(10.3905989232415,16.4,-5.20417042793042E-15));
#25663=CARTESIAN_POINT('Origin',(12.9886751345948,16.4,-1.5));
#25664=CARTESIAN_POINT('Origin',(-13.5660254037844,16.4,0.5));
#25665=CARTESIAN_POINT('Origin',(-12.9886751345948,16.4,1.5));
#25666=CARTESIAN_POINT('Origin',(13.5660254037844,16.4,-0.500000000000007));
#25667=CARTESIAN_POINT('Origin',(7.79337567297406,16.4,-10.4985226280624));
#25668=CARTESIAN_POINT('Origin',(-10.3905989232415,16.4,-1.73472347597681E-15));
#25669=CARTESIAN_POINT('Origin',(-12.9886751345948,16.4,-1.5));
#25670=CARTESIAN_POINT('Origin',(5.19529946162075,16.4,-8.99852262806237));
#25671=CARTESIAN_POINT('Origin',(5.19529946162075,16.4,-11.9985226280624));
#25672=CARTESIAN_POINT('Origin',(-7.21602540378444,16.4,-11.4985226280624));
#25673=CARTESIAN_POINT('Origin',(-7.79337567297407,16.4,-10.4985226280624));
#25674=CARTESIAN_POINT('Origin',(6.35,16.4,-11.9985226280624));
#25675=CARTESIAN_POINT('Origin',(-5.19529946162075,16.4,-11.9985226280624));
#25676=CARTESIAN_POINT('Origin',(-5.19529946162075,16.4,-8.99852262806237));
#25677=CARTESIAN_POINT('Origin',(-48.,-7.90000000000001,7.7));
#25678=CARTESIAN_POINT('Origin',(-48.,-21.9,7.7));
#25679=CARTESIAN_POINT('Origin',(-48.,-7.90000000000001,7.7));
#25680=CARTESIAN_POINT('Origin',(-48.,-7.90000000000001,7.7));
#25681=CARTESIAN_POINT('Origin',(-48.,-7.90000000000001,7.7));
#25682=CARTESIAN_POINT('Origin',(-48.,-7.90000000000001,7.7));
#25683=CARTESIAN_POINT('Ctrl Pts',(-37.2370215606994,11.6489333498058,7.7));
#25684=CARTESIAN_POINT('Ctrl Pts',(-37.2370215606994,11.6489333498058,7.8077479627862));
#25685=CARTESIAN_POINT('Ctrl Pts',(-37.2348311473986,11.6461366519307,7.91713462674333));
#25686=CARTESIAN_POINT('Ctrl Pts',(-37.2302752431834,11.6403197188282,8.02776680121651));
#25687=CARTESIAN_POINT('Ctrl Pts',(-37.2256774210564,11.6344492653536,8.13941687894383));
#25688=CARTESIAN_POINT('Ctrl Pts',(-37.2186702459623,11.6255025740195,8.25233526639646));
#25689=CARTESIAN_POINT('Ctrl Pts',(-37.2090968020071,11.6132792961762,8.36607958557781));
#25690=CARTESIAN_POINT('Ctrl Pts',(-37.2004639399102,11.6022569438768,8.46864863245277));
#25691=CARTESIAN_POINT('Ctrl Pts',(-37.1897445552481,11.5885705403581,8.57188861673383));
#25692=CARTESIAN_POINT('Ctrl Pts',(-37.1768406531966,11.572094966805,8.67545161008087));
#25693=CARTESIAN_POINT('Ctrl Pts',(-37.1626489093056,11.5539750896244,8.78935045031606));
#25694=CARTESIAN_POINT('Ctrl Pts',(-37.1458143533317,11.5324808963114,8.9036374875757));
#25695=CARTESIAN_POINT('Ctrl Pts',(-37.1262661819627,11.5075219859026,9.01783447063753));
#25696=CARTESIAN_POINT('Ctrl Pts',(-37.1064327010615,11.4821987951262,9.13369818186538));
#25697=CARTESIAN_POINT('Ctrl Pts',(-37.083805740066,11.4533089168019,9.24946879412115));
#25698=CARTESIAN_POINT('Ctrl Pts',(-37.0583419637689,11.420797020969,9.36462556197383));
#25699=CARTESIAN_POINT('Ctrl Pts',(-37.0399180815693,11.3972735917682,9.44794528253116));
#25700=CARTESIAN_POINT('Ctrl Pts',(-37.0200097712987,11.3718548595984,9.53094317961308));
#25701=CARTESIAN_POINT('Ctrl Pts',(-36.9986106492179,11.3445326737651,9.61341716182606));
#25702=CARTESIAN_POINT('Ctrl Pts',(-36.9694052390191,11.3072434970515,9.72597722256865));
#25703=CARTESIAN_POINT('Ctrl Pts',(-36.9373995710248,11.2663789790887,9.83753573161566));
#25704=CARTESIAN_POINT('Ctrl Pts',(-36.902657311863,11.2220204087928,9.94761455701875));
#25705=CARTESIAN_POINT('Ctrl Pts',(-36.8657225277775,11.1748624445227,10.0646402699898));
#25706=CARTESIAN_POINT('Ctrl Pts',(-36.8256946326858,11.1237552269421,10.1799930477234));
#25707=CARTESIAN_POINT('Ctrl Pts',(-36.7826890673221,11.0688461496304,10.2931010720517));
#25708=CARTESIAN_POINT('Ctrl Pts',(-36.7410984721777,11.0157436921946,10.4024876132504));
#25709=CARTESIAN_POINT('Ctrl Pts',(-36.69672330252,10.9590859177681,10.5097741691194));
#25710=CARTESIAN_POINT('Ctrl Pts',(-36.6497011112435,10.8990484525159,10.6144542442965));
#25711=CARTESIAN_POINT('Ctrl Pts',(-36.6002792788918,10.835947149451,10.7244763633326));
#25712=CARTESIAN_POINT('Ctrl Pts',(-36.5479333176005,10.7691123476947,10.8316183371238));
#25713=CARTESIAN_POINT('Ctrl Pts',(-36.4928582485832,10.6987930483889,10.9353147905031));
#25714=CARTESIAN_POINT('Ctrl Pts',(-36.4377831795658,10.6284737490832,11.0390112438824));
#25715=CARTESIAN_POINT('Ctrl Pts',(-36.3799792804388,10.5546703066858,11.1392614617744));
#25716=CARTESIAN_POINT('Ctrl Pts',(-36.3196738148537,10.4776728891628,11.2355339059335));
#25717=CARTESIAN_POINT('Ctrl Pts',(-36.2619915983051,10.4040248098692,11.3276185605792));
#25718=CARTESIAN_POINT('Ctrl Pts',(-36.2020302432153,10.3274667491973,11.4160493299939));
#25719=CARTESIAN_POINT('Ctrl Pts',(-36.1400807365056,10.2483702363487,11.5005079328353));
#25720=CARTESIAN_POINT('Ctrl Pts',(-36.0768630623417,10.1676545399319,11.5866954865115));
#25721=CARTESIAN_POINT('Ctrl Pts',(-36.011575325106,10.0842958076127,11.6687460449283));
#25722=CARTESIAN_POINT('Ctrl Pts',(-35.944546007913,9.99871344335855,11.7463674222083));
#25723=CARTESIAN_POINT('Ctrl Pts',(-35.8792875513239,9.91539209627714,11.8219381051833));
#25724=CARTESIAN_POINT('Ctrl Pts',(-35.8123787392189,9.82996359171854,11.893310428993));
#25725=CARTESIAN_POINT('Ctrl Pts',(-35.7441350624009,9.74283074519608,11.9602622260613));
#25726=CARTESIAN_POINT('Ctrl Pts',(-35.6731135837839,9.65215122901703,12.0299392400438));
#25727=CARTESIAN_POINT('Ctrl Pts',(-35.6006467011536,9.55962623539705,12.0948278197615));
#25728=CARTESIAN_POINT('Ctrl Pts',(-35.5270979720375,9.46571995096445,12.1547367464213));
#25729=CARTESIAN_POINT('Ctrl Pts',(-35.4581365562657,9.37767070249793,12.2109090888871));
#25730=CARTESIAN_POINT('Ctrl Pts',(-35.3882243786871,9.28840753083064,12.2627039132039));
#25731=CARTESIAN_POINT('Ctrl Pts',(-35.3176628312434,9.19831525019048,12.3100156165359));
#25732=CARTESIAN_POINT('Ctrl Pts',(-35.312969077141,9.19232231172517,12.313162791019));
#25733=CARTESIAN_POINT('Ctrl Pts',(-35.3082724492566,9.18632570404355,12.3162901472982));
#25734=CARTESIAN_POINT('Ctrl Pts',(-35.3035730360603,9.18032554010357,12.3193976625566));
#25735=CARTESIAN_POINT('Ctrl Pts',(-35.2309234491108,9.08756727142935,12.367437639153));
#25736=CARTESIAN_POINT('Ctrl Pts',(-35.157622566231,8.99397743460166,12.4107244434961));
#25737=CARTESIAN_POINT('Ctrl Pts',(-35.0840243715693,8.90000799305338,12.4493287586889));
#25738=CARTESIAN_POINT('Ctrl Pts',(-35.011193186692,8.8070178619548,12.4875307557594));
#25739=CARTESIAN_POINT('Ctrl Pts',(-34.9380711627225,8.71365639040143,12.521147462252));
#25740=CARTESIAN_POINT('Ctrl Pts',(-34.864990431616,8.62034764116423,12.5502951735018));
#25741=CARTESIAN_POINT('Ctrl Pts',(-34.793030700632,8.52847017371273,12.5789957821106));
#25742=CARTESIAN_POINT('Ctrl Pts',(-34.721111242736,8.43664412653876,12.603363613898));
#25743=CARTESIAN_POINT('Ctrl Pts',(-34.6495345151887,8.34525567405873,12.6235541698602));
#25744=CARTESIAN_POINT('Ctrl Pts',(-34.5785107837497,8.25457328149928,12.6435887351917));
#25745=CARTESIAN_POINT('Ctrl Pts',(-34.5078247134336,8.16432201129683,12.6595104555204));
#25746=CARTESIAN_POINT('Ctrl Pts',(-34.4377539870199,8.07485640605711,12.6715132355078));
#25747=CARTESIAN_POINT('Ctrl Pts',(-34.368285509019,7.98615974558962,12.6834128532252));
#25748=CARTESIAN_POINT('Ctrl Pts',(-34.2994219988082,7.898235501968,12.6914607677224));
#25749=CARTESIAN_POINT('Ctrl Pts',(-34.2314137778158,7.81140328309775,12.6958851496815));
#25750=CARTESIAN_POINT('Ctrl Pts',(-34.1889236830279,7.75715235348064,12.6986494097382));
#25751=CARTESIAN_POINT('Ctrl Pts',(-34.1467670361917,7.70332716688543,12.7));
#25752=CARTESIAN_POINT('Ctrl Pts',(-34.1050004454305,7.65,12.7));
#25753=CARTESIAN_POINT('Ctrl Pts',(-34.1050004454305,7.65,12.7));
#25754=CARTESIAN_POINT('Ctrl Pts',(-34.1050004454305,7.65,12.7));
#25755=CARTESIAN_POINT('Ctrl Pts',(-34.1050004454305,7.65,12.7));
#25756=CARTESIAN_POINT('Ctrl Pts',(-34.2221767330303,8.30461645762901,12.7));
#25757=CARTESIAN_POINT('Ctrl Pts',(-34.3684200110126,8.23864736688717,12.7));
#25758=CARTESIAN_POINT('Ctrl Pts',(-34.5150549589694,8.17355351674842,12.7));
#25759=CARTESIAN_POINT('Ctrl Pts',(-34.3392646891937,8.95873944331344,12.5698633744289));
#25760=CARTESIAN_POINT('Ctrl Pts',(-34.6344129874181,8.833045375353,12.5964281310995));
#25761=CARTESIAN_POINT('Ctrl Pts',(-34.9248003596003,8.69671236121519,12.5698633744284));
#25762=CARTESIAN_POINT('Ctrl Pts',(-34.5557392046831,10.1680948803375,12.0689319506839));
#25763=CARTESIAN_POINT('Ctrl Pts',(-35.1421214426245,9.96758997397988,12.1778901074191));
#25764=CARTESIAN_POINT('Ctrl Pts',(-35.6823457125228,9.66393871899066,12.0689319506845));
#25765=CARTESIAN_POINT('Ctrl Pts',(-34.6550194892076,10.7227336174031,11.6983341944624));
#25766=CARTESIAN_POINT('Ctrl Pts',(-35.3869447814668,10.5146815062463,11.8564353766687));
#25767=CARTESIAN_POINT('Ctrl Pts',(-36.0297737596904,10.1075313875409,11.6983341944627));
#25768=CARTESIAN_POINT('Ctrl Pts',(-34.8207019100435,11.6483341944624,10.7727336174031));
#25769=CARTESIAN_POINT('Ctrl Pts',(-35.8197142077533,11.48176450439,10.9904588000058));
#25770=CARTESIAN_POINT('Ctrl Pts',(-36.6095738700229,10.8478143907806,10.7727336174027));
#25771=CARTESIAN_POINT('Ctrl Pts',(-34.8870388756109,12.0189319519099,10.2180948773777));
#25772=CARTESIAN_POINT('Ctrl Pts',(-36.0061527172947,11.8983870794296,10.439161626936));
#25773=CARTESIAN_POINT('Ctrl Pts',(-36.8417178703412,11.144213537105,10.2180948773781));
#25774=CARTESIAN_POINT('Ctrl Pts',(-34.9542888854506,12.3946305178797,9.31107830404935));
#25775=CARTESIAN_POINT('Ctrl Pts',(-36.2030730684665,12.338432775914,9.4822033404738));
#25776=CARTESIAN_POINT('Ctrl Pts',(-37.0770570386603,11.4446922420911,9.31107830404915));
#25777=CARTESIAN_POINT('Ctrl Pts',(-34.9713749152927,12.4900832460695,8.99641282927341));
#25778=CARTESIAN_POINT('Ctrl Pts',(-36.2546886211118,12.4537748504033,9.14076955834494));
#25779=CARTESIAN_POINT('Ctrl Pts',(-37.1368490306999,11.5210340617091,8.99641282927351));
#25780=CARTESIAN_POINT('Ctrl Pts',(-34.9942307537467,12.6177695579628,8.35449039088788));
#25781=CARTESIAN_POINT('Ctrl Pts',(-36.3245787042152,12.6099538847863,8.43215085130189));
#25782=CARTESIAN_POINT('Ctrl Pts',(-37.2168322756968,11.6231558718972,8.35449039088778));
#25783=CARTESIAN_POINT('Ctrl Pts',(-34.9999999999986,12.65,8.02725293702972));
#25784=CARTESIAN_POINT('Ctrl Pts',(-36.3424993318352,12.6499999999596,8.06661933627904));
#25785=CARTESIAN_POINT('Ctrl Pts',(-37.2370215607001,11.648933349805,8.02725293702981));
#25786=CARTESIAN_POINT('Ctrl Pts',(-35.,12.65,7.7));
#25787=CARTESIAN_POINT('Ctrl Pts',(-36.3424993318543,12.65,7.69999999999999));
#25788=CARTESIAN_POINT('Ctrl Pts',(-37.2370215606994,11.6489333498058,7.7));
#25789=CARTESIAN_POINT('Ctrl Pts',(-35.,12.65,7.7));
#25790=CARTESIAN_POINT('Ctrl Pts',(-35.,12.65,7.80774796278557));
#25791=CARTESIAN_POINT('Ctrl Pts',(-34.9993740722507,12.6465031951891,7.91713462674209));
#25792=CARTESIAN_POINT('Ctrl Pts',(-34.9980721869531,12.6392300893458,8.02776680121466));
#25793=CARTESIAN_POINT('Ctrl Pts',(-34.9967583232841,12.6318900651929,8.13941687894151));
#25794=CARTESIAN_POINT('Ctrl Pts',(-34.9947559681418,12.6207037180452,8.25233526639368));
#25795=CARTESIAN_POINT('Ctrl Pts',(-34.9920202815809,12.6054205452911,8.36607958557456));
#25796=CARTESIAN_POINT('Ctrl Pts',(-34.9895533736499,12.5916389298757,8.46864863245064));
#25797=CARTESIAN_POINT('Ctrl Pts',(-34.9864902255602,12.5745263621959,8.57188861673282));
#25798=CARTESIAN_POINT('Ctrl Pts',(-34.9828028345235,12.5539264020161,8.67545161008097));
#25799=CARTESIAN_POINT('Ctrl Pts',(-34.9787474325986,12.5312705140633,8.78935045031526));
#25800=CARTESIAN_POINT('Ctrl Pts',(-34.9739368264302,12.5043956058905,8.90363748757406));
#25801=CARTESIAN_POINT('Ctrl Pts',(-34.9683507834176,12.4731886461523,9.01783447063506));
#25802=CARTESIAN_POINT('Ctrl Pts',(-34.9626832109724,12.4415262144972,9.1336981818622));
#25803=CARTESIAN_POINT('Ctrl Pts',(-34.9562173797198,12.4054042342126,9.24946879411729));
#25804=CARTESIAN_POINT('Ctrl Pts',(-34.9489409062851,12.3647535244,9.36462556196926));
#25805=CARTESIAN_POINT('Ctrl Pts',(-34.9436761377044,12.335341394785,9.44794528252829));
#25806=CARTESIAN_POINT('Ctrl Pts',(-34.9379871821807,12.3035595045322,9.53094317961187));
#25807=CARTESIAN_POINT('Ctrl Pts',(-34.9318722155105,12.269397662556,9.61341716182647));
#25808=CARTESIAN_POINT('Ctrl Pts',(-34.9235265408946,12.2227737588152,9.72597722256831));
#25809=CARTESIAN_POINT('Ctrl Pts',(-34.9143806706902,12.1716794864331,9.83753573161463));
#25810=CARTESIAN_POINT('Ctrl Pts',(-34.9044527981345,12.1162164836579,9.94761455701708));
#25811=CARTESIAN_POINT('Ctrl Pts',(-34.8938983944165,12.0572533050486,10.0646402699884));
#25812=CARTESIAN_POINT('Ctrl Pts',(-34.8824601100121,11.9933522430528,10.1799930477223));
#25813=CARTESIAN_POINT('Ctrl Pts',(-34.870170933015,11.924697588788,10.2931010720508));
#25814=CARTESIAN_POINT('Ctrl Pts',(-34.8582860948361,11.8583018117264,10.4024876132491));
#25815=CARTESIAN_POINT('Ctrl Pts',(-34.8456055426893,11.7874607030231,10.5097741691177));
#25816=CARTESIAN_POINT('Ctrl Pts',(-34.8321685833911,11.712393853941,10.6144542442945));
#25817=CARTESIAN_POINT('Ctrl Pts',(-34.8180459078685,11.6334961860564,10.7244763633312));
#25818=CARTESIAN_POINT('Ctrl Pts',(-34.8030876396081,11.5499303999952,10.831618337123));
#25819=CARTESIAN_POINT('Ctrl Pts',(-34.7873495074485,11.4620078302062,10.9353147905027));
#25820=CARTESIAN_POINT('Ctrl Pts',(-34.7716113752889,11.3740852604171,11.0390112438825));
#25821=CARTESIAN_POINT('Ctrl Pts',(-34.7550934585612,11.2818063500906,11.139261461775));
#25822=CARTESIAN_POINT('Ctrl Pts',(-34.737860699633,11.1855339059311,11.2355339059344));
#25823=CARTESIAN_POINT('Ctrl Pts',(-34.7213775546548,11.0934492512856,11.3276185605798));
#25824=CARTESIAN_POINT('Ctrl Pts',(-34.7042431279947,10.99772614968,11.4160493299941));
#25825=CARTESIAN_POINT('Ctrl Pts',(-34.6865405714439,10.8988291364902,11.5005079328351));
#25826=CARTESIAN_POINT('Ctrl Pts',(-34.6684756261143,10.7979076039761,11.5866954865114));
#25827=CARTESIAN_POINT('Ctrl Pts',(-34.6498191440552,10.6936813953507,11.6687460449281));
#25828=CARTESIAN_POINT('Ctrl Pts',(-34.6306649918883,10.5866749054099,11.7463674222083));
#25829=CARTESIAN_POINT('Ctrl Pts',(-34.6120168770032,10.482495440797,11.821938105183));
#25830=CARTESIAN_POINT('Ctrl Pts',(-34.5928971601087,10.3756813267753,11.8933104289926));
#25831=CARTESIAN_POINT('Ctrl Pts',(-34.5733959951717,10.266736217042,11.9602622260608));
#25832=CARTESIAN_POINT('Ctrl Pts',(-34.5531010516228,10.1533565877173,12.0299392400434));
#25833=CARTESIAN_POINT('Ctrl Pts',(-34.5323930725609,10.0376694962776,12.0948278197612));
#25834=CARTESIAN_POINT('Ctrl Pts',(-34.5113759473958,9.9202553307762,12.1547367464212));
#25835=CARTESIAN_POINT('Ctrl Pts',(-34.4916696829333,9.81016441306816,12.2109090888872));
#25836=CARTESIAN_POINT('Ctrl Pts',(-34.471691730841,9.69855568661636,12.2627039132042));
#25837=CARTESIAN_POINT('Ctrl Pts',(-34.4515282162257,9.5859102975093,12.3100156165363));
#25838=CARTESIAN_POINT('Ctrl Pts',(-34.4501869392431,9.57841712627964,12.3131627910194));
#25839=CARTESIAN_POINT('Ctrl Pts',(-34.4488448410548,9.57091936730622,12.3162901472986));
#25840=CARTESIAN_POINT('Ctrl Pts',(-34.4475019469419,9.56341716182413,12.319397662557));
#25841=CARTESIAN_POINT('Ctrl Pts',(-34.4267417586902,9.44743839878783,12.3674376391538));
#25842=CARTESIAN_POINT('Ctrl Pts',(-34.4057954575275,9.33041989830073,12.4107244434972));
#25843=CARTESIAN_POINT('Ctrl Pts',(-34.3847641971955,9.21292676534625,12.4493287586903));
#25844=CARTESIAN_POINT('Ctrl Pts',(-34.3639521159143,9.09665809697244,12.4875307557612));
#25845=CARTESIAN_POINT('Ctrl Pts',(-34.3430569250855,8.97992512921895,12.521147462254));
#25846=CARTESIAN_POINT('Ctrl Pts',(-34.3221735340156,8.86325808193921,12.5502951735039));
#25847=CARTESIAN_POINT('Ctrl Pts',(-34.301610477507,8.74838061410455,12.578995782113));
#25848=CARTESIAN_POINT('Ctrl Pts',(-34.2810589293485,8.63356743876123,12.6033636139005));
#25849=CARTESIAN_POINT('Ctrl Pts',(-34.2606053190705,8.51930140268692,12.6235541698628));
#25850=CARTESIAN_POINT('Ctrl Pts',(-34.2403097317599,8.40591817692525,12.6435887351944));
#25851=CARTESIAN_POINT('Ctrl Pts',(-34.2201106337586,8.29307399785344,12.659510455523));
#25852=CARTESIAN_POINT('Ctrl Pts',(-34.2000873750951,8.18121216193919,12.6715132355102));
#25853=CARTESIAN_POINT('Ctrl Pts',(-34.1802362136306,8.07031176336932,12.6834128532274));
#25854=CARTESIAN_POINT('Ctrl Pts',(-34.1605579264484,7.9603771433938,12.6914607677241));
#25855=CARTESIAN_POINT('Ctrl Pts',(-34.1411240448565,7.85180791845727,12.6958851496827));
#25856=CARTESIAN_POINT('Ctrl Pts',(-34.1289821676136,7.78397616825827,12.6986494097386));
#25857=CARTESIAN_POINT('Ctrl Pts',(-34.1169355757335,7.71667673878648,12.7));
#25858=CARTESIAN_POINT('Ctrl Pts',(-34.1050004454305,7.65,12.7));
#25859=CARTESIAN_POINT('Origin',(-48.,7.65,7.7));
#25860=CARTESIAN_POINT('Origin',(-17.9697662756086,7.65,7.7));
#25861=CARTESIAN_POINT('Ctrl Pts',(-17.9697662756086,7.65,12.7));
#25862=CARTESIAN_POINT('Ctrl Pts',(-17.9697662756086,12.65,12.7));
#25863=CARTESIAN_POINT('Ctrl Pts',(-17.9697662756086,12.65,7.7));
#25864=CARTESIAN_POINT('Ctrl Pts',(-17.5769226509334,7.65000000135137,12.7));
#25865=CARTESIAN_POINT('Ctrl Pts',(-17.8797974234722,12.5223340542636,12.7));
#25866=CARTESIAN_POINT('Ctrl Pts',(-17.8786433834304,12.65,7.82930352963304));
#25867=CARTESIAN_POINT('Ctrl Pts',(-17.1871178707086,7.68525114336172,12.7));
#25868=CARTESIAN_POINT('Ctrl Pts',(-17.7621458420668,12.4006679911033,12.699999999999));
#25869=CARTESIAN_POINT('Ctrl Pts',(-17.7836615820008,12.6532040193815,7.96407165192601));
#25870=CARTESIAN_POINT('Ctrl Pts',(-16.8005208252602,7.75488674445212,12.7));
#25871=CARTESIAN_POINT('Ctrl Pts',(-17.617785931914,12.2921100651331,12.7));
#25872=CARTESIAN_POINT('Ctrl Pts',(-17.6839681951541,12.6595351585866,8.1049008253337));
#25873=CARTESIAN_POINT('Origin',(-16.8005208252601,7.75488674445212,7.7));
#25874=CARTESIAN_POINT('Ctrl Pts',(-16.8005208252602,7.75488674445212,12.7));
#25875=CARTESIAN_POINT('Ctrl Pts',(-17.617785931914,12.2921100651331,12.7));
#25876=CARTESIAN_POINT('Ctrl Pts',(-17.6839681951541,12.6595351585866,8.10490082533369));
#25877=CARTESIAN_POINT('Ctrl Pts',(-16.57400807036,7.82781362133464,12.7));
#25878=CARTESIAN_POINT('Ctrl Pts',(-17.6286821698629,12.155095870898,12.671192031208));
#25879=CARTESIAN_POINT('Ctrl Pts',(-17.5797557624158,12.6661532847416,8.25211370792749));
#25880=CARTESIAN_POINT('Ctrl Pts',(-16.3460043190073,7.93905335192941,12.712469440238));
#25881=CARTESIAN_POINT('Ctrl Pts',(-17.5788419030212,12.0132242375904,12.6289721703847));
#25882=CARTESIAN_POINT('Ctrl Pts',(-17.4601309122998,12.6762775771018,8.42880065885016));
#25883=CARTESIAN_POINT('Ctrl Pts',(-15.9085797765213,8.21703647488218,12.7591081700646));
#25884=CARTESIAN_POINT('Ctrl Pts',(-17.3634553041143,11.7807433434256,12.5578936033112));
#25885=CARTESIAN_POINT('Ctrl Pts',(-17.1967503219572,12.7015487707901,8.82270036173133));
#25886=CARTESIAN_POINT('Ctrl Pts',(-15.6990852529236,8.3825852909746,12.7928422221643));
#25887=CARTESIAN_POINT('Ctrl Pts',(-17.2053550226203,11.6893488147424,12.5292392590373));
#25888=CARTESIAN_POINT('Ctrl Pts',(-17.053307387847,12.7165986624452,9.03920832840638));
#25889=CARTESIAN_POINT('Ctrl Pts',(-15.2946854951174,8.75509815651616,12.8776711254801));
#25890=CARTESIAN_POINT('Ctrl Pts',(-16.8188792119444,11.5743897252593,12.5075888732474));
#25891=CARTESIAN_POINT('Ctrl Pts',(-16.7385788933035,12.7504634691449,9.50671774903932));
#25892=CARTESIAN_POINT('Ctrl Pts',(-15.0994609327293,8.96258837046799,12.9289025745581));
#25893=CARTESIAN_POINT('Ctrl Pts',(-16.5928074468314,11.5481648613874,12.5132247397972));
#25894=CARTESIAN_POINT('Ctrl Pts',(-16.5669250005632,12.7693262151711,9.75824593848983));
#25895=CARTESIAN_POINT('Ctrl Pts',(-14.7226800076233,9.40977222762574,13.0463331216422));
#25896=CARTESIAN_POINT('Ctrl Pts',(-16.1048897677201,11.5609929861839,12.5675172427461));
#25897=CARTESIAN_POINT('Ctrl Pts',(-16.1929560790172,12.8099792937465,10.2884101870157));
#25898=CARTESIAN_POINT('Ctrl Pts',(-14.5437893111222,9.64614677008646,13.1116414598527));
#25899=CARTESIAN_POINT('Ctrl Pts',(-15.8472046102766,11.5974627760302,12.6142743787051));
#25900=CARTESIAN_POINT('Ctrl Pts',(-15.993385566602,12.8314678879228,10.5631032975644));
#25901=CARTESIAN_POINT('Ctrl Pts',(-14.0293669548612,10.3837101835141,13.3245337884544));
#25902=CARTESIAN_POINT('Ctrl Pts',(-15.0766777630351,11.7789057456683,12.8105573724733));
#25903=CARTESIAN_POINT('Ctrl Pts',(-15.354300460823,12.898519108126,11.4060563768849));
#25904=CARTESIAN_POINT('Ctrl Pts',(-13.7157820791968,10.9130303131153,13.4887739635291));
#25905=CARTESIAN_POINT('Ctrl Pts',(-14.5379048034935,11.9964940699689,13.0187576709113));
#25906=CARTESIAN_POINT('Ctrl Pts',(-14.8736435223247,12.9466391191654,11.993249292684));
#25907=CARTESIAN_POINT('Ctrl Pts',(-13.1283088804427,12.0122001031246,13.8579187609855));
#25908=CARTESIAN_POINT('Ctrl Pts',(-13.525404177229,12.5253529301391,13.5631951324379));
#25909=CARTESIAN_POINT('Ctrl Pts',(-13.8052132993074,13.0465636459474,13.1624707293919));
#25910=CARTESIAN_POINT('Ctrl Pts',(-12.8547128646902,12.5827074287807,14.063208861629));
#25911=CARTESIAN_POINT('Ctrl Pts',(-13.0355631159118,12.8406828545529,13.9037139318704));
#25912=CARTESIAN_POINT('Ctrl Pts',(-13.2169060869103,13.0984138348476,13.7437844641131));
#25913=CARTESIAN_POINT('Ctrl Pts',(-12.6003906189451,13.15,14.2875));
#25914=CARTESIAN_POINT('Ctrl Pts',(-12.6003906189451,13.15,14.2875));
#25915=CARTESIAN_POINT('Ctrl Pts',(-12.6003906189451,13.15,14.2875));
#25916=CARTESIAN_POINT('Origin',(-48.,-22.9,-7.7));
#25917=CARTESIAN_POINT('Origin',(-48.,-21.9,-7.7));
#25918=CARTESIAN_POINT('Origin',(-48.,-7.90000000000001,-7.7));
#25919=CARTESIAN_POINT('Origin',(-48.,-7.90000000000001,-7.7));
#25920=CARTESIAN_POINT('Origin',(-48.,-7.90000000000001,-7.7));
#25921=CARTESIAN_POINT('Origin',(-48.,-7.90000000000001,-7.7));
#25922=CARTESIAN_POINT('Ctrl Pts',(-34.1050004454305,7.65,-12.7));
#25923=CARTESIAN_POINT('Ctrl Pts',(-34.1718099032197,7.73530164995786,-12.7));
#25924=CARTESIAN_POINT('Ctrl Pts',(-34.2396185565292,7.82187906279926,-12.6965423806533));
#25925=CARTESIAN_POINT('Ctrl Pts',(-34.3081904207592,7.90943093573856,-12.6893758899384));
#25926=CARTESIAN_POINT('Ctrl Pts',(-34.3771672099234,7.99749981279899,-12.6821670802517));
#25927=CARTESIAN_POINT('Ctrl Pts',(-34.4469161091026,8.0865545122324,-12.6712053060908));
#25928=CARTESIAN_POINT('Ctrl Pts',(-34.5171747421384,8.17626003477469,-12.6562735357966));
#25929=CARTESIAN_POINT('Ctrl Pts',(-34.5883719103702,8.2671638697028,-12.6411423025843));
#25930=CARTESIAN_POINT('Ctrl Pts',(-34.66009235558,8.35873581946203,-12.6219341077298));
#25931=CARTESIAN_POINT('Ctrl Pts',(-34.7320426204516,8.45060120067544,-12.598465486817));
#25932=CARTESIAN_POINT('Ctrl Pts',(-34.804616020137,8.5432621942096,-12.5747936127996));
#25933=CARTESIAN_POINT('Ctrl Pts',(-34.8774230033899,8.63622142491524,-12.5467870597146));
#25934=CARTESIAN_POINT('Ctrl Pts',(-34.9501448392507,8.72907194027922,-12.5143028492619));
#25935=CARTESIAN_POINT('Ctrl Pts',(-35.0238838277916,8.82322114604926,-12.4813642855694));
#25936=CARTESIAN_POINT('Ctrl Pts',(-35.0975349916622,8.91725821815552,-12.4438217748955));
#25937=CARTESIAN_POINT('Ctrl Pts',(-35.1707519133804,9.01074085420895,-12.4015749261073));
#25938=CARTESIAN_POINT('Ctrl Pts',(-35.2152124509763,9.06750762556827,-12.3759207799786));
#25939=CARTESIAN_POINT('Ctrl Pts',(-35.2595126064814,9.12406962267239,-12.3485328867842));
#25940=CARTESIAN_POINT('Ctrl Pts',(-35.3035730360607,9.18032554010333,-12.3193976625566));
#25941=CARTESIAN_POINT('Ctrl Pts',(-35.3743528484633,9.270696499268,-12.2725940856323));
#25942=CARTESIAN_POINT('Ctrl Pts',(-35.4445009330806,9.36026087469156,-12.2212852588861));
#25943=CARTESIAN_POINT('Ctrl Pts',(-35.5137142400593,9.44863173534098,-12.165573946384));
#25944=CARTESIAN_POINT('Ctrl Pts',(-35.5869435953334,9.54213024643472,-12.1066300283126));
#25945=CARTESIAN_POINT('Ctrl Pts',(-35.6591261721559,9.6342922412322,-12.042757601111));
#25946=CARTESIAN_POINT('Ctrl Pts',(-35.7299047145333,9.7246615788413,-11.9741404696194));
#25947=CARTESIAN_POINT('Ctrl Pts',(-35.7986260588343,9.81240430644607,-11.9075177141939));
#25948=CARTESIAN_POINT('Ctrl Pts',(-35.866023469218,9.89845664841804,-11.836422628961));
#25949=CARTESIAN_POINT('Ctrl Pts',(-35.931776733129,9.98240976055746,-11.761076892045));
#25950=CARTESIAN_POINT('Ctrl Pts',(-36.0004825183291,10.0701326224572,-11.682347902663));
#25951=CARTESIAN_POINT('Ctrl Pts',(-36.0673926725241,10.1555628405829,-11.5989779345116));
#25952=CARTESIAN_POINT('Ctrl Pts',(-36.1321559838961,10.2382519911851,-11.5112757977197));
#25953=CARTESIAN_POINT('Ctrl Pts',(-36.1969192952681,10.3209411417873,-11.4235736609278));
#25954=CARTESIAN_POINT('Ctrl Pts',(-36.2595353220431,10.4008886608136,-11.331539792544));
#25955=CARTESIAN_POINT('Ctrl Pts',(-36.319673814854,10.4776728891626,-11.2355339059334));
#25956=CARTESIAN_POINT('Ctrl Pts',(-36.3772994165222,10.5512486831415,-11.1435396320325));
#25957=CARTESIAN_POINT('Ctrl Pts',(-36.4326410435374,10.6219083210428,-11.047913512207));
#25958=CARTESIAN_POINT('Ctrl Pts',(-36.4854998118621,10.6893978697096,-10.9491185834245));
#25959=CARTESIAN_POINT('Ctrl Pts',(-36.5395045498368,10.758350581006,-10.8481817963743));
#25960=CARTESIAN_POINT('Ctrl Pts',(-36.5909172651151,10.8239938235529,-10.7439378175919));
#25961=CARTESIAN_POINT('Ctrl Pts',(-36.6395546932315,10.8860936071067,-10.6369112386827));
#25962=CARTESIAN_POINT('Ctrl Pts',(-36.6867359586466,10.9463341766341,-10.5330889433528));
#25963=CARTESIAN_POINT('Ctrl Pts',(-36.7313055740367,11.0032402174342,-10.4266488425142));
#25964=CARTESIAN_POINT('Ctrl Pts',(-36.7731256175259,11.0566356322302,-10.3180893465301));
#25965=CARTESIAN_POINT('Ctrl Pts',(-36.8145521714388,11.1095286434562,-10.2105512992704));
#25966=CARTESIAN_POINT('Ctrl Pts',(-36.8532805293795,11.1589766249522,-10.1009340887698));
#25967=CARTESIAN_POINT('Ctrl Pts',(-36.8892073412382,11.2048476203274,-9.98973289375452));
#25968=CARTESIAN_POINT('Ctrl Pts',(-36.9245963841465,11.2500319976657,-9.88019620908197));
#25969=CARTESIAN_POINT('Ctrl Pts',(-36.9572670623662,11.2917455940576,-9.76912308215516));
#25970=CARTESIAN_POINT('Ctrl Pts',(-36.9871518459034,11.3299021878797,-9.65698972956914));
#25971=CARTESIAN_POINT('Ctrl Pts',(-36.9910180653701,11.3348385383683,-9.64248294386366));
#25972=CARTESIAN_POINT('Ctrl Pts',(-36.994837701986,11.3397154123373,-9.62795841177471));
#25973=CARTESIAN_POINT('Ctrl Pts',(-36.9986106492175,11.3445326737655,-9.61341716182616));
#25974=CARTESIAN_POINT('Ctrl Pts',(-37.0282507404559,11.3823768468988,-9.49918180449011));
#25975=CARTESIAN_POINT('Ctrl Pts',(-37.0550294404338,11.4165676241844,-9.38394181607375));
#25976=CARTESIAN_POINT('Ctrl Pts',(-37.0789680109407,11.4471321524627,-9.26823244742671));
#25977=CARTESIAN_POINT('Ctrl Pts',(-37.1025632992548,11.4772583814581,-9.15418236606997));
#25978=CARTESIAN_POINT('Ctrl Pts',(-37.1233993879242,11.5038616918423,-9.03967670402529));
#25979=CARTESIAN_POINT('Ctrl Pts',(-37.141526145474,11.5270057552509,-8.9252124146849));
#25980=CARTESIAN_POINT('Ctrl Pts',(-37.1547234940072,11.5438559983481,-8.84187566144162));
#25981=CARTESIAN_POINT('Ctrl Pts',(-37.1664853189077,11.5588733791759,-8.75856053416828));
#25982=CARTESIAN_POINT('Ctrl Pts',(-37.1768406531962,11.5720949668055,-8.67545161008092));
#25983=CARTESIAN_POINT('Ctrl Pts',(-37.1911777621346,11.5904004446303,-8.56038611193216));
#25984=CARTESIAN_POINT('Ctrl Pts',(-37.2028177491878,11.6052622641081,-8.4457198673854));
#25985=CARTESIAN_POINT('Ctrl Pts',(-37.2118962775322,11.6168536386311,-8.33192848403724));
#25986=CARTESIAN_POINT('Ctrl Pts',(-37.2208885087921,11.6283348298965,-8.21921875888853));
#25987=CARTESIAN_POINT('Ctrl Pts',(-37.2273678674517,11.6366076104664,-8.10736762720217));
#25988=CARTESIAN_POINT('Ctrl Pts',(-37.2314899522891,11.6418706473102,-7.99680400773177));
#25989=CARTESIAN_POINT('Ctrl Pts',(-37.2352214310094,11.646634962156,-7.89671732597749));
#25990=CARTESIAN_POINT('Ctrl Pts',(-37.2370215606994,11.6489333498058,-7.79768544011085));
#25991=CARTESIAN_POINT('Ctrl Pts',(-37.2370215606994,11.6489333498058,-7.7));
#25992=CARTESIAN_POINT('Ctrl Pts',(-34.1050004454305,7.65,-12.7));
#25993=CARTESIAN_POINT('Ctrl Pts',(-34.1050004454305,7.65,-12.7));
#25994=CARTESIAN_POINT('Ctrl Pts',(-34.1050004454305,7.65,-12.7));
#25995=CARTESIAN_POINT('Ctrl Pts',(-34.51505495897,8.17355351674855,-12.7));
#25996=CARTESIAN_POINT('Ctrl Pts',(-34.3684200110127,8.23864736688751,-12.7));
#25997=CARTESIAN_POINT('Ctrl Pts',(-34.2221767330303,8.30461645762911,-12.7));
#25998=CARTESIAN_POINT('Ctrl Pts',(-34.9248003596002,8.69671236121437,-12.5698633744286));
#25999=CARTESIAN_POINT('Ctrl Pts',(-34.6344129874201,8.83304537535153,-12.5964281310995));
#26000=CARTESIAN_POINT('Ctrl Pts',(-34.3392646891937,8.95873944331332,-12.569863374429));
#26001=CARTESIAN_POINT('Ctrl Pts',(-35.6823457125229,9.66393871899146,-12.0689319506843));
#26002=CARTESIAN_POINT('Ctrl Pts',(-35.1421214426225,9.96758997398136,-12.1778901074191));
#26003=CARTESIAN_POINT('Ctrl Pts',(-34.5557392046831,10.1680948803376,-12.0689319506839));
#26004=CARTESIAN_POINT('Ctrl Pts',(-36.0297737596905,10.1075313875401,-11.6983341944632));
#26005=CARTESIAN_POINT('Ctrl Pts',(-35.3869447814668,10.5146815062458,-11.8564353766689));
#26006=CARTESIAN_POINT('Ctrl Pts',(-34.6550194892076,10.7227336174029,-11.6983341944626));
#26007=CARTESIAN_POINT('Ctrl Pts',(-36.6095738700227,10.8478143907814,-10.7727336174023));
#26008=CARTESIAN_POINT('Ctrl Pts',(-35.8197142077533,11.4817645043905,-10.9904588000056));
#26009=CARTESIAN_POINT('Ctrl Pts',(-34.8207019100435,11.6483341944626,-10.7727336174029));
#26010=CARTESIAN_POINT('Ctrl Pts',(-36.8417178703408,11.1442135371056,-10.2180948773779));
#26011=CARTESIAN_POINT('Ctrl Pts',(-36.0061527172947,11.8983870794298,-10.439161626936));
#26012=CARTESIAN_POINT('Ctrl Pts',(-34.8870388756109,12.01893195191,-10.2180948773776));
#26013=CARTESIAN_POINT('Ctrl Pts',(-37.0770570386605,11.4446922420908,-9.31107830404926));
#26014=CARTESIAN_POINT('Ctrl Pts',(-36.2030730684665,12.3384327759139,-9.4822033404738));
#26015=CARTESIAN_POINT('Ctrl Pts',(-34.9542888854505,12.3946305178797,-9.31107830404939));
#26016=CARTESIAN_POINT('Ctrl Pts',(-37.1368490307002,11.5210340617088,-8.99641282927347));
#26017=CARTESIAN_POINT('Ctrl Pts',(-36.2546886211114,12.4537748504034,-9.14076955834483));
#26018=CARTESIAN_POINT('Ctrl Pts',(-34.9713749152927,12.4900832460695,-8.99641282927339));
#26019=CARTESIAN_POINT('Ctrl Pts',(-37.2168322756965,11.6231558718975,-8.35449039088781));
#26020=CARTESIAN_POINT('Ctrl Pts',(-36.3245787042157,12.6099538847862,-8.43215085130202));
#26021=CARTESIAN_POINT('Ctrl Pts',(-34.9942307537467,12.6177695579628,-8.3544903908879));
#26022=CARTESIAN_POINT('Ctrl Pts',(-37.2370215607004,11.6489333498047,-8.02725293702977));
#26023=CARTESIAN_POINT('Ctrl Pts',(-36.3424993318365,12.6499999999592,-8.06661933627898));
#26024=CARTESIAN_POINT('Ctrl Pts',(-34.9999999999986,12.65,-8.02725293702971));
#26025=CARTESIAN_POINT('Ctrl Pts',(-37.2370215606994,11.6489333498058,-7.69999999999999));
#26026=CARTESIAN_POINT('Ctrl Pts',(-36.3424993318542,12.65,-7.69999999999999));
#26027=CARTESIAN_POINT('Ctrl Pts',(-35.,12.65,-7.69999999999999));
#26028=CARTESIAN_POINT('Ctrl Pts',(-34.1050004454305,7.65,-12.7));
#26029=CARTESIAN_POINT('Ctrl Pts',(-34.1240917710517,7.75665550347773,-12.7));
#26030=CARTESIAN_POINT('Ctrl Pts',(-34.1434686246157,7.86490613592107,-12.6965423806532));
#26031=CARTESIAN_POINT('Ctrl Pts',(-34.1630635716754,7.97437516838843,-12.689375889938));
#26032=CARTESIAN_POINT('Ctrl Pts',(-34.1827742292053,8.08449062838514,-12.6821670802511));
#26033=CARTESIAN_POINT('Ctrl Pts',(-34.2027055232168,8.19583869503812,-12.6712053060899));
#26034=CARTESIAN_POINT('Ctrl Pts',(-34.2227824776687,8.30800050757273,-12.6562735357951));
#26035=CARTESIAN_POINT('Ctrl Pts',(-34.2431276259006,8.42166061012692,-12.6411423025824));
#26036=CARTESIAN_POINT('Ctrl Pts',(-34.2636223046257,8.53615607898092,-12.6219341077272));
#26037=CARTESIAN_POINT('Ctrl Pts',(-34.2841826561185,8.65101843498767,-12.5984654868138));
#26038=CARTESIAN_POINT('Ctrl Pts',(-34.3049210732628,8.76687557166583,-12.5747936127957));
#26039=CARTESIAN_POINT('Ctrl Pts',(-34.3257262387403,8.88310560424568,-12.5467870597101));
#26040=CARTESIAN_POINT('Ctrl Pts',(-34.3465070726839,8.99919970640085,-12.5143028492565));
#26041=CARTESIAN_POINT('Ctrl Pts',(-34.3675785659692,9.11691760456874,-12.4813642855633));
#26042=CARTESIAN_POINT('Ctrl Pts',(-34.3886249626673,9.23449529826958,-12.4438217748886));
#26043=CARTESIAN_POINT('Ctrl Pts',(-34.4095472712707,9.35137976204587,-12.4015749260995));
#26044=CARTESIAN_POINT('Ctrl Pts',(-34.4222522179732,9.42235715324929,-12.3759207799732));
#26045=CARTESIAN_POINT('Ctrl Pts',(-34.4349113342375,9.49307850835849,-12.3485328867815));
#26046=CARTESIAN_POINT('Ctrl Pts',(-34.4475019469418,9.56341716182414,-12.319397662557));
#26047=CARTESIAN_POINT('Ctrl Pts',(-34.4677278324778,9.67641099200239,-12.2725940856327));
#26048=CARTESIAN_POINT('Ctrl Pts',(-34.4877731968533,9.78839632357546,-12.2212852588866));
#26049=CARTESIAN_POINT('Ctrl Pts',(-34.5075514412001,9.89888936374264,-12.1655739463846));
#26050=CARTESIAN_POINT('Ctrl Pts',(-34.5284773027894,10.0157936766117,-12.1066300283132));
#26051=CARTESIAN_POINT('Ctrl Pts',(-34.5491040392408,10.1310268984931,-12.0427576011116));
#26052=CARTESIAN_POINT('Ctrl Pts',(-34.5693295618572,10.2440187011864,-11.97414046962));
#26053=CARTESIAN_POINT('Ctrl Pts',(-34.5889672240172,10.3537263656172,-11.9075177141948));
#26054=CARTESIAN_POINT('Ctrl Pts',(-34.6082265616951,10.4613204844035,-11.8364226289622));
#26055=CARTESIAN_POINT('Ctrl Pts',(-34.6270160716463,10.5662898659801,-11.7610768920466));
#26056=CARTESIAN_POINT('Ctrl Pts',(-34.6466492876715,10.6759726916567,-11.6823479026645));
#26057=CARTESIAN_POINT('Ctrl Pts',(-34.6657693880788,10.7827889482092,-11.598977934513));
#26058=CARTESIAN_POINT('Ctrl Pts',(-34.6842760113416,10.8861779564385,-11.511275797721));
#26059=CARTESIAN_POINT('Ctrl Pts',(-34.7027826346044,10.9895669646678,-11.423573660929));
#26060=CARTESIAN_POINT('Ctrl Pts',(-34.7206756544822,11.0895280193203,-11.3315397925451));
#26061=CARTESIAN_POINT('Ctrl Pts',(-34.7378606996329,11.1855339059311,-11.2355339059344));
#26062=CARTESIAN_POINT('Ctrl Pts',(-34.7543276664658,11.2775281798313,-11.1435396320343));
#26063=CARTESIAN_POINT('Ctrl Pts',(-34.7701419696601,11.3658762863383,-11.0479135122097));
#26064=CARTESIAN_POINT('Ctrl Pts',(-34.785246776545,11.4502607243403,-10.949118583428));
#26065=CARTESIAN_POINT('Ctrl Pts',(-34.8006790532294,11.5364746034736,-10.8481817963777));
#26066=CARTESIAN_POINT('Ctrl Pts',(-34.8153706391351,11.6185505432366,-10.743937817595));
#26067=CARTESIAN_POINT('Ctrl Pts',(-34.8292691650063,11.6961959778085,-10.6369112386856));
#26068=CARTESIAN_POINT('Ctrl Pts',(-34.8427515809851,11.7715167749529,-10.5330889433564));
#26069=CARTESIAN_POINT('Ctrl Pts',(-34.8554876975223,11.8426682993994,-10.4266488425185));
#26070=CARTESIAN_POINT('Ctrl Pts',(-34.8674381023621,11.9094303708381,-10.3180893465352));
#26071=CARTESIAN_POINT('Ctrl Pts',(-34.8792760644748,11.9755642703044,-10.2105512992764));
#26072=CARTESIAN_POINT('Ctrl Pts',(-34.8903429959641,12.0373907339765,-10.1009340887766));
#26073=CARTESIAN_POINT('Ctrl Pts',(-34.9006093637268,12.0947447723694,-9.98973289376224));
#26074=CARTESIAN_POINT('Ctrl Pts',(-34.9107220598017,12.1512403092858,-9.88019620909055));
#26075=CARTESIAN_POINT('Ctrl Pts',(-34.9200579618845,12.2033962128018,-9.76912308216464));
#26076=CARTESIAN_POINT('Ctrl Pts',(-34.9285977727507,12.2511046771403,-9.65698972957955));
#26077=CARTESIAN_POINT('Ctrl Pts',(-34.9297025752325,12.2572767611162,-9.64248294387071));
#26078=CARTESIAN_POINT('Ctrl Pts',(-34.9307940663001,12.2633744796121,-9.6279584117784));
#26079=CARTESIAN_POINT('Ctrl Pts',(-34.9318722155104,12.269397662556,-9.61341716182647));
#26080=CARTESIAN_POINT('Ctrl Pts',(-34.9403421036365,12.316715496867,-9.49918180449091));
#26081=CARTESIAN_POINT('Ctrl Pts',(-34.9479943268078,12.3594653682635,-9.383941816075));
#26082=CARTESIAN_POINT('Ctrl Pts',(-34.954834960747,12.3976812193477,-9.26823244742841));
#26083=CARTESIAN_POINT('Ctrl Pts',(-34.9615774991121,12.4353490501917,-9.15418236607224));
#26084=CARTESIAN_POINT('Ctrl Pts',(-34.9675315745766,12.4686120581704,-9.03967670402811));
#26085=CARTESIAN_POINT('Ctrl Pts',(-34.9727114374621,12.4975498540576,-8.92521241468831));
#26086=CARTESIAN_POINT('Ctrl Pts',(-34.9764826831285,12.5186182760887,-8.84187566144388));
#26087=CARTESIAN_POINT('Ctrl Pts',(-34.9798437166779,12.5373950091753,-8.75856053416942));
#26088=CARTESIAN_POINT('Ctrl Pts',(-34.9828028345235,12.5539264020161,-8.67545161008097));
#26089=CARTESIAN_POINT('Ctrl Pts',(-34.9868997756487,12.5768143526564,-8.56038611193321));
#26090=CARTESIAN_POINT('Ctrl Pts',(-34.990225993079,12.5953965821887,-8.44571986738742));
#26091=CARTESIAN_POINT('Ctrl Pts',(-34.9928202536293,12.6098896651052,-8.3319284840402));
#26092=CARTESIAN_POINT('Ctrl Pts',(-34.9953898541122,12.6242449822129,-8.21921875889255));
#26093=CARTESIAN_POINT('Ctrl Pts',(-34.997241381576,12.6345887162122,-8.10736762720722));
#26094=CARTESIAN_POINT('Ctrl Pts',(-34.99841929959,12.6411692670538,-7.99680400773782));
#26095=CARTESIAN_POINT('Ctrl Pts',(-34.999485598848,12.6471262491157,-7.89671732598147));
#26096=CARTESIAN_POINT('Ctrl Pts',(-35.,12.65,-7.79768544011281));
#26097=CARTESIAN_POINT('Ctrl Pts',(-35.,12.65,-7.7));
#26098=CARTESIAN_POINT('Origin',(-35.,7.65,-7.7));
#26099=CARTESIAN_POINT('Origin',(-17.9697662756086,7.65,-7.7));
#26100=CARTESIAN_POINT('Ctrl Pts',(-17.9697662756086,12.65,-7.7));
#26101=CARTESIAN_POINT('Ctrl Pts',(-17.9697662756086,12.65,-12.7));
#26102=CARTESIAN_POINT('Ctrl Pts',(-17.9697662756086,7.65,-12.7));
#26103=CARTESIAN_POINT('Ctrl Pts',(-17.8786433834317,12.65,-7.82930352963403));
#26104=CARTESIAN_POINT('Ctrl Pts',(-17.8797974234738,12.5223340542632,-12.7));
#26105=CARTESIAN_POINT('Ctrl Pts',(-17.5769226509335,7.65000000135137,-12.7));
#26106=CARTESIAN_POINT('Ctrl Pts',(-17.7836615819991,12.6532040193819,-7.96407165192472));
#26107=CARTESIAN_POINT('Ctrl Pts',(-17.7621458420662,12.4006679911028,-12.7));
#26108=CARTESIAN_POINT('Ctrl Pts',(-17.1871178707085,7.68525114336134,-12.7));
#26109=CARTESIAN_POINT('Ctrl Pts',(-17.6839681951541,12.6595351585866,-8.1049008253337));
#26110=CARTESIAN_POINT('Ctrl Pts',(-17.617785931914,12.2921100651331,-12.7));
#26111=CARTESIAN_POINT('Ctrl Pts',(-16.8005208252602,7.75488674445212,-12.7));
#26112=CARTESIAN_POINT('Origin',(-16.8005208252602,7.75488674445212,-7.7));
#26113=CARTESIAN_POINT('Ctrl Pts',(-17.6839681951541,12.6595351585866,-8.1049008253337));
#26114=CARTESIAN_POINT('Ctrl Pts',(-17.617785931914,12.2921100651331,-12.7));
#26115=CARTESIAN_POINT('Ctrl Pts',(-16.8005208252602,7.75488674445212,-12.7));
#26116=CARTESIAN_POINT('Ctrl Pts',(-17.5771561971189,12.6663183729863,-8.25578591414162));
#26117=CARTESIAN_POINT('Ctrl Pts',(-17.6289209271536,12.15209358202,-12.6705607830935));
#26118=CARTESIAN_POINT('Ctrl Pts',(-16.5687698658206,7.82950008896473,-12.7));
#26119=CARTESIAN_POINT('Ctrl Pts',(-17.4598936459479,12.6763099143986,-8.4291699077561));
#26120=CARTESIAN_POINT('Ctrl Pts',(-17.5782752445044,12.013218333086,-12.6289627825015));
#26121=CARTESIAN_POINT('Ctrl Pts',(-16.3458206877549,7.93940906195254,-12.7125729192313));
#26122=CARTESIAN_POINT('Ctrl Pts',(-17.1998888841757,12.7012381622111,-8.81799222980845));
#26123=CARTESIAN_POINT('Ctrl Pts',(-17.3662719339354,11.7832074074828,-12.5586541771898));
#26124=CARTESIAN_POINT('Ctrl Pts',(-15.9135842369118,8.21361978075451,-12.7584916190665));
#26125=CARTESIAN_POINT('Ctrl Pts',(-17.0571441869795,12.7161912440269,-9.03346319244822));
#26126=CARTESIAN_POINT('Ctrl Pts',(-17.2098830150751,11.6912659624442,-12.5297453843541));
#26127=CARTESIAN_POINT('Ctrl Pts',(-15.7043519652416,8.37810368845214,-12.7918748657651));
#26128=CARTESIAN_POINT('Ctrl Pts',(-16.7409348394768,12.7502046526729,-9.50326306101304));
#26129=CARTESIAN_POINT('Ctrl Pts',(-16.8220227865866,11.5747870675349,-12.5075269194728));
#26130=CARTESIAN_POINT('Ctrl Pts',(-15.2973824695118,8.75225117524501,-12.8769706424726));
#26131=CARTESIAN_POINT('Ctrl Pts',(-16.5677687617376,12.7692327202595,-9.75697351939234));
#26132=CARTESIAN_POINT('Ctrl Pts',(-16.5938533615665,11.5484270002405,-12.5132837475877));
#26133=CARTESIAN_POINT('Ctrl Pts',(-15.1005185854711,8.96155992656123,-12.9286629823072));
#26134=CARTESIAN_POINT('Ctrl Pts',(-16.1973605868977,12.8095022395595,-10.2822412234627));
#26135=CARTESIAN_POINT('Ctrl Pts',(-16.1105390364457,11.5605687167964,-12.5667216513117));
#26136=CARTESIAN_POINT('Ctrl Pts',(-14.7269130064669,9.40452463144808,-13.0449250534816));
#26137=CARTESIAN_POINT('Ctrl Pts',(-15.998896046405,12.8308799157883,-10.5556257828799));
#26138=CARTESIAN_POINT('Ctrl Pts',(-15.8541814468065,11.5962530038123,-12.6128339202831));
#26139=CARTESIAN_POINT('Ctrl Pts',(-14.5485608660789,9.63967907679423,-13.1098286335377));
#26140=CARTESIAN_POINT('Ctrl Pts',(-15.573397634044,12.87554153991,-11.1172708424565));
#26141=CARTESIAN_POINT('Ctrl Pts',(-15.3333943403924,11.7180448914412,-12.7448433212756));
#26142=CARTESIAN_POINT('Ctrl Pts',(-14.2053991112487,10.1309569358866,-13.2515258205145));
#26143=CARTESIAN_POINT('Ctrl Pts',(-15.3463523739799,12.8988286442761,-11.4055303863304));
#26144=CARTESIAN_POINT('Ctrl Pts',(-15.0678470816742,11.8029800287259,-12.829901640401));
#26145=CARTESIAN_POINT('Ctrl Pts',(-14.0406084083384,10.3871150892957,-13.3283300196113));
#26146=CARTESIAN_POINT('Ctrl Pts',(-14.8628607081636,12.9468769497922,-11.9898209804218));
#26147=CARTESIAN_POINT('Ctrl Pts',(-14.5414297968434,12.0098985669587,-13.0365151718341));
#26148=CARTESIAN_POINT('Ctrl Pts',(-13.722266387327,10.9156464454547,-13.4931147637453));
#26149=CARTESIAN_POINT('Ctrl Pts',(-14.6063601361617,12.9716383743557,-12.2857804525791));
#26150=CARTESIAN_POINT('Ctrl Pts',(-14.2788785559446,12.1317581217325,-13.1579975413437));
#26151=CARTESIAN_POINT('Ctrl Pts',(-13.568789765243,11.1880221188636,-13.5811194448631));
#26152=CARTESIAN_POINT('Ctrl Pts',(-13.8028973740084,13.0467768755486,-13.1649381963916));
#26153=CARTESIAN_POINT('Ctrl Pts',(-13.5233243480122,12.5265039443217,-13.5643970241019));
#26154=CARTESIAN_POINT('Ctrl Pts',(-13.1270902810059,12.0145456291354,-13.8587218607487));
#26155=CARTESIAN_POINT('Ctrl Pts',(-13.2185390460369,13.0982771986992,-13.7423443295298));
#26156=CARTESIAN_POINT('Ctrl Pts',(-13.0367148554586,12.8398642053082,-13.902698193065));
#26157=CARTESIAN_POINT('Ctrl Pts',(-12.8553998351504,12.5811750652043,-14.0626030106305));
#26158=CARTESIAN_POINT('Ctrl Pts',(-12.6003906189451,13.15,-14.2875));
#26159=CARTESIAN_POINT('Ctrl Pts',(-12.6003906189451,13.15,-14.2875));
#26160=CARTESIAN_POINT('Ctrl Pts',(-12.6003906189451,13.15,-14.2875));
#26161=CARTESIAN_POINT('Origin',(30.6683956091404,-22.9,-37.7192193816529));
#26162=CARTESIAN_POINT('Origin',(30.6683956091404,-21.9,-37.7192193816529));
#26163=CARTESIAN_POINT('Origin',(30.6683956091404,-7.90000000000001,-37.7192193816529));
#26164=CARTESIAN_POINT('Origin',(30.6683956091404,-7.90000000000001,-37.7192193816529));
#26165=CARTESIAN_POINT('Origin',(30.6683956091404,-7.90000000000001,-37.7192193816529));
#26166=CARTESIAN_POINT('Origin',(30.6683956091404,-7.90000000000001,-37.7192193816529));
#26167=CARTESIAN_POINT('Ctrl Pts',(28.0510228507777,7.65,-23.1857967818223));
#26168=CARTESIAN_POINT('Ctrl Pts',(28.0844275796734,7.7353016499602,-23.2436554694827));
#26169=CARTESIAN_POINT('Ctrl Pts',(28.1153375201382,7.82187906280401,-23.3041082955204));
#26170=CARTESIAN_POINT('Ctrl Pts',(28.1434170892388,7.90943093574576,-23.3670765172878));
#26171=CARTESIAN_POINT('Ctrl Pts',(28.1716624715019,7.99749981280845,-23.4304165738206));
#26172=CARTESIAN_POINT('Ctrl Pts',(28.197043746198,8.08655451224417,-23.4963017794781));
#26173=CARTESIAN_POINT('Ctrl Pts',(28.2192417703178,8.17626003478879,-23.5646134256713));
#26174=CARTESIAN_POINT('Ctrl Pts',(28.2417363220814,8.26716386971868,-23.6338375986452));
#26175=CARTESIAN_POINT('Ctrl Pts',(28.2609617599813,8.35873581947972,-23.7055534235965));
#26176=CARTESIAN_POINT('Ctrl Pts',(28.2766124705147,8.45060120069494,-23.7795984912424));
#26177=CARTESIAN_POINT('Ctrl Pts',(28.2923987261027,8.5432621942306,-23.854284836019));
#26178=CARTESIAN_POINT('Ctrl Pts',(28.3045478312848,8.63622142493773,-23.9313408096329));
#26179=CARTESIAN_POINT('Ctrl Pts',(28.3127765977406,8.72907194030321,-24.0105618721263));
#26180=CARTESIAN_POINT('Ctrl Pts',(28.3211204590885,8.82322114607408,-24.0908909912993));
#26181=CARTESIAN_POINT('Ctrl Pts',(28.3254332730576,8.91725821818117,-24.1734460255676));
#26182=CARTESIAN_POINT('Ctrl Pts',(28.3254548896355,9.01074085423544,-24.2579771641579));
#26183=CARTESIAN_POINT('Ctrl Pts',(28.3254680161731,9.06750762558578,-24.3093081922384));
#26184=CARTESIAN_POINT('Ctrl Pts',(28.3238994826631,9.12406962268099,-24.3613671988867));
#26185=CARTESIAN_POINT('Ctrl Pts',(28.3206978531272,9.18032554010316,-24.4140922623098));
#26186=CARTESIAN_POINT('Ctrl Pts',(28.3155546727241,9.27069649926788,-24.4987911663879));
#26187=CARTESIAN_POINT('Ctrl Pts',(28.3061939676322,9.36026087469145,-24.5851956030667));
#26188=CARTESIAN_POINT('Ctrl Pts',(28.2925532092166,9.44863173534083,-24.6729917414413));
#26189=CARTESIAN_POINT('Ctrl Pts',(28.2781209564053,9.54213024643462,-24.7658821824474));
#26190=CARTESIAN_POINT('Ctrl Pts',(28.2588971002586,9.63429224123211,-24.8603303412872));
#26191=CARTESIAN_POINT('Ctrl Pts',(28.2348621924407,9.72466157884118,-24.9559349227747));
#26192=CARTESIAN_POINT('Ctrl Pts',(28.2115258659228,9.81240430644562,-25.048760730434));
#26193=CARTESIAN_POINT('Ctrl Pts',(28.1836544212187,9.89845664841724,-25.1426761425918));
#26194=CARTESIAN_POINT('Ctrl Pts',(28.1512797309383,9.98240976055632,-25.2372930079781));
#26195=CARTESIAN_POINT('Ctrl Pts',(28.1174513187192,10.0701326224562,-25.3361584580394));
#26196=CARTESIAN_POINT('Ctrl Pts',(28.0787058854849,10.1555628405819,-25.4357893354192));
#26197=CARTESIAN_POINT('Ctrl Pts',(28.0351352627429,10.2382519911843,-25.5357270766966));
#26198=CARTESIAN_POINT('Ctrl Pts',(27.9915646400008,10.3209411417866,-25.6356648179739));
#26199=CARTESIAN_POINT('Ctrl Pts',(27.9431689853593,10.4008886608129,-25.735908822037));
#26200=CARTESIAN_POINT('Ctrl Pts',(27.8900946950471,10.4776728891621,-25.8359932278618));
#26201=CARTESIAN_POINT('Ctrl Pts',(27.8392381176804,10.5512486831409,-25.9318955997651));
#26202=CARTESIAN_POINT('Ctrl Pts',(27.7840942821539,10.621908321042,-26.0276359145594));
#26203=CARTESIAN_POINT('Ctrl Pts',(27.7249647482256,10.6893978697086,-26.1228104151325));
#26204=CARTESIAN_POINT('Ctrl Pts',(27.6645532954511,10.758350581005,-26.2200482836684));
#26205=CARTESIAN_POINT('Ctrl Pts',(27.599981719273,10.8239938235519,-26.3166949905683));
#26206=CARTESIAN_POINT('Ctrl Pts',(27.5316126971157,10.8860936071058,-26.4123295283466));
#26207=CARTESIAN_POINT('Ctrl Pts',(27.4652905845885,10.9463341766329,-26.5051008504436));
#26208=CARTESIAN_POINT('Ctrl Pts',(27.3953955609761,11.0032402174329,-26.5969193200274));
#26209=CARTESIAN_POINT('Ctrl Pts',(27.3222903013767,11.0566356322287,-26.6874162880683));
#26210=CARTESIAN_POINT('Ctrl Pts',(27.2498728975334,11.1095286434545,-26.7770617597774));
#26211=CARTESIAN_POINT('Ctrl Pts',(27.1743057875187,11.1589766249502,-26.8654101068509));
#26212=CARTESIAN_POINT('Ctrl Pts',(27.0959661336342,11.2048476203253,-26.9521242361045));
#26213=CARTESIAN_POINT('Ctrl Pts',(27.0187991035163,11.2500319976632,-27.0375403886143));
#26214=CARTESIAN_POINT('Ctrl Pts',(26.9389422930305,11.291745594055,-27.1213705893742));
#26215=CARTESIAN_POINT('Ctrl Pts',(26.8567743528488,11.329902187877,-27.2033182473963));
#26216=CARTESIAN_POINT('Ctrl Pts',(26.8461442176325,11.3348385383663,-27.2139198845252));
#26217=CARTESIAN_POINT('Ctrl Pts',(26.8354754221718,11.3397154123361,-27.2244900529138));
#26218=CARTESIAN_POINT('Ctrl Pts',(26.8247688039278,11.3445326737649,-27.2350281460392));
#26219=CARTESIAN_POINT('Ctrl Pts',(26.7406581280853,11.3823768468976,-27.3178148966883));
#26220=CARTESIAN_POINT('Ctrl Pts',(26.6542467205756,11.4165676241826,-27.3986259253561));
#26221=CARTESIAN_POINT('Ctrl Pts',(26.5660087531266,11.4471321524605,-27.4772120198674));
#26222=CARTESIAN_POINT('Ctrl Pts',(26.4790361295275,11.4772583814553,-27.5546711796333));
#26223=CARTESIAN_POINT('Ctrl Pts',(26.3902893616569,11.503861691839,-27.6299685927569));
#26224=CARTESIAN_POINT('Ctrl Pts',(26.3002237580396,11.5270057552473,-27.7028989699517));
#26225=CARTESIAN_POINT('Ctrl Pts',(26.2346506869243,11.5438559983458,-27.7559965856693));
#26226=CARTESIAN_POINT('Ctrl Pts',(26.168378582632,11.5588733791746,-27.8078401884682));
#26227=CARTESIAN_POINT('Ctrl Pts',(26.101581810231,11.5720949668051,-27.8583626330737));
#26228=CARTESIAN_POINT('Ctrl Pts',(26.0091007202041,11.59040044463,-27.9283116827057));
#26229=CARTESIAN_POINT('Ctrl Pts',(25.9156168329965,11.6052622641078,-27.995725329467));
#26230=CARTESIAN_POINT('Ctrl Pts',(25.8216098684572,11.6168536386309,-28.0604832573163));
#26231=CARTESIAN_POINT('Ctrl Pts',(25.7284964988546,11.6283348298964,-28.1246256205985));
#26232=CARTESIAN_POINT('Ctrl Pts',(25.6348702567017,11.6366076104663,-28.1861624756413));
#26233=CARTESIAN_POINT('Ctrl Pts',(25.5411803959244,11.6418706473102,-28.2450141155623));
#26234=CARTESIAN_POINT('Ctrl Pts',(25.4563685263053,11.646634962156,-28.2982890118046));
#26235=CARTESIAN_POINT('Ctrl Pts',(25.3715044622055,11.6489333498058,-28.3493639127792));
#26236=CARTESIAN_POINT('Ctrl Pts',(25.28690638949,11.6489333498058,-28.3982066328344));
#26237=CARTESIAN_POINT('Ctrl Pts',(28.0510228507777,7.65,-23.1857967818223));
#26238=CARTESIAN_POINT('Ctrl Pts',(28.0510228507777,7.65,-23.1857967818223));
#26239=CARTESIAN_POINT('Ctrl Pts',(28.0510228507777,7.65,-23.1857967818223));
#26240=CARTESIAN_POINT('Ctrl Pts',(28.2560501075485,8.17355351674861,-23.5409144074858));
#26241=CARTESIAN_POINT('Ctrl Pts',(28.1827326335689,8.23864736688846,-23.4139248174704));
#26242=CARTESIAN_POINT('Ctrl Pts',(28.1096109945771,8.30461645762955,-23.2872744236039));
#26243=CARTESIAN_POINT('Ctrl Pts',(28.3482211841548,8.69671236121348,-23.9608326462974));
#26244=CARTESIAN_POINT('Ctrl Pts',(28.226033252186,8.83304537535178,-23.6960674267144));
#26245=CARTESIAN_POINT('Ctrl Pts',(28.0554533489517,8.95873944331314,-23.4537438809043));
#26246=CARTESIAN_POINT('Ctrl Pts',(28.2931745221,9.66393871899236,-24.8673518783231));
#26247=CARTESIAN_POINT('Ctrl Pts',(28.1174229188328,9.96758997398111,-24.3450248584826));
#26248=CARTESIAN_POINT('Ctrl Pts',(27.72987126818,10.1680948803378,-23.8916820224642));
#26249=CARTESIAN_POINT('Ctrl Pts',(28.1459414742105,10.1075313875402,-25.3535322712673));
#26250=CARTESIAN_POINT('Ctrl Pts',(27.9614466252583,10.5146815062458,-24.7177754547341));
#26251=CARTESIAN_POINT('Ctrl Pts',(27.4585643389691,10.7227336174028,-24.1629601490677));
#26252=CARTESIAN_POINT('Ctrl Pts',(27.6342479158847,10.8478143907813,-26.3184541844604));
#26253=CARTESIAN_POINT('Ctrl Pts',(27.4278736239269,11.4817645043905,-25.5255530602085));
#26254=CARTESIAN_POINT('Ctrl Pts',(26.739811935895,11.6483341944627,-24.7692456230009));
#26255=CARTESIAN_POINT('Ctrl Pts',(27.2699886772589,11.1442135371053,-26.7968161560865));
#26256=CARTESIAN_POINT('Ctrl Pts',(27.0436555217853,11.8983870794305,-25.9626621322513));
#26257=CARTESIAN_POINT('Ctrl Pts',(26.2926491798934,12.0189319519104,-25.1040144904059));
#26258=CARTESIAN_POINT('Ctrl Pts',(26.6021588672634,11.4446922420909,-27.4541341410193));
#26259=CARTESIAN_POINT('Ctrl Pts',(26.3133655109336,12.3384327759135,-26.6116793021192));
#26260=CARTESIAN_POINT('Ctrl Pts',(25.5407747906587,12.3946305178795,-25.6157629939952));
#26261=CARTESIAN_POINT('Ctrl Pts',(26.3595465684333,11.5210340617089,-27.6632482624569));
#26262=CARTESIAN_POINT('Ctrl Pts',(26.0434829582226,12.4537748504032,-26.8270965730051));
#26263=CARTESIAN_POINT('Ctrl Pts',(25.2768095107295,12.4900832460694,-25.7878926672764));
#26264=CARTESIAN_POINT('Ctrl Pts',(25.8436170520302,11.6231558718974,-28.0534770036939));
#26265=CARTESIAN_POINT('Ctrl Pts',(25.4647461978775,12.6099538847864,-27.2419325139664));
#26266=CARTESIAN_POINT('Ctrl Pts',(24.7323162910554,12.6177695579629,-26.1286476231954));
#26267=CARTESIAN_POINT('Ctrl Pts',(25.5703157464213,11.6489333498049,-28.2345801643203));
#26268=CARTESIAN_POINT('Ctrl Pts',(25.1571469337947,12.6499999999603,-27.4402179902493));
#26269=CARTESIAN_POINT('Ctrl Pts',(24.4518049660702,12.65,-26.2972626639387));
#26270=CARTESIAN_POINT('Ctrl Pts',(25.28690638949,11.6489333498058,-28.3982066328345));
#26271=CARTESIAN_POINT('Ctrl Pts',(24.8396452750674,12.65,-27.6235276584047));
#26272=CARTESIAN_POINT('Ctrl Pts',(24.1683956091403,12.65,-26.4608891324552));
#26273=CARTESIAN_POINT('Ctrl Pts',(28.0510228507777,7.65,-23.1857967818223));
#26274=CARTESIAN_POINT('Ctrl Pts',(28.0605685135883,7.75665550347771,-23.202330354802));
#26275=CARTESIAN_POINT('Ctrl Pts',(28.0672625541792,7.86490613592101,-23.2208400119071));
#26276=CARTESIAN_POINT('Ctrl Pts',(28.0708536646936,7.97437516838833,-23.241392979204));
#26277=CARTESIAN_POINT('Ctrl Pts',(28.0744659811386,8.084490628385,-23.2620673141935));
#26278=CARTESIAN_POINT('Ctrl Pts',(28.0749384532501,8.19583869503793,-23.2848092082182));
#26279=CARTESIAN_POINT('Ctrl Pts',(28.0720456380772,8.30800050757249,-23.3096622459514));
#26280=CARTESIAN_POINT('Ctrl Pts',(28.0691141798403,8.42166061012672,-23.3348472777702));
#26281=CARTESIAN_POINT('Ctrl Pts',(28.0627267344974,8.53615607898074,-23.362200287616));
#26282=CARTESIAN_POINT('Ctrl Pts',(28.0526824883409,8.65101843498752,-23.3917403847761));
#26283=CARTESIAN_POINT('Ctrl Pts',(28.0425512526582,8.76687557166562,-23.4215363178663));
#26284=CARTESIAN_POINT('Ctrl Pts',(28.0286994489523,8.8831056042454,-23.4535573962425));
#26285=CARTESIAN_POINT('Ctrl Pts',(28.0109577144494,8.99919970640052,-23.4877962315763));
#26286=CARTESIAN_POINT('Ctrl Pts',(27.9929678281695,9.11691760456845,-23.5225139619035));
#26287=CARTESIAN_POINT('Ctrl Pts',(27.9709782585524,9.23449529826935,-23.5595119314396));
#26288=CARTESIAN_POINT('Ctrl Pts',(27.9448525685729,9.35137976204572,-23.5987546065905));
#26289=CARTESIAN_POINT('Ctrl Pts',(27.9289878996663,9.42235715324939,-23.6225844862518));
#26290=CARTESIAN_POINT('Ctrl Pts',(27.9115988465383,9.49307850835886,-23.6472415491221));
#26291=CARTESIAN_POINT('Ctrl Pts',(27.892662308567,9.56341716182476,-23.6727129516856));
#26292=CARTESIAN_POINT('Ctrl Pts',(27.8622421647305,9.67641099200318,-23.713630870836));
#26293=CARTESIAN_POINT('Ctrl Pts',(27.8278300995177,9.7883963235764,-23.7566450789865));
#26294=CARTESIAN_POINT('Ctrl Pts',(27.7894718097861,9.8988893637437,-23.8016291972841));
#26295=CARTESIAN_POINT('Ctrl Pts',(27.7488878101323,10.0157936766128,-23.8492234840522));
#26296=CARTESIAN_POINT('Ctrl Pts',(27.7038860338,10.1310268984941,-23.8990229754171));
#26297=CARTESIAN_POINT('Ctrl Pts',(27.6545746161017,10.2440187011874,-23.9508473575535));
#26298=CARTESIAN_POINT('Ctrl Pts',(27.6066964485132,10.3537263656184,-24.0011654495676));
#26299=CARTESIAN_POINT('Ctrl Pts',(27.5547559674564,10.4613204844049,-24.0533920678732));
#26300=CARTESIAN_POINT('Ctrl Pts',(27.4988994001961,10.5662898659816,-24.1073371292734));
#26301=CARTESIAN_POINT('Ctrl Pts',(27.4405347033895,10.675972691658,-24.1637044878002));
#26302=CARTESIAN_POINT('Ctrl Pts',(27.3778942432613,10.7827889482103,-24.2219479645514));
#26303=CARTESIAN_POINT('Ctrl Pts',(27.3111952764647,10.8861779564394,-24.2818262388311));
#26304=CARTESIAN_POINT('Ctrl Pts',(27.244496309668,10.9895669646686,-24.3417045131109));
#26305=CARTESIAN_POINT('Ctrl Pts',(27.173739151578,11.0895280193209,-24.4032172570673));
#26306=CARTESIAN_POINT('Ctrl Pts',(27.0991881374357,11.1855339059316,-24.4661028860382));
#26307=CARTESIAN_POINT('Ctrl Pts',(27.0277522426516,11.2775281798321,-24.526360834589));
#26308=CARTESIAN_POINT('Ctrl Pts',(26.952844745215,11.3658762863394,-24.587869482811));
#26309=CARTESIAN_POINT('Ctrl Pts',(26.8748382305671,11.4502607243417,-24.6503480936837));
#26310=CARTESIAN_POINT('Ctrl Pts',(26.7951405471474,11.5364746034749,-24.7141812308558));
#26311=CARTESIAN_POINT('Ctrl Pts',(26.712208406283,11.6185505432378,-24.7790265068635));
#26312=CARTESIAN_POINT('Ctrl Pts',(26.626469933003,11.6961959778096,-24.8445762727979));
#26313=CARTESIAN_POINT('Ctrl Pts',(26.543298395758,11.771516774954,-24.9081635352047));
#26314=CARTESIAN_POINT('Ctrl Pts',(26.4574866227195,11.8426682994006,-24.9724133860907));
#26315=CARTESIAN_POINT('Ctrl Pts',(26.3694465437957,11.9094303708394,-25.0370424882595));
#26316=CARTESIAN_POINT('Ctrl Pts',(26.2822348440526,11.9755642703057,-25.1010634878077));
#26317=CARTESIAN_POINT('Ctrl Pts',(26.1928370208126,12.0373907339777,-25.1654563368694));
#26318=CARTESIAN_POINT('Ctrl Pts',(26.1016671448805,12.0947447723705,-25.2299478696638));
#26319=CARTESIAN_POINT('Ctrl Pts',(26.0118619413461,12.1512403092868,-25.2934740637013));
#26320=CARTESIAN_POINT('Ctrl Pts',(25.9203377427922,12.2033962128026,-25.3570957555352));
#26321=CARTESIAN_POINT('Ctrl Pts',(25.8274973162754,12.2511046771409,-25.4205581249814));
#26322=CARTESIAN_POINT('Ctrl Pts',(25.8154864725656,12.2572767611166,-25.428768304851));
#26323=CARTESIAN_POINT('Ctrl Pts',(25.8034536043298,12.2633744796123,-25.4369758298894));
#26324=CARTESIAN_POINT('Ctrl Pts',(25.7913995870742,12.269397662556,-25.4451801594703));
#26325=CARTESIAN_POINT('Ctrl Pts',(25.6967038096758,12.3167154968663,-25.5096329764217));
#26326=CARTESIAN_POINT('Ctrl Pts',(25.6007291637629,12.3594653682623,-25.5738799902906));
#26327=CARTESIAN_POINT('Ctrl Pts',(25.50394222803,12.397681219346,-25.6376588373824));
#26328=CARTESIAN_POINT('Ctrl Pts',(25.4085432294565,12.4353490501894,-25.7005230875694));
#26329=CARTESIAN_POINT('Ctrl Pts',(25.3123554549835,12.4686120581676,-25.7629322991986));
#26330=CARTESIAN_POINT('Ctrl Pts',(25.2158164040339,12.4975498540546,-25.8246503367143));
#26331=CARTESIAN_POINT('Ctrl Pts',(25.1455302814851,12.5186182760868,-25.8695847078898));
#26332=CARTESIAN_POINT('Ctrl Pts',(25.0750577815173,12.5373950091745,-25.914153011966));
#26333=CARTESIAN_POINT('Ctrl Pts',(25.0045629008949,12.5539264020161,-25.9582701452394));
#26334=CARTESIAN_POINT('Ctrl Pts',(24.906961726961,12.5768143526567,-26.0193509494066));
#26335=CARTESIAN_POINT('Ctrl Pts',(24.8093209549414,12.5953965821892,-26.0795646604735));
#26336=CARTESIAN_POINT('Ctrl Pts',(24.7120718565046,12.6098896651059,-26.1387070476885));
#26337=CARTESIAN_POINT('Ctrl Pts',(24.6157471715131,12.6242449822136,-26.1972872495588));
#26338=CARTESIAN_POINT('Ctrl Pts',(24.519807013762,12.6345887162129,-26.2548162852217));
#26339=CARTESIAN_POINT('Ctrl Pts',(24.4246450695727,12.6411692670544,-26.3111182018807));
#26340=CARTESIAN_POINT('Ctrl Pts',(24.3385006102231,12.6471262491159,-26.3620849850025));
#26341=CARTESIAN_POINT('Ctrl Pts',(24.252993681855,12.65,-26.4120464124005));
#26342=CARTESIAN_POINT('Ctrl Pts',(24.1683956091403,12.65,-26.4608891324552));
#26343=CARTESIAN_POINT('Origin',(24.1683956091403,7.65,-26.4608891324553));
#26344=CARTESIAN_POINT('Origin',(15.6532787469445,7.65,-11.7122740947458));
#26345=CARTESIAN_POINT('Ctrl Pts',(15.6532787469445,12.65,-11.7122740947458));
#26346=CARTESIAN_POINT('Ctrl Pts',(19.9834057658667,12.65,-9.21227409474583));
#26347=CARTESIAN_POINT('Ctrl Pts',(19.9834057658667,7.65,-9.21227409474583));
#26348=CARTESIAN_POINT('Ctrl Pts',(15.7196974423161,12.65,-11.5687075904364));
#26349=CARTESIAN_POINT('Ctrl Pts',(19.9384213397983,12.5223340542639,-9.13435878324517));
#26350=CARTESIAN_POINT('Ctrl Pts',(19.7869839535292,7.65000000135137,-8.8720615360625));
#26351=CARTESIAN_POINT('Ctrl Pts',(15.7889191591276,12.6532040193816,-11.4190668763549));
#26352=CARTESIAN_POINT('Ctrl Pts',(19.8795955490932,12.4006679911038,-9.03246952495588));
#26353=CARTESIAN_POINT('Ctrl Pts',(19.5920815634166,7.68525114336099,-8.53448069387081));
#26354=CARTESIAN_POINT('Ctrl Pts',(15.8610341074696,12.6595351585866,-11.2623152840526));
#26355=CARTESIAN_POINT('Ctrl Pts',(19.8074155940194,12.2921100651331,-8.90745017547355));
#26356=CARTESIAN_POINT('Ctrl Pts',(19.3987830406925,7.75488674445212,-8.19967783148469));
#26357=CARTESIAN_POINT('Origin',(15.0686560217703,7.75488674445212,-10.6996778314847));
#26358=CARTESIAN_POINT('Ctrl Pts',(15.8610341074696,12.6595351585866,-11.2623152840526));
#26359=CARTESIAN_POINT('Ctrl Pts',(19.8074155940194,12.2921100651332,-8.90745017547354));
#26360=CARTESIAN_POINT('Ctrl Pts',(19.3987830406925,7.75488674445212,-8.19967783148469));
#26361=CARTESIAN_POINT('Ctrl Pts',(15.9382984284129,12.6663183729861,-11.0943708359216));
#26362=CARTESIAN_POINT('Ctrl Pts',(19.7874879819338,12.1520935820195,-8.93181297267561));
#26363=CARTESIAN_POINT('Ctrl Pts',(19.2829075609725,7.82950008896404,-7.99897561325821));
#26364=CARTESIAN_POINT('Ctrl Pts',(16.0298220959059,12.6763099143987,-10.9061264908871));
#26365=CARTESIAN_POINT('Ctrl Pts',(19.7261402153455,12.0132183330864,-8.90875152520499));
#26366=CARTESIAN_POINT('Ctrl Pts',(19.1823214393941,7.93940906195289,-7.79960950168563));
#26367=CARTESIAN_POINT('Ctrl Pts',(16.236549723476,12.701238162211,-10.4865446010616));
#26368=CARTESIAN_POINT('Ctrl Pts',(19.5592495217588,11.7832074074825,-8.76030557522187));
#26369=CARTESIAN_POINT('Ctrl Pts',(19.0059699745382,8.21361978075416,-7.40232240489545));
#26370=CARTESIAN_POINT('Ctrl Pts',(16.3517807023014,12.7161912440271,-10.2551885857138));
#26371=CARTESIAN_POINT('Ctrl Pts',(19.4560193133398,11.6912659624446,-8.63932319503599));
#26372=CARTESIAN_POINT('Ctrl Pts',(18.9302645784051,8.37810368845214,-7.2044303189888));
#26373=CARTESIAN_POINT('Ctrl Pts',(16.6005346494223,12.7502046526726,-9.74644332358053));
#26374=CARTESIAN_POINT('Ctrl Pts',(19.2428474440738,11.5747870675345,-8.3145356164884));
#26375=CARTESIAN_POINT('Ctrl Pts',(18.8004749349236,8.752251175245,-6.80943650876738));
#26376=CARTESIAN_POINT('Ctrl Pts',(16.7336713127152,12.7692327202591,-9.46962187199463));
#26377=CARTESIAN_POINT('Ctrl Pts',(19.1337482909567,11.5484270002398,-8.11405668399569));
#26378=CARTESIAN_POINT('Ctrl Pts',(18.7468098723811,8.96155992656123,-6.61310121418329));
#26379=CARTESIAN_POINT('Ctrl Pts',(17.0033624008067,12.8095022395598,-8.8862051307789));
#26380=CARTESIAN_POINT('Ctrl Pts',(18.9383697105472,11.5605687167971,-7.66877524856764));
#26381=CARTESIAN_POINT('Ctrl Pts',(18.6606929900126,9.40452463144807,-6.23141825618296));
#26382=CARTESIAN_POINT('Ctrl Pts',(17.1408881040185,12.8308799157881,-8.57763751725331));
#26383=CARTESIAN_POINT('Ctrl Pts',(18.8501253120837,11.5962530038116,-7.42370692900014));
#26384=CARTESIAN_POINT('Ctrl Pts',(18.6277250689438,9.63967907679459,-6.04450898175927));
#26385=CARTESIAN_POINT('Ctrl Pts',(17.4145377873414,12.8755415399101,-7.92832255308998));
#26386=CARTESIAN_POINT('Ctrl Pts',(18.7040552536722,11.7180448914419,-6.90668736438696));
#26387=CARTESIAN_POINT('Ctrl Pts',(18.5788575550954,10.1309569358863,-5.67647359098107));
#26388=CARTESIAN_POINT('Ctrl Pts',(17.5506552451877,12.8988286442756,-7.58756581812893));
#26389=CARTESIAN_POINT('Ctrl Pts',(18.6449442894794,11.8029800287248,-6.63418753286814));
#26390=CARTESIAN_POINT('Ctrl Pts',(18.5629765911754,10.3871150892957,-5.49535855640502));
#26391=CARTESIAN_POINT('Ctrl Pts',(17.8149199099546,12.9468769497926,-6.87670445596825));
#26392=CARTESIAN_POINT('Ctrl Pts',(18.560668214052,12.0098985669597,-6.07499002549749));
#26393=CARTESIAN_POINT('Ctrl Pts',(18.5465133552458,10.9156464454547,-5.13727390704943));
#26394=CARTESIAN_POINT('Ctrl Pts',(17.9429780453325,12.9716383743554,-6.50658870845175));
#26395=CARTESIAN_POINT('Ctrl Pts',(18.5345994117103,12.1317581217343,-5.78687279633148));
#26396=CARTESIAN_POINT('Ctrl Pts',(18.5459893337037,11.1880221188647,-4.96035691287977));
#26397=CARTESIAN_POINT('Ctrl Pts',(18.3026196043319,13.0467768755492,-5.37119067352287));
#26398=CARTESIAN_POINT('Ctrl Pts',(18.5087745838942,12.5265039443181,-4.92934391693923));
#26399=CARTESIAN_POINT('Ctrl Pts',(18.5655503358942,12.0145456291332,-4.43903273074705));
#26400=CARTESIAN_POINT('Ctrl Pts',(18.5104888199441,13.0982771986907,-4.57641845002038));
#26401=CARTESIAN_POINT('Ctrl Pts',(18.5584472440761,12.8398642052624,-4.33877715016644));
#26402=CARTESIAN_POINT('Ctrl Pts',(18.6062713681263,12.5811750651764,-4.10180132768386));
#26403=CARTESIAN_POINT('Ctrl Pts',(18.6735332660427,13.15,-3.76850837361349));
#26404=CARTESIAN_POINT('Ctrl Pts',(18.6735332660427,13.15,-3.76850837361349));
#26405=CARTESIAN_POINT('Ctrl Pts',(18.6735332660427,13.15,-3.76850837361349));
#26406=CARTESIAN_POINT('Ctrl Pts',(-2.59826221543221,7.75488674445212,-20.8996778314848));
#26407=CARTESIAN_POINT('Ctrl Pts',(-2.18962966210527,12.2921100651332,-21.6074501754737));
#26408=CARTESIAN_POINT('Ctrl Pts',(1.82293408768471,12.6595351585866,-19.3672161093864));
#26409=CARTESIAN_POINT('Ctrl Pts',(-2.71151859288215,7.82781362133594,-20.7035120314603));
#26410=CARTESIAN_POINT('Ctrl Pts',(-2.15923311032346,12.1550958708992,-21.6024826099445));
#26411=CARTESIAN_POINT('Ctrl Pts',(1.6433377752248,12.6661532847417,-19.3505719365413));
#26412=CARTESIAN_POINT('Ctrl Pts',(-2.83631932057571,7.93905335192905,-20.5122897107496));
#26413=CARTESIAN_POINT('Ctrl Pts',(-2.14758977172822,12.0132242375897,-21.5382097423197));
#26414=CARTESIAN_POINT('Ctrl Pts',(1.43050996215087,12.6762775771012,-19.3353172528801));
#26415=CARTESIAN_POINT('Ctrl Pts',(-3.09542191664885,8.21703647488254,-20.1567883096311));
#26416=CARTESIAN_POINT('Ctrl Pts',(-2.19372722643324,11.7807433434263,-21.3161401924937));
#26417=CARTESIAN_POINT('Ctrl Pts',(0.957692517741071,12.7015487707907,-19.3041728222174));
#26418=CARTESIAN_POINT('Ctrl Pts',(-3.22938372453809,8.38258529097424,-19.9922277562922));
#26419=CARTESIAN_POINT('Ctrl Pts',(-2.24796197710858,11.6893488147428,-21.1648941602397));
#26420=CARTESIAN_POINT('Ctrl Pts',(0.698469651424131,12.7165986624447,-19.2882015806242));
#26421=CARTESIAN_POINT('Ctrl Pts',(-3.50504758868887,8.75509815651651,-19.6844217444045));
#26422=CARTESIAN_POINT('Ctrl Pts',(-2.4224500983523,11.5743897252589,-20.8193710973479));
#26423=CARTESIAN_POINT('Ctrl Pts',(0.136230369374985,12.7504634691454,-19.2493934193698));
#26424=CARTESIAN_POINT('Ctrl Pts',(-3.64702760625654,8.96258837046762,-19.5409680384734));
#26425=CARTESIAN_POINT('Ctrl Pts',(-2.54036678451312,11.548164861387,-20.626405138958));
#26426=CARTESIAN_POINT('Ctrl Pts',(-0.167426378826852,12.7693262151714,
-19.2265008823239));
#26427=CARTESIAN_POINT('Ctrl Pts',(-3.93711590576484,9.4097722276261,-19.2733814592121));
#26428=CARTESIAN_POINT('Ctrl Pts',(-2.8313443108564,11.5609929861842,-20.231002285367));
#26429=CARTESIAN_POINT('Ctrl Pts',(-0.813546547001557,12.8099792937463,
-19.1677164203027));
#26430=CARTESIAN_POINT('Ctrl Pts',(-4.08311993398416,9.64614677008682,-19.151111740647));
#26431=CARTESIAN_POINT('Ctrl Pts',(-3.00067975712713,11.5974627760305,-20.0312189608217));
#26432=CARTESIAN_POINT('Ctrl Pts',(-1.15122301518874,12.8314678879227,-19.132229841979));
#26433=CARTESIAN_POINT('Ctrl Pts',(-4.52470127695561,10.3837101835134,-18.8120550761505));
#26434=CARTESIAN_POINT('Ctrl Pts',(-3.55592923968279,11.7789057456676,-19.4620646336976));
#26435=CARTESIAN_POINT('Ctrl Pts',(-2.20078434896851,12.8985191081262,-19.0002424448541));
#26436=CARTESIAN_POINT('Ctrl Pts',(-4.82372987872531,10.9130303131124,-18.6226026951196));
#26437=CARTESIAN_POINT('Ctrl Pts',(-4.00562246697594,11.9964940699711,-19.0995737130823));
#26438=CARTESIAN_POINT('Ctrl Pts',(-2.94963680022586,12.9466391191654,-18.8775777835082));
#26439=CARTESIAN_POINT('Ctrl Pts',(-5.43715525037156,12.0122001031275,-18.2984083796858));
#26440=CARTESIAN_POINT('Ctrl Pts',(-4.98336945256202,12.525352930137,-18.4949411801501));
#26441=CARTESIAN_POINT('Ctrl Pts',(-4.49642737856456,13.0465636459473,-18.5369007865598));
#26442=CARTESIAN_POINT('Ctrl Pts',(-5.75173970056742,12.5827074287695,-18.1641123299857));
#26443=CARTESIAN_POINT('Ctrl Pts',(-5.52318791400461,12.8406828545358,-18.2409857769472));
#26444=CARTESIAN_POINT('Ctrl Pts',(-5.29401344660782,13.098413834845,-18.318068662753));
#26445=CARTESIAN_POINT('Ctrl Pts',(-6.07314264709754,13.15,-18.0560083736136));
#26446=CARTESIAN_POINT('Ctrl Pts',(-6.07314264709754,13.15,-18.0560083736136));
#26447=CARTESIAN_POINT('Ctrl Pts',(-6.07314264709754,13.15,-18.0560083736136));
#26448=CARTESIAN_POINT('Origin',(1.73186480348997,7.75488674445212,-18.3996778314848));
#26449=CARTESIAN_POINT('Ctrl Pts',(-2.01363949025797,7.65,-21.9122740947459));
#26450=CARTESIAN_POINT('Ctrl Pts',(-2.01363949025797,12.65,-21.9122740947459));
#26451=CARTESIAN_POINT('Ctrl Pts',(2.31648752866421,12.65,-19.4122740947459));
#26452=CARTESIAN_POINT('Ctrl Pts',(-2.21006130259559,7.65000000135137,-21.5720615360624));
#26453=CARTESIAN_POINT('Ctrl Pts',(-2.05862391632681,12.5223340542645,-21.8343587832484));
#26454=CARTESIAN_POINT('Ctrl Pts',(2.15894594111395,12.65,-19.3980111200692));
#26455=CARTESIAN_POINT('Ctrl Pts',(-2.40496369270797,7.68525114336172,-21.2344806938712));
#26456=CARTESIAN_POINT('Ctrl Pts',(-2.11744970702864,12.4006679911003,-21.7324695249547));
#26457=CARTESIAN_POINT('Ctrl Pts',(1.99474242287307,12.6532040193815,-19.3831385282814));
#26458=CARTESIAN_POINT('Ctrl Pts',(-2.5982622154322,7.75488674445212,-20.8996778314848));
#26459=CARTESIAN_POINT('Ctrl Pts',(-2.18962966210525,12.2921100651332,-21.6074501754737));
#26460=CARTESIAN_POINT('Ctrl Pts',(1.82293408768472,12.6595351585866,-19.3672161093864));
#26461=CARTESIAN_POINT('Origin',(2.31648752866421,7.65,-19.4122740947459));
#26462=CARTESIAN_POINT('Origin',(17.33160439086,7.65,-45.419219381653));
#26463=CARTESIAN_POINT('Ctrl Pts',(6.05397759465306,7.65,-35.8857967818224));
#26464=CARTESIAN_POINT('Ctrl Pts',(6.06352325746355,7.75665550347739,-35.9023303548021));
#26465=CARTESIAN_POINT('Ctrl Pts',(6.07620607043637,7.86490613592037,-35.9173823925603));
#26466=CARTESIAN_POINT('Ctrl Pts',(6.09220990698139,7.97437516838736,-35.930768869142));
#26467=CARTESIAN_POINT('Ctrl Pts',(6.10830824806606,8.08449062838374,-35.9442343944446));
#26468=CARTESIAN_POINT('Ctrl Pts',(6.12776706996586,8.19583869503638,-35.9560145143081));
#26469=CARTESIAN_POINT('Ctrl Pts',(6.15073683959036,8.30800050757065,-35.9659357817465));
#26470=CARTESIAN_POINT('Ctrl Pts',(6.17401344605895,8.4216606101247,-35.9759895803526));
#26471=CARTESIAN_POINT('Ctrl Pts',(6.20089557012674,8.53615607897855,-35.9841343953433));
#26472=CARTESIAN_POINT('Ctrl Pts',(6.23150016777579,8.65101843498515,-35.99020587159));
#26473=CARTESIAN_POINT('Ctrl Pts',(6.2623698206027,8.76687557166323,-35.9963299306622));
#26474=CARTESIAN_POINT('Ctrl Pts',(6.29702678978594,8.88310560424299,-36.0003444559528));
#26475=CARTESIAN_POINT('Ctrl Pts',(6.33554935823233,8.99919970639809,-36.002099080833));
#26476=CARTESIAN_POINT('Ctrl Pts',(6.37461073779734,9.11691760456602,-36.003878247467));
#26477=CARTESIAN_POINT('Ctrl Pts',(6.4176467041125,9.2344952982669,-36.0033337063284));
#26478=CARTESIAN_POINT('Ctrl Pts',(6.46469470269531,9.35137976204325,-36.0003295326902));
#26479=CARTESIAN_POINT('Ctrl Pts',(6.49326431830472,9.42235715324775,-35.9985052662251));
#26480=CARTESIAN_POINT('Ctrl Pts',(6.5233124876975,9.49307850835805,-35.9957744359036));
#26481=CARTESIAN_POINT('Ctrl Pts',(6.55483963837352,9.56341716182477,-35.9921106142424));
#26482=CARTESIAN_POINT('Ctrl Pts',(6.60548566774611,9.67641099200345,-35.9862249564685));
#26483=CARTESIAN_POINT('Ctrl Pts',(6.65994309733461,9.78839632357693,-35.9779303378726));
#26484=CARTESIAN_POINT('Ctrl Pts',(6.71807963141314,9.8988893637445,-35.9672031436682));
#26485=CARTESIAN_POINT('Ctrl Pts',(6.77958949265622,10.0157936766134,-35.9558535123649));
#26486=CARTESIAN_POINT('Ctrl Pts',(6.84521800543985,10.1310268984947,-35.9417805765281));
#26487=CARTESIAN_POINT('Ctrl Pts',(6.91475494575457,10.2440187011879,-35.924987827173));
#26488=CARTESIAN_POINT('Ctrl Pts',(6.98227077550315,10.3537263656191,-35.9086831637618));
#26489=CARTESIAN_POINT('Ctrl Pts',(7.05347059423811,10.4613204844058,-35.8898146968345));
#26490=CARTESIAN_POINT('Ctrl Pts',(7.12811667144977,10.5662898659827,-35.868414021319));
#26491=CARTESIAN_POINT('Ctrl Pts',(7.20611458428136,10.675972691659,-35.8460523904638));
#26492=CARTESIAN_POINT('Ctrl Pts',(7.28787514481669,10.782788948211,-35.8209258990637));
#26493=CARTESIAN_POINT('Ctrl Pts',(7.37308073487587,10.8861779564399,-35.7931020365515));
#26494=CARTESIAN_POINT('Ctrl Pts',(7.45828632493505,10.9895669646689,-35.7652781740394));
#26495=CARTESIAN_POINT('Ctrl Pts',(7.54693650290271,11.089528019321,-35.7347570496121));
#26496=CARTESIAN_POINT('Ctrl Pts',(7.63867256219547,11.1855339059315,-35.7016367919725));
#26497=CARTESIAN_POINT('Ctrl Pts',(7.72657542381271,11.2775281798324,-35.6699004666227));
#26498=CARTESIAN_POINT('Ctrl Pts',(7.81729722444394,11.36587628634,-35.6357829950195));
#26499=CARTESIAN_POINT('Ctrl Pts',(7.91040854597715,11.4502607243425,-35.59946667711));
#26500=CARTESIAN_POINT('Ctrl Pts',(8.00553850608124,11.5364746034756,-35.5623630272319));
#26501=CARTESIAN_POINT('Ctrl Pts',(8.10316223285138,11.6185505432383,-35.5229643244569));
#26502=CARTESIAN_POINT('Ctrl Pts',(8.20279923200259,11.6961959778101,-35.481487511482));
#26503=CARTESIAN_POINT('Ctrl Pts',(8.29945318522683,11.7715167749547,-35.4412524785593));
#26504=CARTESIAN_POINT('Ctrl Pts',(8.39800107480301,11.8426682994014,-35.3990622286071));
#26505=CARTESIAN_POINT('Ctrl Pts',(8.49799155856711,11.9094303708404,-35.3551318347922));
#26506=CARTESIAN_POINT('Ctrl Pts',(8.59704122042354,11.9755642703069,-35.3116147870814));
#26507=CARTESIAN_POINT('Ctrl Pts',(8.6975059751535,12.0373907339791,-35.2663904256432));
#26508=CARTESIAN_POINT('Ctrl Pts',(8.79894221884899,12.094744772372,-35.219680763423));
#26509=CARTESIAN_POINT('Ctrl Pts',(8.89886011845857,12.1512403092884,-35.173670272789));
#26510=CARTESIAN_POINT('Ctrl Pts',(8.99972021909567,12.2033962128042,-35.1262188376971));
#26511=CARTESIAN_POINT('Ctrl Pts',(9.10110045647905,12.2511046771425,-35.0775478545584));
#26512=CARTESIAN_POINT('Ctrl Pts',(9.11421610266949,12.2572767611176,-35.0712512487201));
#26513=CARTESIAN_POINT('Ctrl Pts',(9.12734046197172,12.2633744796128,-35.0649342416672));
#26514=CARTESIAN_POINT('Ctrl Pts',(9.14047262843647,12.269397662556,-35.0585973212973));
#26515=CARTESIAN_POINT('Ctrl Pts',(9.24363829396122,12.3167154968663,-35.0088147809147));
#26516=CARTESIAN_POINT('Ctrl Pts',(9.34726516304563,12.3594653682624,-34.9578218063693));
#26517=CARTESIAN_POINT('Ctrl Pts',(9.45089273271786,12.3976812193462,-34.9058912848161));
#26518=CARTESIAN_POINT('Ctrl Pts',(9.55303426965624,12.4353490501894,-34.8547054536494));
#26519=CARTESIAN_POINT('Ctrl Pts',(9.65517611959362,12.4686120581676,-34.8026090032369));
#26520=CARTESIAN_POINT('Ctrl Pts',(9.75689503342851,12.4975498540545,-34.7498627514153));
#26521=CARTESIAN_POINT('Ctrl Pts',(9.83095240164393,12.5186182760868,-34.7114603693422));
#26522=CARTESIAN_POINT('Ctrl Pts',(9.9047859351615,12.5373950091745,-34.67271354614));
#26523=CARTESIAN_POINT('Ctrl Pts',(9.97823993362958,12.5539264020161,-34.6337217553209));
#26524=CARTESIAN_POINT('Ctrl Pts',(10.0799380486854,12.576814352656,-34.5797370613403));
#26525=CARTESIAN_POINT('Ctrl Pts',(10.180905038132,12.595396582188,-34.5252845278614));
#26526=CARTESIAN_POINT('Ctrl Pts',(10.2807483971159,12.6098896651044,-34.4706355317292));
#26527=CARTESIAN_POINT('Ctrl Pts',(10.3796426825862,12.6242449822119,-34.4165060084523));
#26528=CARTESIAN_POINT('Ctrl Pts',(10.4774343677972,12.6345887162111,-34.3621839124303));
#26529=CARTESIAN_POINT('Ctrl Pts',(10.5737742299967,12.641169267053,-34.3079222096205));
#26530=CARTESIAN_POINT('Ctrl Pts',(10.6609849886114,12.6471262491154,-34.2588023109854));
#26531=CARTESIAN_POINT('Ctrl Pts',(10.7470063181385,12.65,-34.209731852514));
#26532=CARTESIAN_POINT('Ctrl Pts',(10.83160439086,12.65,-34.1608891324553));
#26533=CARTESIAN_POINT('Ctrl Pts',(6.05397759465306,7.65,-35.8857967818224));
#26534=CARTESIAN_POINT('Ctrl Pts',(6.05397759465306,7.65,-35.8857967818224));
#26535=CARTESIAN_POINT('Ctrl Pts',(6.05397759465306,7.65,-35.8857967818224));
#26536=CARTESIAN_POINT('Ctrl Pts',(6.11256573845244,8.30461645762939,-35.9872744236041));
#26537=CARTESIAN_POINT('Ctrl Pts',(6.18568737744441,8.23864736688774,-36.1139248174709));
#26538=CARTESIAN_POINT('Ctrl Pts',(6.25900485142217,8.17355351675001,-36.240914407483));
#26539=CARTESIAN_POINT('Ctrl Pts',(6.2838113402416,8.9587394433133,-36.0236072553336));
#26540=CARTESIAN_POINT('Ctrl Pts',(6.4083797352317,8.83304537535228,-36.2924955578147));
#26541=CARTESIAN_POINT('Ctrl Pts',(6.57657917544434,8.69671236121524,-36.5306960207266));
#26542=CARTESIAN_POINT('Ctrl Pts',(6.82586793650413,10.1680948803376,-35.9606139731479));
#26543=CARTESIAN_POINT('Ctrl Pts',(7.02469852379275,9.96758997398064,-36.522914965901));
#26544=CARTESIAN_POINT('Ctrl Pts',(7.38917119042457,9.6639387189906,-36.9362838290071));
#26545=CARTESIAN_POINT('Ctrl Pts',(7.19645515023948,10.7227336174027,-35.8612943435307));
#26546=CARTESIAN_POINT('Ctrl Pts',(7.42549815621051,10.5146815062461,-36.5742108314027));
#26547=CARTESIAN_POINT('Ctrl Pts',(7.88383228548133,10.1075313875409,-37.0518664657295));
#26548=CARTESIAN_POINT('Ctrl Pts',(8.08088997414811,11.6483341944628,-35.5419792404035));
#26549=CARTESIAN_POINT('Ctrl Pts',(8.39184058382502,11.4817645043902,-36.5160118602147));
#26550=CARTESIAN_POINT('Ctrl Pts',(8.97532595413734,10.8478143907806,-37.0911878018637));
#26551=CARTESIAN_POINT('Ctrl Pts',(8.59438969571741,12.0189319519102,-35.3221093677828));
#26552=CARTESIAN_POINT('Ctrl Pts',(8.96249719550974,11.89838707943,-36.4018237591869));
#26553=CARTESIAN_POINT('Ctrl Pts',(9.57172919308274,11.1442135371052,-37.0149110334635));
#26554=CARTESIAN_POINT('Ctrl Pts',(9.41351409479233,12.3946305178796,-34.926841298045));
#26555=CARTESIAN_POINT('Ctrl Pts',(9.88970755753321,12.3384327759138,-36.0938826425933));
#26556=CARTESIAN_POINT('Ctrl Pts',(10.4748981713972,11.444692242091,-36.7652124450691));
#26557=CARTESIAN_POINT('Ctrl Pts',(9.69456540456372,12.4900832460695,-34.7843054965499));
#26558=CARTESIAN_POINT('Ctrl Pts',(10.2112056628904,12.4537748504033,-35.96786613135));
#26559=CARTESIAN_POINT('Ctrl Pts',(10.7773024622675,11.5210340617089,-36.6596610917303));
#26560=CARTESIAN_POINT('Ctrl Pts',(10.2619144626914,12.6177695579628,-34.4831380140834));
#26561=CARTESIAN_POINT('Ctrl Pts',(10.8598325063373,12.6099538847863,-35.6740833652685));
#26562=CARTESIAN_POINT('Ctrl Pts',(11.3732152236663,11.6231558718973,-36.4079673945819));
#26563=CARTESIAN_POINT('Ctrl Pts',(10.5481950339283,12.65,-34.3245156009683));
#26564=CARTESIAN_POINT('Ctrl Pts',(11.1853523980411,12.6499999999596,-35.5068373265266));
#26565=CARTESIAN_POINT('Ctrl Pts',(11.6667058142795,11.6489333498051,-36.2618331013498));
#26566=CARTESIAN_POINT('Ctrl Pts',(10.83160439086,12.65,-34.1608891324553));
#26567=CARTESIAN_POINT('Ctrl Pts',(11.5028540567871,12.65,-35.3235276584047));
#26568=CARTESIAN_POINT('Ctrl Pts',(11.9501151712097,11.6489333498058,-36.0982066328345));
#26569=CARTESIAN_POINT('Origin',(17.33160439086,-7.90000000000001,-45.419219381653));
#26570=CARTESIAN_POINT('Origin',(17.3316043908594,-7.90000000000001,45.4192193816532));
#26571=CARTESIAN_POINT('Ctrl Pts',(6.05397759465256,7.65,35.8857967818225));
#26572=CARTESIAN_POINT('Ctrl Pts',(6.05397759465256,7.65,35.8857967818225));
#26573=CARTESIAN_POINT('Ctrl Pts',(6.05397759465256,7.65,35.8857967818225));
#26574=CARTESIAN_POINT('Ctrl Pts',(6.25900485142175,8.17355351675083,36.2409144074832));
#26575=CARTESIAN_POINT('Ctrl Pts',(6.18568737744254,8.23864736688944,36.1139248174686));
#26576=CARTESIAN_POINT('Ctrl Pts',(6.11256573845197,8.30461645762935,35.9872744236042));
#26577=CARTESIAN_POINT('Ctrl Pts',(6.57657917544341,8.69671236121402,36.5306960207267));
#26578=CARTESIAN_POINT('Ctrl Pts',(6.40837973523168,8.83304537535155,36.2924955578148));
#26579=CARTESIAN_POINT('Ctrl Pts',(6.28381134024114,8.95873944331333,36.0236072553337));
#26580=CARTESIAN_POINT('Ctrl Pts',(7.38917119042446,9.66393871899181,36.9362838290071));
#26581=CARTESIAN_POINT('Ctrl Pts',(7.02469852379175,9.96758997398138,36.5229149659011));
#26582=CARTESIAN_POINT('Ctrl Pts',(6.82586793650358,10.1680948803376,35.9606139731479));
#26583=CARTESIAN_POINT('Ctrl Pts',(7.88383228548062,10.10753138754,37.0518664657301));
#26584=CARTESIAN_POINT('Ctrl Pts',(7.42549815620927,10.5146815062463,36.5742108314018));
#26585=CARTESIAN_POINT('Ctrl Pts',(7.19645515023883,10.7227336174031,35.8612943435298));
#26586=CARTESIAN_POINT('Ctrl Pts',(8.97532595413702,10.8478143907815,37.0911878018634));
#26587=CARTESIAN_POINT('Ctrl Pts',(8.3918405838252,11.48176450439,36.5160118602157));
#26588=CARTESIAN_POINT('Ctrl Pts',(8.08088997414776,11.6483341944624,35.5419792404046));
#26589=CARTESIAN_POINT('Ctrl Pts',(9.571729193082,11.1442135371058,37.0149110334632));
#26590=CARTESIAN_POINT('Ctrl Pts',(8.96249719550926,11.89838707943,36.4018237591861));
#26591=CARTESIAN_POINT('Ctrl Pts',(8.59438969571705,12.0189319519102,35.3221093677829));
#26592=CARTESIAN_POINT('Ctrl Pts',(10.4748981713968,11.4446922420907,36.7652124450694));
#26593=CARTESIAN_POINT('Ctrl Pts',(9.88970755753271,12.3384327759138,36.0938826425938));
#26594=CARTESIAN_POINT('Ctrl Pts',(9.41351409479177,12.3946305178795,34.9268412980451));
#26595=CARTESIAN_POINT('Ctrl Pts',(10.7773024622668,11.5210340617088,36.6596610917307));
#26596=CARTESIAN_POINT('Ctrl Pts',(10.2112056628899,12.4537748504033,35.9678661313506));
#26597=CARTESIAN_POINT('Ctrl Pts',(9.69456540456328,12.4900832460695,34.78430549655));
#26598=CARTESIAN_POINT('Ctrl Pts',(11.373215223666,11.6231558718975,36.4079673945819));
#26599=CARTESIAN_POINT('Ctrl Pts',(10.8598325063368,12.6099538847863,35.6740833652681));
#26600=CARTESIAN_POINT('Ctrl Pts',(10.2619144626909,12.6177695579628,34.4831380140835));
#26601=CARTESIAN_POINT('Ctrl Pts',(11.6667058142791,11.6489333498044,36.2618331013506));
#26602=CARTESIAN_POINT('Ctrl Pts',(11.1853523980417,12.6499999999595,35.5068373265291));
#26603=CARTESIAN_POINT('Ctrl Pts',(10.5481950339276,12.65,34.3245156009679));
#26604=CARTESIAN_POINT('Ctrl Pts',(11.9501151712092,11.6489333498058,36.0982066328347));
#26605=CARTESIAN_POINT('Ctrl Pts',(11.5028540567866,12.65,35.3235276584049));
#26606=CARTESIAN_POINT('Ctrl Pts',(10.8316043908595,12.65,34.1608891324555));
#26607=CARTESIAN_POINT('Ctrl Pts',(6.05397759465256,7.65,35.8857967818225));
#26608=CARTESIAN_POINT('Ctrl Pts',(6.06352325746305,7.75665550347733,35.9023303548022));
#26609=CARTESIAN_POINT('Ctrl Pts',(6.07620607043586,7.86490613592026,35.9173823925604));
#26610=CARTESIAN_POINT('Ctrl Pts',(6.09220990698088,7.9743751683872,35.9307688691421));
#26611=CARTESIAN_POINT('Ctrl Pts',(6.10830824806559,8.08449062838383,35.9442343944447));
#26612=CARTESIAN_POINT('Ctrl Pts',(6.12776706996545,8.19583869503674,35.9560145143083));
#26613=CARTESIAN_POINT('Ctrl Pts',(6.15073683959002,8.30800050757127,35.9659357817467));
#26614=CARTESIAN_POINT('Ctrl Pts',(6.17401344605865,8.42166061012539,35.9759895803528));
#26615=CARTESIAN_POINT('Ctrl Pts',(6.20089557012648,8.53615607897931,35.9841343953435));
#26616=CARTESIAN_POINT('Ctrl Pts',(6.23150016777558,8.65101843498598,35.9902058715903));
#26617=CARTESIAN_POINT('Ctrl Pts',(6.26236982060258,8.7668755716643,35.9963299306624));
#26618=CARTESIAN_POINT('Ctrl Pts',(6.29702678978593,8.88310560424431,36.0003444559531));
#26619=CARTESIAN_POINT('Ctrl Pts',(6.33554935823244,8.99919970639965,36.0020990808332));
#26620=CARTESIAN_POINT('Ctrl Pts',(6.37461073779751,9.11691760456761,36.0038782474673));
#26621=CARTESIAN_POINT('Ctrl Pts',(6.41764670411273,9.23449529826853,36.0033337063286));
#26622=CARTESIAN_POINT('Ctrl Pts',(6.46469470269562,9.35137976204491,36.0003295326905));
#26623=CARTESIAN_POINT('Ctrl Pts',(6.49326431830481,9.42235715324882,35.9985052662254));
#26624=CARTESIAN_POINT('Ctrl Pts',(6.52331248769736,9.49307850835852,35.9957744359039));
#26625=CARTESIAN_POINT('Ctrl Pts',(6.55483963837312,9.56341716182466,35.9921106142428));
#26626=CARTESIAN_POINT('Ctrl Pts',(6.6054856677456,9.67641099200306,35.9862249564689));
#26627=CARTESIAN_POINT('Ctrl Pts',(6.65994309733397,9.78839632357628,35.9779303378731));
#26628=CARTESIAN_POINT('Ctrl Pts',(6.71807963141235,9.8988893637436,35.9672031436686));
#26629=CARTESIAN_POINT('Ctrl Pts',(6.77958949265545,10.0157936766126,35.9558535123653));
#26630=CARTESIAN_POINT('Ctrl Pts',(6.84521800543911,10.1310268984939,35.9417805765286));
#26631=CARTESIAN_POINT('Ctrl Pts',(6.91475494575386,10.2440187011872,35.9249878271734));
#26632=CARTESIAN_POINT('Ctrl Pts',(6.98227077550244,10.3537263656185,35.9086831637623));
#26633=CARTESIAN_POINT('Ctrl Pts',(7.0534705942374,10.4613204844052,35.889814696835));
#26634=CARTESIAN_POINT('Ctrl Pts',(7.12811667144906,10.5662898659821,35.8684140213195));
#26635=CARTESIAN_POINT('Ctrl Pts',(7.20611458428071,10.6759726916585,35.8460523904643));
#26636=CARTESIAN_POINT('Ctrl Pts',(7.28787514481612,10.7827889482106,35.8209258990643));
#26637=CARTESIAN_POINT('Ctrl Pts',(7.3730807348754,10.8861779564396,35.7931020365523));
#26638=CARTESIAN_POINT('Ctrl Pts',(7.45828632493467,10.9895669646686,35.7652781740402));
#26639=CARTESIAN_POINT('Ctrl Pts',(7.54693650290243,11.0895280193208,35.7347570496131));
#26640=CARTESIAN_POINT('Ctrl Pts',(7.63867256219533,11.1855339059313,35.7016367919737));
#26641=CARTESIAN_POINT('Ctrl Pts',(7.72657542381267,11.2775281798321,35.6699004666241));
#26642=CARTESIAN_POINT('Ctrl Pts',(7.817297224444,11.3658762863397,35.6357829950211));
#26643=CARTESIAN_POINT('Ctrl Pts',(7.91040854597731,11.4502607243423,35.5994666771117));
#26644=CARTESIAN_POINT('Ctrl Pts',(8.00553850608143,11.5364746034753,35.5623630272337));
#26645=CARTESIAN_POINT('Ctrl Pts',(8.10316223285158,11.6185505432381,35.5229643244588));
#26646=CARTESIAN_POINT('Ctrl Pts',(8.20279923200281,11.6961959778098,35.481487511484));
#26647=CARTESIAN_POINT('Ctrl Pts',(8.29945318522714,11.7715167749545,35.4412524785613));
#26648=CARTESIAN_POINT('Ctrl Pts',(8.39800107480342,11.8426682994013,35.399062228609));
#26649=CARTESIAN_POINT('Ctrl Pts',(8.49799155856761,11.9094303708404,35.355131834794));
#26650=CARTESIAN_POINT('Ctrl Pts',(8.59704122042377,11.9755642703067,35.3116147870833));
#26651=CARTESIAN_POINT('Ctrl Pts',(8.69750597515344,12.0373907339787,35.2663904256451));
#26652=CARTESIAN_POINT('Ctrl Pts',(8.79894221884864,12.0947447723716,35.2196807634251));
#26653=CARTESIAN_POINT('Ctrl Pts',(8.8988601184582,12.151240309288,35.173670272791));
#26654=CARTESIAN_POINT('Ctrl Pts',(8.99972021909529,12.2033962128038,35.1262188376991));
#26655=CARTESIAN_POINT('Ctrl Pts',(9.10110045647863,12.2511046771421,35.0775478545603));
#26656=CARTESIAN_POINT('Ctrl Pts',(9.11421610266926,12.2572767611173,35.071251248722));
#26657=CARTESIAN_POINT('Ctrl Pts',(9.12734046197164,12.2633744796126,35.064934241669));
#26658=CARTESIAN_POINT('Ctrl Pts',(9.14047262843657,12.2693976625559,35.0585973212989));
#26659=CARTESIAN_POINT('Ctrl Pts',(9.24363829396072,12.316715496866,35.0088147809166));
#26660=CARTESIAN_POINT('Ctrl Pts',(9.34726516304456,12.3594653682618,34.9578218063714));
#26661=CARTESIAN_POINT('Ctrl Pts',(9.45089273271621,12.3976812193455,34.9058912848185));
#26662=CARTESIAN_POINT('Ctrl Pts',(9.55303426965392,12.4353490501885,34.8547054536521));
#26663=CARTESIAN_POINT('Ctrl Pts',(9.65517611959064,12.4686120581666,34.80260900324));
#26664=CARTESIAN_POINT('Ctrl Pts',(9.75689503342485,12.4975498540534,34.7498627514186));
#26665=CARTESIAN_POINT('Ctrl Pts',(9.83095240164152,12.5186182760862,34.7114603693449));
#26666=CARTESIAN_POINT('Ctrl Pts',(9.90478593516031,12.5373950091742,34.6727135461419));
#26667=CARTESIAN_POINT('Ctrl Pts',(9.97823993362961,12.5539264020161,34.6337217553221));
#26668=CARTESIAN_POINT('Ctrl Pts',(10.0799380486856,12.576814352656,34.5797370613413));
#26669=CARTESIAN_POINT('Ctrl Pts',(10.1809050381322,12.595396582188,34.5252845278622));
#26670=CARTESIAN_POINT('Ctrl Pts',(10.2807483971162,12.6098896651045,34.4706355317297));
#26671=CARTESIAN_POINT('Ctrl Pts',(10.3796426825865,12.6242449822119,34.4165060084527));
#26672=CARTESIAN_POINT('Ctrl Pts',(10.4774343677974,12.6345887162112,34.3621839124305));
#26673=CARTESIAN_POINT('Ctrl Pts',(10.5737742299969,12.641169267053,34.3079222096205));
#26674=CARTESIAN_POINT('Ctrl Pts',(10.6609849886113,12.6471262491154,34.2588023109854));
#26675=CARTESIAN_POINT('Ctrl Pts',(10.7470063181382,12.65,34.209731852514));
#26676=CARTESIAN_POINT('Ctrl Pts',(10.8316043908595,12.65,34.1608891324555));
#26677=CARTESIAN_POINT('Origin',(10.8316043908595,7.65,34.1608891324555));
#26678=CARTESIAN_POINT('Origin',(2.31648752866394,7.65,19.4122740947459));
#26679=CARTESIAN_POINT('Ctrl Pts',(2.31648752866395,12.65,19.4122740947459));
#26680=CARTESIAN_POINT('Ctrl Pts',(-2.01363949025827,12.65,21.9122740947459));
#26681=CARTESIAN_POINT('Ctrl Pts',(-2.01363949025827,7.65,21.9122740947459));
#26682=CARTESIAN_POINT('Ctrl Pts',(2.158945941114,12.65,19.398011120066));
#26683=CARTESIAN_POINT('Ctrl Pts',(-2.05862391633069,12.5223340542653,21.8343587832445));
#26684=CARTESIAN_POINT('Ctrl Pts',(-2.21006130259589,7.65000000135137,21.5720615360624));
#26685=CARTESIAN_POINT('Ctrl Pts',(1.99474242287254,12.653204019381,19.3831385282839));
#26686=CARTESIAN_POINT('Ctrl Pts',(-2.1174497070286,12.4006679911032,21.732469524956));
#26687=CARTESIAN_POINT('Ctrl Pts',(-2.40496369270825,7.68525114336183,21.2344806938712));
#26688=CARTESIAN_POINT('Ctrl Pts',(1.82293408768446,12.6595351585866,19.3672161093864));
#26689=CARTESIAN_POINT('Ctrl Pts',(-2.18962966210555,12.2921100651332,21.6074501754736));
#26690=CARTESIAN_POINT('Ctrl Pts',(-2.59826221543248,7.75488674445211,20.8996778314848));
#26691=CARTESIAN_POINT('Origin',(1.73186480348973,7.75488674445211,18.3996778314848));
#26692=CARTESIAN_POINT('Ctrl Pts',(1.82293408768446,12.6595351585866,19.3672161093864));
#26693=CARTESIAN_POINT('Ctrl Pts',(-2.18962966210555,12.2921100651332,21.6074501754736));
#26694=CARTESIAN_POINT('Ctrl Pts',(-2.59826221543248,7.75488674445211,20.8996778314848));
#26695=CARTESIAN_POINT('Ctrl Pts',(1.63885776870729,12.666318372986,19.3501567500646));
#26696=CARTESIAN_POINT('Ctrl Pts',(-2.15856705477721,12.1520935820205,21.6023737557688));
#26697=CARTESIAN_POINT('Ctrl Pts',(-2.71413769515256,7.82950008896478,20.6989756132582));
#26698=CARTESIAN_POINT('Ctrl Pts',(1.43007155004091,12.6763099143986,19.3352963986434));
#26699=CARTESIAN_POINT('Ctrl Pts',(-2.14786497084269,12.0132183330853,21.5377143077062));
#26700=CARTESIAN_POINT('Ctrl Pts',(-2.83650075163869,7.93940906195218,20.5121824209172));
#26701=CARTESIAN_POINT('Ctrl Pts',(0.963339160700537,12.7012381622111,19.30453683087));
#26702=CARTESIAN_POINT('Ctrl Pts',(-2.19297758782216,11.7832074074835,21.3189597524121));
#26703=CARTESIAN_POINT('Ctrl Pts',(-3.09238573762713,8.21361978075487,20.1608140239618));
#26704=CARTESIAN_POINT('Ctrl Pts',(0.705363484677257,12.7161912440272,19.288651778162));
#26705=CARTESIAN_POINT('Ctrl Pts',(-2.24613629826497,11.6912659624442,21.1690685793912));
#26706=CARTESIAN_POINT('Ctrl Pts',(-3.22591261316364,8.37810368845214,19.9963051847538));
#26707=CARTESIAN_POINT('Ctrl Pts',(0.140400190055169,12.7502046526726,19.2497063845938));
#26708=CARTESIAN_POINT('Ctrl Pts',(-2.42082465748723,11.5747870675349,20.8220625359603));
#26709=CARTESIAN_POINT('Ctrl Pts',(-3.50309246541194,8.752251175245,19.6864071512402));
#26710=CARTESIAN_POINT('Ctrl Pts',(-0.165902550976841,12.7692327202596,
19.2265953913871));
#26711=CARTESIAN_POINT('Ctrl Pts',(-2.53989492939034,11.5484270002409,20.6273404315831));
#26712=CARTESIAN_POINT('Ctrl Pts',(-3.64629128691028,8.96155992656158,19.5417641964904));
#26713=CARTESIAN_POINT('Ctrl Pts',(-0.806001813909957,12.8095022395594,
19.1684463542416));
#26714=CARTESIAN_POINT('Ctrl Pts',(-2.82783067410163,11.5605687167961,20.2354968998797));
#26715=CARTESIAN_POINT('Ctrl Pts',(-3.93377998354566,9.40452463144772,19.2763433096647));
#26716=CARTESIAN_POINT('Ctrl Pts',(-1.14199205761375,12.8308799157878,19.1332633001334));
#26717=CARTESIAN_POINT('Ctrl Pts',(-2.99594386527674,11.5962530038109,20.0365408492835));
#26718=CARTESIAN_POINT('Ctrl Pts',(-4.07916420286535,9.63967907679387,19.154337615297));
#26719=CARTESIAN_POINT('Ctrl Pts',(-1.84114015329749,12.8755415399104,19.0455933955465));
#26720=CARTESIAN_POINT('Ctrl Pts',(-3.37066091328056,11.7180448914426,19.6515306856625));
#26721=CARTESIAN_POINT('Ctrl Pts',(-4.37345844384653,10.130956935887,18.9279994114957));
#26722=CARTESIAN_POINT('Ctrl Pts',(-2.20430287120771,12.8988286442761,18.9930962044593));
#26723=CARTESIAN_POINT('Ctrl Pts',(-3.57709720780661,11.8029800287245,19.4640891732687));
#26724=CARTESIAN_POINT('Ctrl Pts',(-4.52236818283683,10.3871150892957,18.8236885760162));
#26725=CARTESIAN_POINT('Ctrl Pts',(-2.95205920179125,12.9468769497921,18.8665254363902));
#26726=CARTESIAN_POINT('Ctrl Pts',(-4.01923841720749,12.0098985669601,19.1115051973322));
#26727=CARTESIAN_POINT('Ctrl Pts',(-4.82424696791924,10.9156464454547,18.630388670795));
#26728=CARTESIAN_POINT('Ctrl Pts',(-3.33661790917173,12.9716383743556,18.7923691610298));
#26729=CARTESIAN_POINT('Ctrl Pts',(-4.2557208557653,12.1317581217325,18.9448703376736));
#26730=CARTESIAN_POINT('Ctrl Pts',(-4.97719956846094,11.1880221188625,18.5414763577422));
#26731=CARTESIAN_POINT('Ctrl Pts',(-4.49972223032189,13.0467768755487,18.5361288699168));
#26732=CARTESIAN_POINT('Ctrl Pts',(-4.98545023588316,12.5265039443217,18.4937409410444));
#26733=CARTESIAN_POINT('Ctrl Pts',(-5.43846005488829,12.0145456291375,18.2977545914973));
#26734=CARTESIAN_POINT('Ctrl Pts',(-5.29194977390885,13.0982771986938,18.3187627795489));
#26735=CARTESIAN_POINT('Ctrl Pts',(-5.52173238862912,12.8398642052775,18.2414753432483));
#26736=CARTESIAN_POINT('Ctrl Pts',(-5.75087153299792,12.5811750651829,18.1644043383511));
#26737=CARTESIAN_POINT('Ctrl Pts',(-6.07314264709777,13.15,18.0560083736135));
#26738=CARTESIAN_POINT('Ctrl Pts',(-6.07314264709777,13.15,18.0560083736135));
#26739=CARTESIAN_POINT('Ctrl Pts',(-6.07314264709777,13.15,18.0560083736135));
#26740=CARTESIAN_POINT('Ctrl Pts',(19.3987830406924,7.75488674445212,8.19967783148497));
#26741=CARTESIAN_POINT('Ctrl Pts',(19.8074155940193,12.2921100651332,8.90745017547383));
#26742=CARTESIAN_POINT('Ctrl Pts',(15.8610341074694,12.6595351585866,11.2623152840528));
#26743=CARTESIAN_POINT('Ctrl Pts',(19.2855266632425,7.82781362133611,8.00351203146055));
#26744=CARTESIAN_POINT('Ctrl Pts',(19.7879152801881,12.1550958708994,8.93129057874443));
#26745=CARTESIAN_POINT('Ctrl Pts',(15.9364179871942,12.6661532847409,11.0984582286157));
#26746=CARTESIAN_POINT('Ctrl Pts',(19.1823236395831,7.93905335192905,7.79982027051171));
#26747=CARTESIAN_POINT('Ctrl Pts',(19.7264316747511,12.0132242375897,8.90923757193522));
#26748=CARTESIAN_POINT('Ctrl Pts',(16.0296209501497,12.6762775771014,10.9065165940293));
#26749=CARTESIAN_POINT('Ctrl Pts',(19.0040016931701,8.21703647488254,7.39768013956664));
#26750=CARTESIAN_POINT('Ctrl Pts',(19.557182530546,11.7807433434263,8.75824658918266));
#26751=CARTESIAN_POINT('Ctrl Pts',(16.2390578042154,12.7015487707905,10.4814724604871));
#26752=CARTESIAN_POINT('Ctrl Pts',(18.9284689774622,8.3825852909746,7.19938553412737));
#26753=CARTESIAN_POINT('Ctrl Pts',(19.4533169997301,11.6893488147424,8.6356549012008));
#26754=CARTESIAN_POINT('Ctrl Pts',(16.3548377364231,12.7165986624452,10.2489932522172));
#26755=CARTESIAN_POINT('Ctrl Pts',(18.7997330838058,8.75509815651615,6.80675061892527));
#26756=CARTESIAN_POINT('Ctrl Pts',(19.2413293102956,11.5743897252593,8.31178222410246));
#26757=CARTESIAN_POINT('Ctrl Pts',(16.6023485239282,12.7504634691448,9.74267567033139));
#26758=CARTESIAN_POINT('Ctrl Pts',(18.746488538986,8.96258837046799,6.61206546391529));
#26759=CARTESIAN_POINT('Ctrl Pts',(19.1331742313435,11.5481648613881,8.11318039916058));
#26760=CARTESIAN_POINT('Ctrl Pts',(16.7343513793893,12.7693262151716,9.46825494383473));
#26761=CARTESIAN_POINT('Ctrl Pts',(18.6597959133881,9.40977222762574,6.22704833757024));
#26762=CARTESIAN_POINT('Ctrl Pts',(18.9362340785775,11.5609929861831,7.6634850426214));
#26763=CARTESIAN_POINT('Ctrl Pts',(17.0065026260195,12.809979293746,8.87930623328658));
#26764=CARTESIAN_POINT('Ctrl Pts',(18.6269092451068,9.6461467700861,6.03947028079449));
#26765=CARTESIAN_POINT('Ctrl Pts',(18.8478843674036,11.5974627760309,7.41694458211731));
#26766=CARTESIAN_POINT('Ctrl Pts',(17.1446085817907,12.831467887923,8.56912654441456));
#26767=CARTESIAN_POINT('Ctrl Pts',(18.5540682318161,10.3837101835148,5.48752128769627));
#26768=CARTESIAN_POINT('Ctrl Pts',(18.6326070027182,11.7789057456669,6.6515072612234));
#26769=CARTESIAN_POINT('Ctrl Pts',(17.5550848097915,12.8985191081256,7.59418606796978));
#26770=CARTESIAN_POINT('Ctrl Pts',(18.5395119579207,10.9130303131145,5.13382873159073));
#26771=CARTESIAN_POINT('Ctrl Pts',(18.5435272704706,11.9964940699733,6.08081604217292));
#26772=CARTESIAN_POINT('Ctrl Pts',(17.8232803225471,12.9466391191647,6.8843284908237));
#26773=CARTESIAN_POINT('Ctrl Pts',(18.5654641308157,12.0122001031253,4.4404896187003));
#26774=CARTESIAN_POINT('Ctrl Pts',(18.50877362979,12.5253529301349,4.9317460477106));
#26775=CARTESIAN_POINT('Ctrl Pts',(18.3016406778754,13.046563645948,5.37443005716869));
#26776=CARTESIAN_POINT('Ctrl Pts',(18.6064525652392,12.5827074287898,4.10090346837722));
#26777=CARTESIAN_POINT('Ctrl Pts',(18.5587510299058,12.8406828545658,4.33727184508721));
#26778=CARTESIAN_POINT('Ctrl Pts',(18.5109195335152,13.0984138348512,4.57428419864026));
#26779=CARTESIAN_POINT('Ctrl Pts',(18.6735332660427,13.15,3.76850837361377));
#26780=CARTESIAN_POINT('Ctrl Pts',(18.6735332660427,13.15,3.76850837361377));
#26781=CARTESIAN_POINT('Ctrl Pts',(18.6735332660427,13.15,3.76850837361377));
#26782=CARTESIAN_POINT('Origin',(15.0686560217701,7.75488674445212,10.6996778314849));
#26783=CARTESIAN_POINT('Ctrl Pts',(19.9834057658666,7.65,9.21227409474614));
#26784=CARTESIAN_POINT('Ctrl Pts',(19.9834057658666,12.65,9.21227409474612));
#26785=CARTESIAN_POINT('Ctrl Pts',(15.6532787469444,12.65,11.7122740947461));
#26786=CARTESIAN_POINT('Ctrl Pts',(19.786983953529,7.65000000135137,8.87206153606267));
#26787=CARTESIAN_POINT('Ctrl Pts',(19.9384213397991,12.5223340542634,9.13435878324342));
#26788=CARTESIAN_POINT('Ctrl Pts',(15.7196974423163,12.65,11.5687075904368));
#26789=CARTESIAN_POINT('Ctrl Pts',(19.5920815634165,7.68525114336148,8.53448069387126));
#26790=CARTESIAN_POINT('Ctrl Pts',(19.879595549097,12.4006679911059,9.03246952495355));
#26791=CARTESIAN_POINT('Ctrl Pts',(15.788919159126,12.6532040193819,11.4190668763545));
#26792=CARTESIAN_POINT('Ctrl Pts',(19.3987830406924,7.75488674445212,8.19967783148497));
#26793=CARTESIAN_POINT('Ctrl Pts',(19.8074155940193,12.2921100651331,8.90745017547383));
#26794=CARTESIAN_POINT('Ctrl Pts',(15.8610341074694,12.6595351585866,11.2623152840528));
#26795=CARTESIAN_POINT('Origin',(15.6532787469444,7.65,11.7122740947461));
#26796=CARTESIAN_POINT('Origin',(30.6683956091398,7.65,37.7192193816533));
#26797=CARTESIAN_POINT('Ctrl Pts',(28.0510228507774,7.65,23.1857967818227));
#26798=CARTESIAN_POINT('Ctrl Pts',(28.060568513588,7.7566555034772,23.2023303548025));
#26799=CARTESIAN_POINT('Ctrl Pts',(28.067262554179,7.86490613592002,23.2208400119076));
#26800=CARTESIAN_POINT('Ctrl Pts',(28.0708536646935,7.97437516838686,23.2413929792046));
#26801=CARTESIAN_POINT('Ctrl Pts',(28.0744659811386,8.08449062838318,23.2620673141941));
#26802=CARTESIAN_POINT('Ctrl Pts',(28.0749384532501,8.19583869503577,23.2848092082189));
#26803=CARTESIAN_POINT('Ctrl Pts',(28.0720456380773,8.30800050757001,23.3096622459521));
#26804=CARTESIAN_POINT('Ctrl Pts',(28.0691141798405,8.42166061012386,23.3348472777708));
#26805=CARTESIAN_POINT('Ctrl Pts',(28.0627267344978,8.53615607897753,23.3622002876166));
#26806=CARTESIAN_POINT('Ctrl Pts',(28.0526824883414,8.65101843498394,23.3917403847766));
#26807=CARTESIAN_POINT('Ctrl Pts',(28.0425512526588,8.76687557166174,23.4215363178668));
#26808=CARTESIAN_POINT('Ctrl Pts',(28.0286994489531,8.88310560424122,23.4535573962429));
#26809=CARTESIAN_POINT('Ctrl Pts',(28.0109577144504,8.99919970639603,23.4877962315765));
#26810=CARTESIAN_POINT('Ctrl Pts',(27.9929678281707,9.11691760456367,23.5225139619036));
#26811=CARTESIAN_POINT('Ctrl Pts',(27.9709782585537,9.23449529826427,23.5595119314396));
#26812=CARTESIAN_POINT('Ctrl Pts',(27.9448525685745,9.35137976204033,23.5987546065903));
#26813=CARTESIAN_POINT('Ctrl Pts',(27.9289878996676,9.42235715324562,23.6225844862522));
#26814=CARTESIAN_POINT('Ctrl Pts',(27.9115988465393,9.49307850835669,23.6472415491231));
#26815=CARTESIAN_POINT('Ctrl Pts',(27.8926623085676,9.56341716182418,23.6727129516872));
#26816=CARTESIAN_POINT('Ctrl Pts',(27.8622421647312,9.67641099200259,23.7136308708377));
#26817=CARTESIAN_POINT('Ctrl Pts',(27.8278300995184,9.78839632357584,23.7566450789882));
#26818=CARTESIAN_POINT('Ctrl Pts',(27.7894718097869,9.89888936374319,23.801629197286));
#26819=CARTESIAN_POINT('Ctrl Pts',(27.7488878101332,10.0157936766121,23.8492234840541));
#26820=CARTESIAN_POINT('Ctrl Pts',(27.703886033801,10.1310268984934,23.899022975419));
#26821=CARTESIAN_POINT('Ctrl Pts',(27.6545746161027,10.2440187011867,23.9508473575555));
#26822=CARTESIAN_POINT('Ctrl Pts',(27.6066964485145,10.3537263656175,24.0011654495696));
#26823=CARTESIAN_POINT('Ctrl Pts',(27.5547559674577,10.4613204844038,24.053392067875));
#26824=CARTESIAN_POINT('Ctrl Pts',(27.4988994001976,10.5662898659804,24.1073371292752));
#26825=CARTESIAN_POINT('Ctrl Pts',(27.440534703391,10.6759726916569,24.163704487802));
#26826=CARTESIAN_POINT('Ctrl Pts',(27.3778942432628,10.7827889482093,24.2219479645533));
#26827=CARTESIAN_POINT('Ctrl Pts',(27.3111952764661,10.8861779564386,24.2818262388331));
#26828=CARTESIAN_POINT('Ctrl Pts',(27.2444963096694,10.9895669646679,24.3417045131128));
#26829=CARTESIAN_POINT('Ctrl Pts',(27.1737391515792,11.0895280193203,24.4032172570693));
#26830=CARTESIAN_POINT('Ctrl Pts',(27.0991881374367,11.1855339059311,24.4661028860402));
#26831=CARTESIAN_POINT('Ctrl Pts',(27.0277522426528,11.2775281798315,24.5263608345907));
#26832=CARTESIAN_POINT('Ctrl Pts',(26.9528447452163,11.3658762863386,24.5878694828124));
#26833=CARTESIAN_POINT('Ctrl Pts',(26.8748382305686,11.4502607243407,24.6503480936848));
#26834=CARTESIAN_POINT('Ctrl Pts',(26.7951405471489,11.536474603474,24.7141812308569));
#26835=CARTESIAN_POINT('Ctrl Pts',(26.7122084062844,11.618550543237,24.7790265068645));
#26836=CARTESIAN_POINT('Ctrl Pts',(26.6264699330043,11.6961959778089,24.8445762727988));
#26837=CARTESIAN_POINT('Ctrl Pts',(26.5432983957594,11.7715167749532,24.9081635352054));
#26838=CARTESIAN_POINT('Ctrl Pts',(26.4574866227211,11.8426682993997,24.9724133860912));
#26839=CARTESIAN_POINT('Ctrl Pts',(26.3694465437975,11.9094303708384,25.0370424882597));
#26840=CARTESIAN_POINT('Ctrl Pts',(26.2822348440543,11.9755642703047,25.1010634878078));
#26841=CARTESIAN_POINT('Ctrl Pts',(26.1928370208142,12.0373907339768,25.1654563368694));
#26842=CARTESIAN_POINT('Ctrl Pts',(26.1016671448819,12.0947447723696,25.2299478696638));
#26843=CARTESIAN_POINT('Ctrl Pts',(26.0118619413472,12.1512403092862,25.2934740637014));
#26844=CARTESIAN_POINT('Ctrl Pts',(25.9203377427928,12.2033962128022,25.3570957555355));
#26845=CARTESIAN_POINT('Ctrl Pts',(25.8274973162755,12.2511046771407,25.4205581249819));
#26846=CARTESIAN_POINT('Ctrl Pts',(25.8154864725656,12.2572767611165,25.4287683048515));
#26847=CARTESIAN_POINT('Ctrl Pts',(25.8034536043297,12.2633744796122,25.4369758298899));
#26848=CARTESIAN_POINT('Ctrl Pts',(25.791399587074,12.269397662556,25.4451801594709));
#26849=CARTESIAN_POINT('Ctrl Pts',(25.6967038096742,12.3167154968669,25.509632976423));
#26850=CARTESIAN_POINT('Ctrl Pts',(25.60072916376,12.3594653682634,25.5738799902926));
#26851=CARTESIAN_POINT('Ctrl Pts',(25.5039422280259,12.3976812193475,25.6376588373852));
#26852=CARTESIAN_POINT('Ctrl Pts',(25.4085432294501,12.4353490501916,25.7005230875736));
#26853=CARTESIAN_POINT('Ctrl Pts',(25.3123554549748,12.4686120581704,25.7629322992041));
#26854=CARTESIAN_POINT('Ctrl Pts',(25.215816404023,12.4975498540577,25.8246503367211));
#26855=CARTESIAN_POINT('Ctrl Pts',(25.1455302814777,12.5186182760887,25.8695847078942));
#26856=CARTESIAN_POINT('Ctrl Pts',(25.0750577815132,12.5373950091753,25.9141530119682));
#26857=CARTESIAN_POINT('Ctrl Pts',(25.0045629008943,12.5539264020161,25.9582701452394));
#26858=CARTESIAN_POINT('Ctrl Pts',(24.9069617269622,12.5768143526563,26.0193509494053));
#26859=CARTESIAN_POINT('Ctrl Pts',(24.8093209549444,12.5953965821885,26.0795646604711));
#26860=CARTESIAN_POINT('Ctrl Pts',(24.7120718565095,12.6098896651051,26.1387070476852));
#26861=CARTESIAN_POINT('Ctrl Pts',(24.6157471715197,12.6242449822127,26.1972872495546));
#26862=CARTESIAN_POINT('Ctrl Pts',(24.5198070137702,12.634588716212,26.2548162852166));
#26863=CARTESIAN_POINT('Ctrl Pts',(24.4246450695825,12.6411692670537,26.3111182018749));
#26864=CARTESIAN_POINT('Ctrl Pts',(24.3385006102295,12.6471262491156,26.3620849849988));
#26865=CARTESIAN_POINT('Ctrl Pts',(24.252993681858,12.65,26.4120464123989));
#26866=CARTESIAN_POINT('Ctrl Pts',(24.1683956091399,12.65,26.4608891324556));
#26867=CARTESIAN_POINT('Ctrl Pts',(28.0510228507774,7.65,23.1857967818227));
#26868=CARTESIAN_POINT('Ctrl Pts',(28.0510228507774,7.65,23.1857967818227));
#26869=CARTESIAN_POINT('Ctrl Pts',(28.0510228507774,7.65,23.1857967818227));
#26870=CARTESIAN_POINT('Ctrl Pts',(28.1096109945774,8.30461645762897,23.2872744236054));
#26871=CARTESIAN_POINT('Ctrl Pts',(28.1827326335685,8.23864736688808,23.4139248174707));
#26872=CARTESIAN_POINT('Ctrl Pts',(28.256050107547,8.17355351675034,23.540914407484));
#26873=CARTESIAN_POINT('Ctrl Pts',(28.0554533489513,8.95873944331359,23.4537438809049));
#26874=CARTESIAN_POINT('Ctrl Pts',(28.2260332521862,8.83304537535202,23.6960674267152));
#26875=CARTESIAN_POINT('Ctrl Pts',(28.3482211841544,8.69671236121383,23.9608326462977));
#26876=CARTESIAN_POINT('Ctrl Pts',(27.7298712681797,10.1680948803373,23.8916820224643));
#26877=CARTESIAN_POINT('Ctrl Pts',(28.1174229188319,9.96758997398087,24.3450248584824));
#26878=CARTESIAN_POINT('Ctrl Pts',(28.2931745220997,9.66393871899201,24.8673518783236));
#26879=CARTESIAN_POINT('Ctrl Pts',(27.4585643389691,10.7227336174025,24.1629601490681));
#26880=CARTESIAN_POINT('Ctrl Pts',(27.9614466252574,10.5146815062456,24.7177754547336));
#26881=CARTESIAN_POINT('Ctrl Pts',(28.1459414742105,10.1075313875396,25.3535322712672));
#26882=CARTESIAN_POINT('Ctrl Pts',(26.7398119358942,11.648334194463,24.7692456230013));
#26883=CARTESIAN_POINT('Ctrl Pts',(27.427873623927,11.4817645043907,25.5255530602099));
#26884=CARTESIAN_POINT('Ctrl Pts',(27.634247915884,10.8478143907818,26.3184541844612));
#26885=CARTESIAN_POINT('Ctrl Pts',(26.2926491798939,12.0189319519099,25.1040144904058));
#26886=CARTESIAN_POINT('Ctrl Pts',(27.0436555217853,11.8983870794298,25.9626621322522));
#26887=CARTESIAN_POINT('Ctrl Pts',(27.2699886772591,11.1442135371051,26.7968161560863));
#26888=CARTESIAN_POINT('Ctrl Pts',(25.5407747906579,12.3946305178797,25.6157629939958));
#26889=CARTESIAN_POINT('Ctrl Pts',(26.313365510933,12.3384327759139,26.6116793021193));
#26890=CARTESIAN_POINT('Ctrl Pts',(26.6021588672628,11.4446922420911,27.4541341410199));
#26891=CARTESIAN_POINT('Ctrl Pts',(25.2768095107291,12.4900832460695,25.7878926672769));
#26892=CARTESIAN_POINT('Ctrl Pts',(26.0434829582219,12.4537748504032,26.8270965730057));
#26893=CARTESIAN_POINT('Ctrl Pts',(26.3595465684327,11.5210340617089,27.6632482624575));
#26894=CARTESIAN_POINT('Ctrl Pts',(24.732316291055,12.6177695579628,26.1286476231956));
#26895=CARTESIAN_POINT('Ctrl Pts',(25.4647461978773,12.6099538847864,27.2419325139665));
#26896=CARTESIAN_POINT('Ctrl Pts',(25.8436170520301,11.6231558718974,28.053477003694));
#26897=CARTESIAN_POINT('Ctrl Pts',(24.45180496607,12.65,26.2972626639395));
#26898=CARTESIAN_POINT('Ctrl Pts',(25.1571469337936,12.6499999999603,27.4402179902489));
#26899=CARTESIAN_POINT('Ctrl Pts',(25.5703157464209,11.6489333498045,28.2345801643211));
#26900=CARTESIAN_POINT('Ctrl Pts',(24.1683956091399,12.65,26.4608891324556));
#26901=CARTESIAN_POINT('Ctrl Pts',(24.8396452750671,12.65,27.623527658405));
#26902=CARTESIAN_POINT('Ctrl Pts',(25.2869063894896,11.6489333498058,28.3982066328348));
#26903=CARTESIAN_POINT('Ctrl Pts',(28.0510228507774,7.65,23.1857967818227));
#26904=CARTESIAN_POINT('Ctrl Pts',(28.0844275796731,7.73530164996095,23.243655469483));
#26905=CARTESIAN_POINT('Ctrl Pts',(28.1153375201379,7.82187906280546,23.3041082955208));
#26906=CARTESIAN_POINT('Ctrl Pts',(28.1434170892384,7.90943093574786,23.3670765172883));
#26907=CARTESIAN_POINT('Ctrl Pts',(28.1716624715014,7.99749981281107,23.4304165738212));
#26908=CARTESIAN_POINT('Ctrl Pts',(28.1970437461975,8.08655451224725,23.4963017794788));
#26909=CARTESIAN_POINT('Ctrl Pts',(28.2192417703173,8.1762600347923,23.5646134256722));
#26910=CARTESIAN_POINT('Ctrl Pts',(28.2417363220809,8.26716386972267,23.6338375986463));
#26911=CARTESIAN_POINT('Ctrl Pts',(28.2609617599807,8.35873581948415,23.7055534235978));
#26912=CARTESIAN_POINT('Ctrl Pts',(28.276612470514,8.45060120069979,23.7795984912439));
#26913=CARTESIAN_POINT('Ctrl Pts',(28.292398726102,8.54326219423563,23.8542848360207));
#26914=CARTESIAN_POINT('Ctrl Pts',(28.3045478312839,8.63622142494294,23.9313408096347));
#26915=CARTESIAN_POINT('Ctrl Pts',(28.3127765977397,8.72907194030857,24.0105618721281));
#26916=CARTESIAN_POINT('Ctrl Pts',(28.3211204590875,8.82322114607964,24.0908909913013));
#26917=CARTESIAN_POINT('Ctrl Pts',(28.3254332730565,8.91725821818692,24.1734460255698));
#26918=CARTESIAN_POINT('Ctrl Pts',(28.3254548896342,9.01074085424139,24.2579771641602));
#26919=CARTESIAN_POINT('Ctrl Pts',(28.3254680161717,9.06750762559021,24.3093081922392));
#26920=CARTESIAN_POINT('Ctrl Pts',(28.3238994826617,9.12406962268391,24.3613671988861));
#26921=CARTESIAN_POINT('Ctrl Pts',(28.3206978531259,9.18032554010459,24.4140922623076));
#26922=CARTESIAN_POINT('Ctrl Pts',(28.3155546727227,9.27069649927002,24.4987911663861));
#26923=CARTESIAN_POINT('Ctrl Pts',(28.3061939676307,9.36026087469428,24.5851956030652));
#26924=CARTESIAN_POINT('Ctrl Pts',(28.292553209215,9.44863173534435,24.6729917414403));
#26925=CARTESIAN_POINT('Ctrl Pts',(28.2781209564036,9.54213024643806,24.765882182446));
#26926=CARTESIAN_POINT('Ctrl Pts',(28.2588971002568,9.63429224123548,24.8603303412854));
#26927=CARTESIAN_POINT('Ctrl Pts',(28.234862192439,9.7246615788445,24.9559349227726));
#26928=CARTESIAN_POINT('Ctrl Pts',(28.2115258659209,9.81240430644903,25.0487607304318));
#26929=CARTESIAN_POINT('Ctrl Pts',(28.1836544212169,9.89845664842074,25.1426761425893));
#26930=CARTESIAN_POINT('Ctrl Pts',(28.1512797309364,9.98240976055992,25.2372930079755));
#26931=CARTESIAN_POINT('Ctrl Pts',(28.1174513187174,10.0701326224597,25.3361584580365));
#26932=CARTESIAN_POINT('Ctrl Pts',(28.078705885483,10.1555628405854,25.435789335416));
#26933=CARTESIAN_POINT('Ctrl Pts',(28.0351352627411,10.2382519911876,25.5357270766931));
#26934=CARTESIAN_POINT('Ctrl Pts',(27.9915646399991,10.3209411417899,25.6356648179701));
#26935=CARTESIAN_POINT('Ctrl Pts',(27.9431689853577,10.4008886608162,25.735908822033));
#26936=CARTESIAN_POINT('Ctrl Pts',(27.8900946950455,10.4776728891654,25.8359932278577));
#26937=CARTESIAN_POINT('Ctrl Pts',(27.839238117679,10.5512486831439,25.9318955997605));
#26938=CARTESIAN_POINT('Ctrl Pts',(27.7840942821528,10.6219083210448,26.0276359145545));
#26939=CARTESIAN_POINT('Ctrl Pts',(27.7249647482248,10.6893978697112,26.1228104151272));
#26940=CARTESIAN_POINT('Ctrl Pts',(27.6645532954503,10.7583505810078,26.2200482836633));
#26941=CARTESIAN_POINT('Ctrl Pts',(27.5999817192723,10.8239938235548,26.3166949905633));
#26942=CARTESIAN_POINT('Ctrl Pts',(27.531612697115,10.8860936071087,26.4123295283418));
#26943=CARTESIAN_POINT('Ctrl Pts',(27.4652905845881,10.9463341766357,26.5051008504386));
#26944=CARTESIAN_POINT('Ctrl Pts',(27.395395560976,11.0032402174354,26.5969193200223));
#26945=CARTESIAN_POINT('Ctrl Pts',(27.3222903013768,11.0566356322311,26.687416288063));
#26946=CARTESIAN_POINT('Ctrl Pts',(27.2498728975335,11.1095286434568,26.7770617597724));
#26947=CARTESIAN_POINT('Ctrl Pts',(27.1743057875189,11.1589766249525,26.865410106846));
#26948=CARTESIAN_POINT('Ctrl Pts',(27.0959661336344,11.2048476203275,26.9521242360999));
#26949=CARTESIAN_POINT('Ctrl Pts',(27.0187991035164,11.2500319976655,27.0375403886101));
#26950=CARTESIAN_POINT('Ctrl Pts',(26.9389422930304,11.2917455940572,27.1213705893704));
#26951=CARTESIAN_POINT('Ctrl Pts',(26.8567743528486,11.3299021878793,27.2033182473929));
#26952=CARTESIAN_POINT('Ctrl Pts',(26.8461442176319,11.3348385383688,27.2139198845222));
#26953=CARTESIAN_POINT('Ctrl Pts',(26.8354754221709,11.3397154123387,27.2244900529112));
#26954=CARTESIAN_POINT('Ctrl Pts',(26.8247688039266,11.3445326737677,27.2350281460368));
#26955=CARTESIAN_POINT('Ctrl Pts',(26.7406581280837,11.3823768469003,27.3178148966865));
#26956=CARTESIAN_POINT('Ctrl Pts',(26.6542467205738,11.4165676241853,27.3986259253548));
#26957=CARTESIAN_POINT('Ctrl Pts',(26.5660087531245,11.4471321524631,27.4772120198665));
#26958=CARTESIAN_POINT('Ctrl Pts',(26.4790361295247,11.4772583814579,27.5546711796332));
#26959=CARTESIAN_POINT('Ctrl Pts',(26.3902893616535,11.5038616918416,27.6299685927576));
#26960=CARTESIAN_POINT('Ctrl Pts',(26.3002237580355,11.5270057552498,27.702898969953));
#26961=CARTESIAN_POINT('Ctrl Pts',(26.2346506869213,11.5438559983479,27.7559965856699));
#26962=CARTESIAN_POINT('Ctrl Pts',(26.16837858263,11.5588733791764,27.8078401884681));
#26963=CARTESIAN_POINT('Ctrl Pts',(26.1015818102301,11.5720949668065,27.8583626330729));
#26964=CARTESIAN_POINT('Ctrl Pts',(26.009100720206,11.5904004446306,27.928311682703));
#26965=CARTESIAN_POINT('Ctrl Pts',(25.9156168330012,11.605262264108,27.9957253294626));
#26966=CARTESIAN_POINT('Ctrl Pts',(25.8216098684647,11.6168536386306,28.0604832573104));
#26967=CARTESIAN_POINT('Ctrl Pts',(25.7284964988654,11.6283348298957,28.1246256205907));
#26968=CARTESIAN_POINT('Ctrl Pts',(25.6348702567158,11.6366076104655,28.1861624756317));
#26969=CARTESIAN_POINT('Ctrl Pts',(25.5411803959419,11.6418706473094,28.2450141155512));
#26970=CARTESIAN_POINT('Ctrl Pts',(25.4563685263168,11.6466349621557,28.2982890117977));
#26971=CARTESIAN_POINT('Ctrl Pts',(25.371504462211,11.6489333498058,28.3493639127762));
#26972=CARTESIAN_POINT('Ctrl Pts',(25.2869063894896,11.6489333498058,28.3982066328348));
#26973=CARTESIAN_POINT('Origin',(30.6683956091398,-7.9,37.7192193816533));
#26974=CARTESIAN_POINT('Origin',(30.6683956091398,-7.9,37.7192193816533));
#26975=CARTESIAN_POINT('Origin',(30.6683956091398,-7.90000000000001,37.7192193816533));
#26976=CARTESIAN_POINT('Origin',(30.6683956091398,-7.90000000000001,37.7192193816533));
#26977=CARTESIAN_POINT('Origin',(30.6683956091398,-7.90000000000001,37.7192193816533));
#26978=CARTESIAN_POINT('Origin',(30.6683956091398,-21.9,37.7192193816533));
#26979=CARTESIAN_POINT('Ctrl Pts',(-15.5865359611318,-22.9,11.8009489759233));
#26980=CARTESIAN_POINT('Ctrl Pts',(-15.7517039698567,-22.9,12.7872144213759));
#26981=CARTESIAN_POINT('Ctrl Pts',(-15.7517039698567,-21.9,12.7872144213759));
#26982=CARTESIAN_POINT('Ctrl Pts',(-15.3559607473128,-22.9,11.9647821254064));
#26983=CARTESIAN_POINT('Ctrl Pts',(-15.5607856662629,-22.7827980547214,
12.8191871306933));
#26984=CARTESIAN_POINT('Ctrl Pts',(-15.4355591423194,-21.9000000281286,
12.8401585976865));
#26985=CARTESIAN_POINT('Ctrl Pts',(-15.1190374158585,-22.9205735494498,
12.1462781863217));
#26986=CARTESIAN_POINT('Ctrl Pts',(-15.2973142372118,-22.7172748074572,
12.8709905227205));
#26987=CARTESIAN_POINT('Ctrl Pts',(-15.1328683878844,-21.9617206530121,
12.915148108118));
#26988=CARTESIAN_POINT('Ctrl Pts',(-14.6271245805211,-22.9836857365403,
12.5399038917133));
#26989=CARTESIAN_POINT('Ctrl Pts',(-14.7359632242306,-22.6985884975707,
13.0355614944526));
#26990=CARTESIAN_POINT('Ctrl Pts',(-14.5466360368447,-22.151057204958,13.105466734237));
#26991=CARTESIAN_POINT('Ctrl Pts',(-14.3791131979057,-23.0257436937064,
12.7464145774642));
#26992=CARTESIAN_POINT('Ctrl Pts',(-14.4436326996405,-22.7356048512228,
13.1424140441331));
#26993=CARTESIAN_POINT('Ctrl Pts',(-14.2714100237779,-22.2772310832513,
13.2181656147264));
#26994=CARTESIAN_POINT('Ctrl Pts',(-13.6286677467523,-23.1675945141807,
13.383230113175));
#26995=CARTESIAN_POINT('Ctrl Pts',(-13.6265116615006,-22.9266590509653,
13.5179293418098));
#26996=CARTESIAN_POINT('Ctrl Pts',(-13.4894327977986,-22.7027835382778,
13.6005990193291));
#26997=CARTESIAN_POINT('Ctrl Pts',(-13.1126423384295,-23.2843988132411,
13.8357364471931));
#26998=CARTESIAN_POINT('Ctrl Pts',(-13.0648889625182,-23.1694382547404,
13.877850966168));
#26999=CARTESIAN_POINT('Ctrl Pts',(-13.0193938287046,-23.0534635976961,
13.9179739028129));
#27000=CARTESIAN_POINT('Ctrl Pts',(-12.6003906189451,-23.4,14.2875));
#27001=CARTESIAN_POINT('Ctrl Pts',(-12.6003906189451,-23.4,14.2875));
#27002=CARTESIAN_POINT('Ctrl Pts',(-12.6003906189451,-23.4,14.2875));
#27003=CARTESIAN_POINT('Origin',(-15.5865359611318,-21.9,11.8009489759233));
#27004=CARTESIAN_POINT('Origin',(-16.8005208252602,-21.9,19.05));
#27005=CARTESIAN_POINT('Origin',(-16.8005208252602,-21.9,11.7));
#27006=CARTESIAN_POINT('Origin',(-48.,-21.9,11.7));
#27007=CARTESIAN_POINT('Origin',(-48.,-21.9,11.7));
#27008=CARTESIAN_POINT('Origin',(-48.,-21.9,7.7));
#27009=CARTESIAN_POINT('Origin',(-52.,-21.9,7.7));
#27010=CARTESIAN_POINT('Origin',(-52.,-21.9,12.7));
#27011=CARTESIAN_POINT('Origin',(-52.,-21.9,-7.7));
#27012=CARTESIAN_POINT('Origin',(-48.,-21.9,-7.7));
#27013=CARTESIAN_POINT('Origin',(-48.,-21.9,-11.7));
#27014=CARTESIAN_POINT('Origin',(4.15723558123562E-15,-21.9,-11.7));
#27015=CARTESIAN_POINT('Origin',(-16.8005208252602,-21.9,-11.7));
#27016=CARTESIAN_POINT('Origin',(-16.8005208252602,-21.9,-19.05));
#27017=CARTESIAN_POINT('Origin',(-15.5865359611318,-21.9,-11.8009489759233));
#27018=CARTESIAN_POINT('Ctrl Pts',(-15.7517039698567,-21.9,-12.7872144213759));
#27019=CARTESIAN_POINT('Ctrl Pts',(-15.7517039698567,-22.9,-12.7872144213759));
#27020=CARTESIAN_POINT('Ctrl Pts',(-15.5865359611318,-22.9,-11.8009489759233));
#27021=CARTESIAN_POINT('Ctrl Pts',(-15.4355591423194,-21.9000000281286,
-12.8401585976865));
#27022=CARTESIAN_POINT('Ctrl Pts',(-15.5607856662644,-22.7827980547194,
-12.8191871306931));
#27023=CARTESIAN_POINT('Ctrl Pts',(-15.3559607473148,-22.9,-11.9647821254094));
#27024=CARTESIAN_POINT('Ctrl Pts',(-15.1328683878844,-21.9617206530121,
-12.915148108118));
#27025=CARTESIAN_POINT('Ctrl Pts',(-15.2973142372121,-22.7172748074559,
-12.8709905227205));
#27026=CARTESIAN_POINT('Ctrl Pts',(-15.1190374158585,-22.9205735494498,
-12.1462781863214));
#27027=CARTESIAN_POINT('Ctrl Pts',(-14.5466360368447,-22.151057204958,-13.105466734237));
#27028=CARTESIAN_POINT('Ctrl Pts',(-14.7359632242303,-22.6985884975719,
-13.0355614944526));
#27029=CARTESIAN_POINT('Ctrl Pts',(-14.6271245805211,-22.9836857365402,
-12.5399038917136));
#27030=CARTESIAN_POINT('Ctrl Pts',(-14.2714100237779,-22.2772310832513,
-13.2181656147264));
#27031=CARTESIAN_POINT('Ctrl Pts',(-14.4436326996405,-22.7356048512221,
-13.1424140441331));
#27032=CARTESIAN_POINT('Ctrl Pts',(-14.3791131979061,-23.0257436937059,
-12.7464145774643));
#27033=CARTESIAN_POINT('Ctrl Pts',(-13.4894327977986,-22.7027835382778,
-13.6005990193291));
#27034=CARTESIAN_POINT('Ctrl Pts',(-13.6265116615004,-22.9266590509666,
-13.5179293418098));
#27035=CARTESIAN_POINT('Ctrl Pts',(-13.6286677467514,-23.1675945141816,
-13.3832301131747));
#27036=CARTESIAN_POINT('Ctrl Pts',(-13.0193938287093,-23.0534635977063,
-13.9179739028087));
#27037=CARTESIAN_POINT('Ctrl Pts',(-13.0648889625215,-23.1694382547513,
-13.8778509661652));
#27038=CARTESIAN_POINT('Ctrl Pts',(-13.1126423384301,-23.2843988132432,
-13.8357364471925));
#27039=CARTESIAN_POINT('Ctrl Pts',(-12.6003906189451,-23.4,-14.2875));
#27040=CARTESIAN_POINT('Ctrl Pts',(-12.6003906189451,-23.4,-14.2875));
#27041=CARTESIAN_POINT('Ctrl Pts',(-12.6003906189451,-23.4,-14.2875));
#27042=CARTESIAN_POINT('Ctrl Pts',(18.9499045174787,-21.9,-7.24776858010006));
#27043=CARTESIAN_POINT('Ctrl Pts',(18.9499045174787,-22.9,-7.24776858010006));
#27044=CARTESIAN_POINT('Ctrl Pts',(18.0131895824795,-22.9,-7.59786161137808));
#27045=CARTESIAN_POINT('Ctrl Pts',(18.8376831053774,-21.9000000281286,-6.94750704002252));
#27046=CARTESIAN_POINT('Ctrl Pts',(18.8821345441792,-22.7827980547207,-7.06644212448199));
#27047=CARTESIAN_POINT('Ctrl Pts',(18.0397856450054,-22.9,-7.31626104398644));
#27048=CARTESIAN_POINT('Ctrl Pts',(18.7512805492109,-21.9617206530127,-6.64787440197507));
#27049=CARTESIAN_POINT('Ctrl Pts',(18.7952618831513,-22.7172748074566,-6.81236747773836));
#27050=CARTESIAN_POINT('Ctrl Pts',(18.0785041787165,-22.9205735494498,-7.02033138973984));
#27051=CARTESIAN_POINT('Ctrl Pts',(18.6229851387236,-22.1510572049574,-6.04502298039525));
#27052=CARTESIAN_POINT('Ctrl Pts',(18.6571090189048,-22.6985884975713,-6.24393775419057));
#27053=CARTESIAN_POINT('Ctrl Pts',(18.1734376214998,-22.9836857365402,-6.39750952519446));
#27054=CARTESIAN_POINT('Ctrl Pts',(18.582972225672,-22.2772310832513,-5.75032082105227));
#27055=CARTESIAN_POINT('Ctrl Pts',(18.6034807790932,-22.7356048512228,-5.93734581875364));
#27056=CARTESIAN_POINT('Ctrl Pts',(18.2282754302052,-23.0257436937062,-6.07947002454654));
#27057=CARTESIAN_POINT('Ctrl Pts',(18.5231806563241,-22.7027835382778,-4.88189197587188));
#27058=CARTESIAN_POINT('Ctrl Pts',(18.5201260473201,-22.9266590509653,-5.04194059291939));
#27059=CARTESIAN_POINT('Ctrl Pts',(18.4045511360785,-23.1675945141811,-5.11115743183685));
#27060=CARTESIAN_POINT('Ctrl Pts',(18.5630158834026,-23.0534635976512,-4.31613884609869));
#27061=CARTESIAN_POINT('Ctrl Pts',(18.5510159678978,-23.1694382547042,-4.37560025606624));
#27062=CARTESIAN_POINT('Ctrl Pts',(18.5384204125509,-23.2843988132179,-4.43801315221929));
#27063=CARTESIAN_POINT('Ctrl Pts',(18.6735332660427,-23.4,-3.76850837361349));
#27064=CARTESIAN_POINT('Ctrl Pts',(18.6735332660427,-23.4,-3.76850837361349));
#27065=CARTESIAN_POINT('Ctrl Pts',(18.6735332660427,-23.4,-3.76850837361349));
#27066=CARTESIAN_POINT('Origin',(18.0131895824795,-21.9,-7.59786161137808));
#27067=CARTESIAN_POINT('Origin',(24.8980443547237,-21.9,-5.02467783148466));
#27068=CARTESIAN_POINT('Origin',(18.5327576369081,-21.9,-8.69967783148469));
#27069=CARTESIAN_POINT('Origin',(10.1324972242779,-21.9,5.85000000000005));
#27070=CARTESIAN_POINT('Origin',(34.1324972242781,-21.9,-35.7192193816529));
#27071=CARTESIAN_POINT('Origin',(30.6683956091404,-21.9,-37.7192193816529));
#27072=CARTESIAN_POINT('Origin',(32.6683956091404,-21.9,-41.1833209967907));
#27073=CARTESIAN_POINT('Origin',(15.0014773719379,-21.9,-51.3833209967907));
#27074=CARTESIAN_POINT('Origin',(19.3316043908601,-21.9,-48.8833209967907));
#27075=CARTESIAN_POINT('Origin',(17.33160439086,-21.9,-45.419219381653));
#27076=CARTESIAN_POINT('Origin',(13.8675027757223,-21.9,-47.419219381653));
#27077=CARTESIAN_POINT('Origin',(13.8675027757223,-21.9,-47.419219381653));
#27078=CARTESIAN_POINT('Origin',(-1.73223681164776,-21.9,-20.3996778314848));
#27079=CARTESIAN_POINT('Origin',(-8.09752352946338,-21.9,-24.0746778314848));
#27080=CARTESIAN_POINT('Origin',(-2.42665362134758,-21.9,-19.3988105873015));
#27081=CARTESIAN_POINT('Ctrl Pts',(-2.42665362134758,-22.9,-19.3988105873015));
#27082=CARTESIAN_POINT('Ctrl Pts',(-3.19820054762184,-22.9,-20.0349830014761));
#27083=CARTESIAN_POINT('Ctrl Pts',(-3.19820054762184,-21.9,-20.0349830014761));
#27084=CARTESIAN_POINT('Ctrl Pts',(-2.6838248976923,-22.9,-19.281043169395));
#27085=CARTESIAN_POINT('Ctrl Pts',(-3.32134887791377,-22.7827980547212,
-19.8856292551749));
#27086=CARTESIAN_POINT('Ctrl Pts',(-3.40212396305772,-21.9000000281286,
-19.7876656377092));
#27087=CARTESIAN_POINT('Ctrl Pts',(-2.9594667628583,-22.9205735494497,-19.1666095760619));
#27088=CARTESIAN_POINT('Ctrl Pts',(-3.49794764593905,-22.7172748074552,
-19.6833580004591));
#27089=CARTESIAN_POINT('Ctrl Pts',(-3.61841216132671,-21.9617206530128,
-19.5630225100931));
#27090=CARTESIAN_POINT('Ctrl Pts',(-3.54631304097816,-22.9836857365404,
-18.9374134169076));
#27091=CARTESIAN_POINT('Ctrl Pts',(-3.92114579467461,-22.6985884975725,
-19.2794992486431));
#27092=CARTESIAN_POINT('Ctrl Pts',(-4.07634910187847,-22.1510572049574,
-19.1504897146324));
#27093=CARTESIAN_POINT('Ctrl Pts',(-3.84916223229935,-23.0257436937064,
-18.8258846020106));
#27094=CARTESIAN_POINT('Ctrl Pts',(-4.15984807945244,-22.7356048512215,
-19.0797598628861));
#27095=CARTESIAN_POINT('Ctrl Pts',(-4.31156220189444,-22.2772310832507,
-18.9684864357784));
#27096=CARTESIAN_POINT('Ctrl Pts',(-4.77588338932629,-23.1675945141807,
-18.4943875450126));
#27097=CARTESIAN_POINT('Ctrl Pts',(-4.8936143858196,-22.9266590509677,-18.5598699347309));
#27098=CARTESIAN_POINT('Ctrl Pts',(-5.03374785852442,-22.702783538279,-18.4824909952018));
#27099=CARTESIAN_POINT('Ctrl Pts',(-5.42577807412219,-23.2843988132312,
-18.2737495994153));
#27100=CARTESIAN_POINT('Ctrl Pts',(-5.48612700538341,-23.169438254721,-18.2534512222455));
#27101=CARTESIAN_POINT('Ctrl Pts',(-5.54362205470623,-23.053463597673,-18.2341127489343));
#27102=CARTESIAN_POINT('Ctrl Pts',(-6.07314264709753,-23.4,-18.0560083736136));
#27103=CARTESIAN_POINT('Ctrl Pts',(-6.07314264709753,-23.4,-18.0560083736136));
#27104=CARTESIAN_POINT('Ctrl Pts',(-6.07314264709753,-23.4,-18.0560083736136));
#27105=CARTESIAN_POINT('Ctrl Pts',(-3.19820054762209,-21.9,20.0349830014761));
#27106=CARTESIAN_POINT('Ctrl Pts',(-3.19820054762209,-22.9,20.0349830014761));
#27107=CARTESIAN_POINT('Ctrl Pts',(-2.42665362134782,-22.9,19.3988105873015));
#27108=CARTESIAN_POINT('Ctrl Pts',(-3.40212396305782,-21.9000000281286,
19.7876656377093));
#27109=CARTESIAN_POINT('Ctrl Pts',(-3.32134887791476,-22.7827980547218,
19.8856292551756));
#27110=CARTESIAN_POINT('Ctrl Pts',(-2.68382489769184,-22.9,19.2810431693938));
#27111=CARTESIAN_POINT('Ctrl Pts',(-3.61841216132718,-21.9617206530121,
19.5630225100929));
#27112=CARTESIAN_POINT('Ctrl Pts',(-3.49794764593911,-22.7172748074559,
19.6833580004577));
#27113=CARTESIAN_POINT('Ctrl Pts',(-2.95946676285849,-22.9205735494499,
19.1666095760613));
#27114=CARTESIAN_POINT('Ctrl Pts',(-4.07634910187848,-22.151057204958,19.1504897146326));
#27115=CARTESIAN_POINT('Ctrl Pts',(-3.92114579467499,-22.6985884975719,
19.2794992486443));
#27116=CARTESIAN_POINT('Ctrl Pts',(-3.54631304097847,-22.9836857365401,
18.9374134169081));
#27117=CARTESIAN_POINT('Ctrl Pts',(-4.31156220189439,-22.2772310832513,
18.9684864357786));
#27118=CARTESIAN_POINT('Ctrl Pts',(-4.15984807945252,-22.7356048512228,
19.079759862886));
#27119=CARTESIAN_POINT('Ctrl Pts',(-3.84916223229944,-23.0257436937064,
18.8258846020105));
#27120=CARTESIAN_POINT('Ctrl Pts',(-5.03374785852525,-22.7027835382778,
18.4824909952013));
#27121=CARTESIAN_POINT('Ctrl Pts',(-4.89361438582019,-22.9266590509653,
18.5598699347308));
#27122=CARTESIAN_POINT('Ctrl Pts',(-4.77588338932682,-23.1675945141806,
18.4943875450126));
#27123=CARTESIAN_POINT('Ctrl Pts',(-5.54362205469395,-23.0534635976944,
18.2341127489385));
#27124=CARTESIAN_POINT('Ctrl Pts',(-5.48612700537819,-23.1694382547378,
18.2534512222473));
#27125=CARTESIAN_POINT('Ctrl Pts',(-5.42577807412138,-23.2843988132367,
18.2737495994156));
#27126=CARTESIAN_POINT('Ctrl Pts',(-6.07314264709777,-23.4,18.0560083736135));
#27127=CARTESIAN_POINT('Ctrl Pts',(-6.07314264709777,-23.4,18.0560083736135));
#27128=CARTESIAN_POINT('Ctrl Pts',(-6.07314264709777,-23.4,18.0560083736135));
#27129=CARTESIAN_POINT('Origin',(-2.42665362134782,-21.9,19.3988105873015));
#27130=CARTESIAN_POINT('Origin',(-8.09752352946369,-21.9,24.0746778314847));
#27131=CARTESIAN_POINT('Origin',(-1.73223681164803,-21.9,20.3996778314848));
#27132=CARTESIAN_POINT('Origin',(-10.132497224278,-21.9,5.8499999999999));
#27133=CARTESIAN_POINT('Origin',(36.998522628062,-21.9,38.6833209967911));
#27134=CARTESIAN_POINT('Origin',(32.6683956091398,-21.9,41.1833209967911));
#27135=CARTESIAN_POINT('Origin',(30.6683956091398,-21.9,37.7192193816533));
#27136=CARTESIAN_POINT('Origin',(34.1324972242776,-21.9,35.7192193816534));
#27137=CARTESIAN_POINT('Origin',(34.1324972242776,-21.9,35.7192193816534));
#27138=CARTESIAN_POINT('Origin',(18.5327576369079,-21.9,8.69967783148496));
#27139=CARTESIAN_POINT('Origin',(24.8980443547236,-21.9,5.02467783148503));
#27140=CARTESIAN_POINT('Origin',(18.0131895824794,-21.9,7.59786161137834));
#27141=CARTESIAN_POINT('Ctrl Pts',(18.0131895824794,-22.9,7.59786161137834));
#27142=CARTESIAN_POINT('Ctrl Pts',(18.9499045174786,-22.9,7.24776858010034));
#27143=CARTESIAN_POINT('Ctrl Pts',(18.9499045174786,-21.9,7.24776858010033));
#27144=CARTESIAN_POINT('Ctrl Pts',(18.0397856450098,-22.9,7.31626104398709));
#27145=CARTESIAN_POINT('Ctrl Pts',(18.8821345441806,-22.7827980547183,7.06644212448328));
#27146=CARTESIAN_POINT('Ctrl Pts',(18.8376831053773,-21.9000000281286,6.9475070400228));
#27147=CARTESIAN_POINT('Ctrl Pts',(18.0785041787167,-22.9205735494497,7.02033138974019));
#27148=CARTESIAN_POINT('Ctrl Pts',(18.7952618831505,-22.7172748074566,6.81236747773876));
#27149=CARTESIAN_POINT('Ctrl Pts',(18.7512805492108,-21.9617206530121,6.64787440197535));
#27150=CARTESIAN_POINT('Ctrl Pts',(18.1734376214995,-22.9836857365403,6.39750952519463));
#27151=CARTESIAN_POINT('Ctrl Pts',(18.6571090189054,-22.6985884975713,6.24393775419066));
#27152=CARTESIAN_POINT('Ctrl Pts',(18.6229851387235,-22.151057204958,6.04502298039552));
#27153=CARTESIAN_POINT('Ctrl Pts',(18.2282754302052,-23.0257436937062,6.0794700245468));
#27154=CARTESIAN_POINT('Ctrl Pts',(18.6034807790925,-22.7356048512234,5.93734581875439));
#27155=CARTESIAN_POINT('Ctrl Pts',(18.5829722256719,-22.2772310832513,5.75032082105249));
#27156=CARTESIAN_POINT('Ctrl Pts',(18.4045511360784,-23.1675945141811,5.11115743183711));
#27157=CARTESIAN_POINT('Ctrl Pts',(18.5201260473212,-22.9266590509641,5.04194059291876));
#27158=CARTESIAN_POINT('Ctrl Pts',(18.523180656324,-22.7027835382778,4.88189197587223));
#27159=CARTESIAN_POINT('Ctrl Pts',(18.5384204125495,-23.2843988132564,4.43801315222598));
#27160=CARTESIAN_POINT('Ctrl Pts',(18.5510159678927,-23.1694382547702,4.37560025609122));
#27161=CARTESIAN_POINT('Ctrl Pts',(18.5630158833926,-23.053463597732,4.31613884614811));
#27162=CARTESIAN_POINT('Ctrl Pts',(18.6735332660427,-23.4,3.76850837361377));
#27163=CARTESIAN_POINT('Ctrl Pts',(18.6735332660427,-23.4,3.76850837361377));
#27164=CARTESIAN_POINT('Ctrl Pts',(18.6735332660427,-23.4,3.76850837361377));
#27165=CARTESIAN_POINT('',(0.,0.,0.));
#27166=CARTESIAN_POINT('Ctrl Pts',(4.99864419322373,-21.608305818412,10.8906322767302));
#27167=CARTESIAN_POINT('Ctrl Pts',(4.99883364334396,-21.6179081044763,11.7031708025873));
#27168=CARTESIAN_POINT('Ctrl Pts',(5.72391665153499,-21.5966350540385,11.3369690930511));
#27169=CARTESIAN_POINT('Ctrl Pts',(5.00698491717006,-21.9683819493214,10.8859593746152));
#27170=CARTESIAN_POINT('Ctrl Pts',(5.00568014694611,-21.9487593964398,11.700455499203));
#27171=CARTESIAN_POINT('Ctrl Pts',(5.73346753777204,-21.9927228607166,11.3321045753797));
#27172=CARTESIAN_POINT('Ctrl Pts',(4.97681790987538,-22.3214319362742,10.903022409287));
#27173=CARTESIAN_POINT('Ctrl Pts',(4.98154299652122,-22.2686534039265,11.7100742339915));
#27174=CARTESIAN_POINT('Ctrl Pts',(5.69892353458948,-22.3810823369386,11.3498673084045));
#27175=CARTESIAN_POINT('Ctrl Pts',(4.84821686874648,-22.9911597054847,10.9728701997679));
#27176=CARTESIAN_POINT('Ctrl Pts',(4.87172013085809,-22.8940685954447,11.7530513658957));
#27177=CARTESIAN_POINT('Ctrl Pts',(5.55166363360174,-23.1177906197389,11.4225792046101));
#27178=CARTESIAN_POINT('Ctrl Pts',(4.75280187594809,-23.3116970781571,11.0240130526473));
#27179=CARTESIAN_POINT('Ctrl Pts',(4.79059840005532,-23.1963542824898,11.7847242777248));
#27180=CARTESIAN_POINT('Ctrl Pts',(5.44240468437886,-23.4703854977074,11.4758191935635));
#27181=CARTESIAN_POINT('Ctrl Pts',(4.50592320341294,-23.9166636689606,11.1487513379524));
#27182=CARTESIAN_POINT('Ctrl Pts',(4.56891533871215,-23.784060286346,11.868052837188));
#27183=CARTESIAN_POINT('Ctrl Pts',(5.15970603065283,-24.1358555142914,11.605672265421));
#27184=CARTESIAN_POINT('Ctrl Pts',(4.35465771842323,-24.2035260698023,11.2222713469962));
#27185=CARTESIAN_POINT('Ctrl Pts',(4.43153279702055,-24.0685058089498,11.9186637657369));
#27186=CARTESIAN_POINT('Ctrl Pts',(4.98649309301282,-24.4514073295638,11.6822068961658));
#27187=CARTESIAN_POINT('Ctrl Pts',(3.99621871821646,-24.747643148554,11.3824972363738));
#27188=CARTESIAN_POINT('Ctrl Pts',(4.09216913012772,-24.6194703396761,12.0353086028313));
#27189=CARTESIAN_POINT('Ctrl Pts',(4.57604742933995,-25.0499419971568,11.8490025577107));
#27190=CARTESIAN_POINT('Ctrl Pts',(3.79223436493213,-24.9994962931869,11.4676424780953));
#27191=CARTESIAN_POINT('Ctrl Pts',(3.89587775698716,-24.880259680682,12.0995329053305));
#27192=CARTESIAN_POINT('Ctrl Pts',(4.34246643061078,-25.3269830936796,11.9376389892933));
#27193=CARTESIAN_POINT('Ctrl Pts',(3.45427885759424,-25.3435355466136,11.593909463285));
#27194=CARTESIAN_POINT('Ctrl Pts',(3.5593346006441,-25.2431905195649,12.1987939611122));
#27195=CARTESIAN_POINT('Ctrl Pts',(3.95547616613724,-25.7054297215759,12.0690831535375));
#27196=CARTESIAN_POINT('Ctrl Pts',(3.33602937785994,-25.4528825858882,11.6358715221986));
#27197=CARTESIAN_POINT('Ctrl Pts',(3.44182785331483,-25.35834649947,12.2319414526239));
#27198=CARTESIAN_POINT('Ctrl Pts',(3.82006949082991,-25.8257126129142,12.1127657467956));
#27199=CARTESIAN_POINT('Ctrl Pts',(3.08792996304833,-25.6608466898983,11.7184463463716));
#27200=CARTESIAN_POINT('Ctrl Pts',(3.19329244351081,-25.5781989955108,12.2979140331202));
#27201=CARTESIAN_POINT('Ctrl Pts',(3.53597248666522,-26.0544753237534,12.1987263107462));
#27202=CARTESIAN_POINT('Ctrl Pts',(2.95738179070761,-25.7598839936288,11.7592458546648));
#27203=CARTESIAN_POINT('Ctrl Pts',(3.0616485141192,-25.6836426250107,12.3309331047788));
#27204=CARTESIAN_POINT('Ctrl Pts',(3.38648260575685,-26.163417392629,12.2411986733987));
#27205=CARTESIAN_POINT('Ctrl Pts',(2.55511469027868,-26.0351012414329,11.8757244107345));
#27206=CARTESIAN_POINT('Ctrl Pts',(2.65679594043675,-25.9750106533199,12.4252277213909));
#27207=CARTESIAN_POINT('Ctrl Pts',(2.92584880312279,-26.4661594138917,12.362453120026));
#27208=CARTESIAN_POINT('Ctrl Pts',(2.27166012221888,-26.1910580609653,11.9460131777189));
#27209=CARTESIAN_POINT('Ctrl Pts',(2.36557359217751,-26.144410994428,12.4841667316537));
#27210=CARTESIAN_POINT('Ctrl Pts',(2.60126664333885,-26.6377134749538,12.4356238030185));
#27211=CARTESIAN_POINT('Ctrl Pts',(1.67298569393372,-26.4480533981848,12.0650208326994));
#27212=CARTESIAN_POINT('Ctrl Pts',(1.7476443014938,-26.4221373472383,12.584193569546));
#27213=CARTESIAN_POINT('Ctrl Pts',(1.91572775104536,-26.920411071464,12.5595109498063));
#27214=CARTESIAN_POINT('Ctrl Pts',(1.35365874382953,-26.5495415074398,12.114005519406));
#27215=CARTESIAN_POINT('Ctrl Pts',(1.41459460586887,-26.5335291638453,12.6263023633275));
#27216=CARTESIAN_POINT('Ctrl Pts',(1.55006815385439,-27.0320490032883,12.610504042265));
#27217=CARTESIAN_POINT('Ctrl Pts',(0.708759568526575,-26.685469004934,12.1802503963495));
#27218=CARTESIAN_POINT('Ctrl Pts',(0.742700211667052,-26.681396361373,12.6829030413056));
#27219=CARTESIAN_POINT('Ctrl Pts',(0.811597193074135,-27.1815707028637,
12.6794650457788));
#27220=CARTESIAN_POINT('Ctrl Pts',(0.381529450169107,-26.7214769991791,
12.1982295563787));
#27221=CARTESIAN_POINT('Ctrl Pts',(0.39883067063808,-26.721134815956,12.6985538974327));
#27222=CARTESIAN_POINT('Ctrl Pts',(0.436887620603506,-27.2211798544626,
12.6981813593444));
#27223=CARTESIAN_POINT('Ctrl Pts',(-0.11672432528406,-26.7263960269428,
12.2006688310083));
#27224=CARTESIAN_POINT('Ctrl Pts',(-0.121960033275976,-26.7264982085473,
12.7006498339556));
#27225=CARTESIAN_POINT('Ctrl Pts',(-0.13366049259157,-27.226590836366,12.7007206478696));
#27226=CARTESIAN_POINT('Ctrl Pts',(-0.284953721660202,-26.7196403876827,
12.1973109610589));
#27227=CARTESIAN_POINT('Ctrl Pts',(-0.298043404871046,-26.71910948222,12.69775442877));
#27228=CARTESIAN_POINT('Ctrl Pts',(-0.326299187379028,-27.219159562167,
12.6972251018568));
#27229=CARTESIAN_POINT('Ctrl Pts',(-0.616054324255102,-26.6896861218385,
12.1825046937998));
#27230=CARTESIAN_POINT('Ctrl Pts',(-0.643871216622145,-26.6864670918352,
12.6850470220168));
#27231=CARTESIAN_POINT('Ctrl Pts',(-0.70544095955049,-27.1862095499586,
12.6818117584869));
#27232=CARTESIAN_POINT('Ctrl Pts',(-0.779654440780969,-26.6665839293988,
12.1711045612618));
#27233=CARTESIAN_POINT('Ctrl Pts',(-0.814871506455407,-26.6612250484592,
12.6752407488006));
#27234=CARTESIAN_POINT('Ctrl Pts',(-0.892778674333035,-27.1607968950611,
12.6699442088688));
#27235=CARTESIAN_POINT('Ctrl Pts',(-1.10308417480477,-26.6045817512992,
12.1407978831975));
#27236=CARTESIAN_POINT('Ctrl Pts',(-1.15201059362342,-26.5937532945347,
12.6493224876276));
#27237=CARTESIAN_POINT('Ctrl Pts',(-1.26313652698652,-27.0925938369454,
12.6383949174095));
#27238=CARTESIAN_POINT('Ctrl Pts',(-1.26291351966876,-26.5656809459862,
12.1218902629486));
#27239=CARTESIAN_POINT('Ctrl Pts',(-1.3185970928561,-26.55133271456,12.6331387123477));
#27240=CARTESIAN_POINT('Ctrl Pts',(-1.44615632156059,-27.0498025433814,
12.6187120638605));
#27241=CARTESIAN_POINT('Ctrl Pts',(-1.57882910825917,-26.472045523799,12.0770004764839));
#27242=CARTESIAN_POINT('Ctrl Pts',(-1.64674489658538,-26.4496895602423,
12.5949866446668));
#27243=CARTESIAN_POINT('Ctrl Pts',(-1.80790969162943,-26.9468025811083,
12.5719817348827));
#27244=CARTESIAN_POINT('Ctrl Pts',(-1.7357664458342,-26.4169293390886,12.0508406581823));
#27245=CARTESIAN_POINT('Ctrl Pts',(-1.80956942120921,-26.3897811738161,
12.5727721171669));
#27246=CARTESIAN_POINT('Ctrl Pts',(-1.98761782339906,-26.8861742010614,
12.5447493327003));
#27247=CARTESIAN_POINT('Ctrl Pts',(-2.19294340094436,-26.2304792608021,
11.9639571152858));
#27248=CARTESIAN_POINT('Ctrl Pts',(-2.28460854688898,-26.1870098690536,
12.4991934983994));
#27249=CARTESIAN_POINT('Ctrl Pts',(-2.51112856541472,-26.6810772067274,
12.4543034671678));
#27250=CARTESIAN_POINT('Ctrl Pts',(-2.48019406540275,-26.0786113976599,
11.8949950968601));
#27251=CARTESIAN_POINT('Ctrl Pts',(-2.58014891835197,-26.0218933438711,
12.4412197385113));
#27252=CARTESIAN_POINT('Ctrl Pts',(-2.84005763385079,-26.5140210366101,
12.3825139332799));
#27253=CARTESIAN_POINT('Ctrl Pts',(-3.0221032942732,-25.7215217624029,11.742358595615));
#27254=CARTESIAN_POINT('Ctrl Pts',(-3.13102074266629,-25.6402445849069,
12.3162445020822));
#27255=CARTESIAN_POINT('Ctrl Pts',(-3.4605946074415,-26.1212186661171,12.223619062105));
#27256=CARTESIAN_POINT('Ctrl Pts',(-3.27719005316914,-25.5149405044532,
11.6582504274636));
#27257=CARTESIAN_POINT('Ctrl Pts',(-3.38703375447497,-25.419666275089,12.2483547934178));
#27258=CARTESIAN_POINT('Ctrl Pts',(-3.75269279737139,-25.8939771831764,
12.1360623135586));
#27259=CARTESIAN_POINT('Ctrl Pts',(-3.73612218146736,-25.0634149529074,
11.4900064799871));
#27260=CARTESIAN_POINT('Ctrl Pts',(-3.84117285767248,-24.9466832868258,
12.1166714943089));
#27261=CARTESIAN_POINT('Ctrl Pts',(-4.27821277731412,-25.3972942939697,
11.960919972182));
#27262=CARTESIAN_POINT('Ctrl Pts',(-3.9428591300061,-24.8169069162524,11.4050875170057));
#27263=CARTESIAN_POINT('Ctrl Pts',(-4.04093407956023,-24.6906342031624,
12.0521900648229));
#27264=CARTESIAN_POINT('Ctrl Pts',(-4.51494576615864,-25.1261328819914,
11.8725191056138));
#27265=CARTESIAN_POINT('Ctrl Pts',(-4.31056667036922,-24.2794160099143,
11.2429469206136));
#27266=CARTESIAN_POINT('Ctrl Pts',(-4.39056436964167,-24.1445715889292,
11.9333269822134));
#27267=CARTESIAN_POINT('Ctrl Pts',(-4.93600478532903,-24.5348870880994,
11.7037302415389));
#27268=CARTESIAN_POINT('Ctrl Pts',(-4.46745152170304,-23.9937229399016,
11.1675387733309));
#27269=CARTESIAN_POINT('Ctrl Pts',(-4.53383740962333,-23.86015852534,11.8809582569124));
#27270=CARTESIAN_POINT('Ctrl Pts',(-5.11565242286094,-24.2206215634778,
11.6252300596616));
#27271=CARTESIAN_POINT('Ctrl Pts',(-4.65922173876165,-23.5465266850194,
11.0715060585919));
#27272=CARTESIAN_POINT('Ctrl Pts',(-4.70540726860683,-23.4277698236053,
11.8168401515203));
#27273=CARTESIAN_POINT('Ctrl Pts',(-5.33524695956652,-23.7287004880997,
11.5252595713033));
#27274=CARTESIAN_POINT('Ctrl Pts',(-4.71608662573261,-23.3939539209264,
11.0422301701708));
#27275=CARTESIAN_POINT('Ctrl Pts',(-4.7557251197416,-23.2807813557057,11.7976839118));
#27276=CARTESIAN_POINT('Ctrl Pts',(-5.40036246187489,-23.5608687218702,
11.4947832415057));
#27277=CARTESIAN_POINT('Ctrl Pts',(-4.81528967505078,-23.0814164438215,
10.9903022583832));
#27278=CARTESIAN_POINT('Ctrl Pts',(-4.84282117938902,-22.9825138810756,
11.7642375532091));
#27279=CARTESIAN_POINT('Ctrl Pts',(-5.51395900583216,-23.2170739466321,
11.4407260503891));
#27280=CARTESIAN_POINT('Ctrl Pts',(-4.85782281130184,-22.9204654286535,
10.9675445919213));
#27281=CARTESIAN_POINT('Ctrl Pts',(-4.87941790820092,-22.8307997636199,
11.750008368624));
#27282=CARTESIAN_POINT('Ctrl Pts',(-5.5626633344584,-23.0400259697853,11.4170352072457));
#27283=CARTESIAN_POINT('Ctrl Pts',(-4.96283908675816,-22.4231124826611,
10.9107685647248));
#27284=CARTESIAN_POINT('Ctrl Pts',(-4.96989390455362,-22.3626227944554,
11.7146772216865));
#27285=CARTESIAN_POINT('Ctrl Pts',(-5.68291650617108,-22.4929321295635,
11.3579310989885));
#27286=CARTESIAN_POINT('Ctrl Pts',(-4.99857193949256,-22.0854699970494,
10.8906542554823));
#27287=CARTESIAN_POINT('Ctrl Pts',(-4.99871428575359,-22.0557131075165,
11.7032123083642));
#27288=CARTESIAN_POINT('Ctrl Pts',(-5.72383391223237,-22.1215213732838,
11.3369919725727));
#27289=CARTESIAN_POINT('Ctrl Pts',(-4.9999606548595,-21.7450738646105,10.8898978613776));
#27290=CARTESIAN_POINT('Ctrl Pts',(-4.9999232845375,-21.7434332325445,11.7027395821881));
#27291=CARTESIAN_POINT('Ctrl Pts',(-5.72542411954922,-21.7470814748957,
11.3362045626284));
#27292=CARTESIAN_POINT('',(-4.99974790012546,-21.775208915454,10.8900436331349));
#27293=CARTESIAN_POINT('',(5.00000093190807,-21.7249999999251,10.8899036431084));
#27294=CARTESIAN_POINT('Ctrl Pts',(-4.99974790012546,-21.775208915454,10.8900436331349));
#27295=CARTESIAN_POINT('Ctrl Pts',(-4.99862155597278,-21.8873690121469,
10.8906693458292));
#27296=CARTESIAN_POINT('Ctrl Pts',(-4.99372822121316,-21.9992115592643,
10.8933945121638));
#27297=CARTESIAN_POINT('Ctrl Pts',(-4.98509810138154,-22.1107420376394,
10.8981732472158));
#27298=CARTESIAN_POINT('Ctrl Pts',(-4.97648594371211,-22.2220403838331,
10.9029420361238));
#27299=CARTESIAN_POINT('Ctrl Pts',(-4.96415246845925,-22.3330286474081,
10.9097558543201));
#27300=CARTESIAN_POINT('Ctrl Pts',(-4.94807614325441,-22.4437088983424,
10.9185691027912));
#27301=CARTESIAN_POINT('Ctrl Pts',(-4.93284610808526,-22.5485627186516,
10.9269184041682));
#27302=CARTESIAN_POINT('Ctrl Pts',(-4.91425644508413,-22.653140568427,10.9370621685552));
#27303=CARTESIAN_POINT('Ctrl Pts',(-4.89224714016671,-22.757433009706,10.9489616257723));
#27304=CARTESIAN_POINT('Ctrl Pts',(-4.86468603771555,-22.8880329841149,
10.9638626942388));
#27305=CARTESIAN_POINT('Ctrl Pts',(-4.83202306043748,-23.0169058067954,
10.9813906240525));
#27306=CARTESIAN_POINT('Ctrl Pts',(-4.79452430018796,-23.1436390432055,
11.0011703424276));
#27307=CARTESIAN_POINT('Ctrl Pts',(-4.75683130501539,-23.2710287285292,
11.0210525151785));
#27308=CARTESIAN_POINT('Ctrl Pts',(-4.71425260210546,-23.3962563395395,
11.0432098643964));
#27309=CARTESIAN_POINT('Ctrl Pts',(-4.6670950177236,-23.5189409398137,11.0672614586823));
#27310=CARTESIAN_POINT('Ctrl Pts',(-4.64452824749322,-23.5776503758775,
11.0787710983095));
#27311=CARTESIAN_POINT('Ctrl Pts',(-4.6209134211507,-23.6357780439662,11.0907145202877));
#27312=CARTESIAN_POINT('Ctrl Pts',(-4.5962867820572,-23.6932855019245,11.1030499800133));
#27313=CARTESIAN_POINT('Ctrl Pts',(-4.49601285006955,-23.927442461232,11.1532770956529));
#27314=CARTESIAN_POINT('Ctrl Pts',(-4.37796206036335,-24.1536729575001,
11.2104673133284));
#27315=CARTESIAN_POINT('Ctrl Pts',(-4.24308688402606,-24.3700356698173,
11.2718912075364));
#27316=CARTESIAN_POINT('Ctrl Pts',(-4.20675437544135,-24.4283191903001,
11.2884375003697));
#27317=CARTESIAN_POINT('Ctrl Pts',(-4.16920085776234,-24.4858864280512,
11.3052910096004));
#27318=CARTESIAN_POINT('Ctrl Pts',(-4.13044480435484,-24.5426986563822,
11.322398381924));
#27319=CARTESIAN_POINT('Ctrl Pts',(-4.07064556195374,-24.6303579486633,
11.3487944623935));
#27320=CARTESIAN_POINT('Ctrl Pts',(-4.00839642509525,-24.7156218846498,
11.3755981754695));
#27321=CARTESIAN_POINT('Ctrl Pts',(-3.94374556949127,-24.7985762367506,
11.4026504426682));
#27322=CARTESIAN_POINT('Ctrl Pts',(-3.87734852680968,-24.8837711441591,
11.4304333779912));
#27323=CARTESIAN_POINT('Ctrl Pts',(-3.80841806017054,-24.966530674899,11.4584784754038));
#27324=CARTESIAN_POINT('Ctrl Pts',(-3.73695665037637,-25.0469203773131,
11.4866134152488));
#27325=CARTESIAN_POINT('Ctrl Pts',(-3.6654952405822,-25.1273100797272,11.5147483550939));
#27326=CARTESIAN_POINT('Ctrl Pts',(-3.59150241991524,-25.2053304747119,
11.5429731373713));
#27327=CARTESIAN_POINT('Ctrl Pts',(-3.51493712463866,-25.2810113905662,
11.571115442424));
#27328=CARTESIAN_POINT('Ctrl Pts',(-3.44606366015048,-25.3490893213272,
11.596430541656));
#27329=CARTESIAN_POINT('Ctrl Pts',(-3.37490019206008,-25.4154688541623,
11.6217515149196));
#27330=CARTESIAN_POINT('Ctrl Pts',(-3.30165936568716,-25.4798695627106,
11.6468682576675));
#27331=CARTESIAN_POINT('Ctrl Pts',(-3.22851890098722,-25.5441820231714,
11.6719505830222));
#27332=CARTESIAN_POINT('Ctrl Pts',(-3.15330706396815,-25.6065207404411,
11.6968292371907));
#27333=CARTESIAN_POINT('Ctrl Pts',(-3.0762736333601,-25.666641857487,11.7212949781596));
#27334=CARTESIAN_POINT('Ctrl Pts',(-2.9992662633753,-25.7267426353922,11.7457524423004));
#27335=CARTESIAN_POINT('Ctrl Pts',(-2.92043887733222,-25.7846270223891,
11.7697972725738));
#27336=CARTESIAN_POINT('Ctrl Pts',(-2.84007419592335,-25.8400915617578,
11.793220439256));
#27337=CARTESIAN_POINT('Ctrl Pts',(-2.81520835764417,-25.8572529844374,
11.8004678601938));
#27338=CARTESIAN_POINT('Ctrl Pts',(-2.7901955634273,-25.8741830466732,11.8076557654808));
#27339=CARTESIAN_POINT('Ctrl Pts',(-2.76504474865934,-25.890876562971,11.8147779632489));
#27340=CARTESIAN_POINT('Ctrl Pts',(-2.67541351514142,-25.9503680932188,
11.8401597004694));
#27341=CARTESIAN_POINT('Ctrl Pts',(-2.58395536026546,-26.0069103550976,
11.8647470590679));
#27342=CARTESIAN_POINT('Ctrl Pts',(-2.49063957468001,-26.0605177901881,
11.8884047411879));
#27343=CARTESIAN_POINT('Ctrl Pts',(-2.39717760460386,-26.1142092043777,
11.9120994844139));
#27344=CARTESIAN_POINT('Ctrl Pts',(-2.30185161455251,-26.1649569339623,
11.9348616360976));
#27345=CARTESIAN_POINT('Ctrl Pts',(-2.20460789532439,-26.2127281588654,
11.9565552615305));
#27346=CARTESIAN_POINT('Ctrl Pts',(-2.10736417609627,-26.2604993837685,
11.9782488869635));
#27347=CARTESIAN_POINT('Ctrl Pts',(-2.00820212260246,-26.3052944118206,
11.9988739861457));
#27348=CARTESIAN_POINT('Ctrl Pts',(-1.9070539613402,-26.3470282548397,12.0182946243687));
#27349=CARTESIAN_POINT('Ctrl Pts',(-1.83958236011387,-26.3748671120042,
12.0312492993859));
#27350=CARTESIAN_POINT('Ctrl Pts',(-1.77116522528206,-26.4013624874179,
12.0436669537073));
#27351=CARTESIAN_POINT('Ctrl Pts',(-1.70211845445723,-26.4263607356803,
12.0554616259635));
#27352=CARTESIAN_POINT('Ctrl Pts',(-1.63312683696538,-26.4513390157864,
12.0672468768452));
#27353=CARTESIAN_POINT('Ctrl Pts',(-1.56350692997892,-26.4748224190479,
12.0784101405182));
#27354=CARTESIAN_POINT('Ctrl Pts',(-1.49359250753464,-26.4967063427496,
12.0888656614418));
#27355=CARTESIAN_POINT('Ctrl Pts',(-1.47621822254929,-26.5021446702605,
12.0914639407932));
#27356=CARTESIAN_POINT('Ctrl Pts',(-1.4588258251848,-26.5074844603353,12.0940185126651));
#27357=CARTESIAN_POINT('Ctrl Pts',(-1.44142057741721,-26.5127245867947,
12.0965280609763));
#27358=CARTESIAN_POINT('Ctrl Pts',(-1.33443605684673,-26.5449339770008,
12.1119534560361));
#27359=CARTESIAN_POINT('Ctrl Pts',(-1.2265643434951,-26.5735040359102,12.1257607110881));
#27360=CARTESIAN_POINT('Ctrl Pts',(-1.11780240571892,-26.5984502954035,
12.1378800488878));
#27361=CARTESIAN_POINT('Ctrl Pts',(-1.06640774795444,-26.6102384677677,
12.1436069532744));
#27362=CARTESIAN_POINT('Ctrl Pts',(-1.0148140761704,-26.6212167384201,12.1489569515008));
#27363=CARTESIAN_POINT('Ctrl Pts',(-0.963020157800805,-26.6313827995448,
12.1539226808697));
#27364=CARTESIAN_POINT('Ctrl Pts',(-0.855269211084243,-26.6525320530682,
12.1642532767675));
#27365=CARTESIAN_POINT('Ctrl Pts',(-0.746653788707331,-26.6701690181909,
12.1729212537809));
#27366=CARTESIAN_POINT('Ctrl Pts',(-0.637152302600715,-26.6842375364859,
12.1798520908436));
#27367=CARTESIAN_POINT('Ctrl Pts',(-0.5826308696635,-26.6912423343568,12.1833029953157));
#27368=CARTESIAN_POINT('Ctrl Pts',(-0.527889749065468,-26.6973616759382,
12.1863232449754));
#27369=CARTESIAN_POINT('Ctrl Pts',(-0.47292655284801,-26.7025837989542,
12.1889036412423));
#27370=CARTESIAN_POINT('Ctrl Pts',(-0.404235664745158,-26.7091102073955,
12.1921285212244));
#27371=CARTESIAN_POINT('Ctrl Pts',(-0.335041472045689,-26.7142453423437,
12.1946593254799));
#27372=CARTESIAN_POINT('Ctrl Pts',(-0.265699869767895,-26.7179353670166,
12.1964843947152));
#27373=CARTESIAN_POINT('Ctrl Pts',(-0.196380842097205,-26.7216241903782,
12.1983088697875));
#27374=CARTESIAN_POINT('Ctrl Pts',(-0.126914850849468,-26.7238688082875,
12.199428069278));
#27375=CARTESIAN_POINT('Ctrl Pts',(-0.0576609418612023,-26.7246675105234,
12.199830345277));
#27376=CARTESIAN_POINT('Ctrl Pts',(-0.0294298005914876,-26.7249930990135,
12.1999943318407));
#27377=CARTESIAN_POINT('Ctrl Pts',(-0.00123391300176287,-26.7250790148406,
12.2000391829301));
#27378=CARTESIAN_POINT('Ctrl Pts',(0.02690243843868,-26.7249276253568,12.1999641095028));
#27379=CARTESIAN_POINT('Ctrl Pts',(0.138964937173212,-26.7243246657343,
12.199665104286));
#27380=CARTESIAN_POINT('Ctrl Pts',(0.250446307094146,-26.7199615810888,
12.1975038994839));
#27381=CARTESIAN_POINT('Ctrl Pts',(0.361351533677301,-26.7119254124269,
12.1935289489303));
#27382=CARTESIAN_POINT('Ctrl Pts',(0.473050020772804,-26.7038317642803,
12.189525567153));
#27383=CARTESIAN_POINT('Ctrl Pts',(0.584164785055125,-26.69201231097,12.1836824008448));
#27384=CARTESIAN_POINT('Ctrl Pts',(0.694705554438122,-26.6765032255501,
12.1760489510065));
#27385=CARTESIAN_POINT('Ctrl Pts',(0.799969826429573,-26.6617344429996,
12.1687798724168));
#27386=CARTESIAN_POINT('Ctrl Pts',(0.904714134528312,-26.6436194134591,
12.1598873441439));
#27387=CARTESIAN_POINT('Ctrl Pts',(1.00894214499993,-26.6221456735575,12.1494141115995));
#27388=CARTESIAN_POINT('Ctrl Pts',(1.09363406960635,-26.6046968864941,12.1409039403218));
#27389=CARTESIAN_POINT('Ctrl Pts',(1.17814728800982,-26.5849902238148,12.1312966461346));
#27390=CARTESIAN_POINT('Ctrl Pts',(1.26214615412685,-26.5630767961684,12.1206897039041));
#27391=CARTESIAN_POINT('Ctrl Pts',(1.34613296222794,-26.5411665141889,12.1100842842975));
#27392=CARTESIAN_POINT('Ctrl Pts',(1.42960515522795,-26.5170501926057,12.0984795036255));
#27393=CARTESIAN_POINT('Ctrl Pts',(1.51223946396481,-26.4908296028737,12.0859727947828));
#27394=CARTESIAN_POINT('Ctrl Pts',(1.59512110193217,-26.4645305334112,12.0734286526425));
#27395=CARTESIAN_POINT('Ctrl Pts',(1.67715943435879,-26.436114726054,12.0599771752061));
#27396=CARTESIAN_POINT('Ctrl Pts',(1.75804669282504,-26.4057341118511,12.0457166728564));
#27397=CARTESIAN_POINT('Ctrl Pts',(1.82285587208338,-26.3813922969697,12.0342907515108));
#27398=CARTESIAN_POINT('Ctrl Pts',(1.88692638866243,-26.355790141741,12.0223454627404));
#27399=CARTESIAN_POINT('Ctrl Pts',(1.95011090991557,-26.3290273065033,12.00993137371));
#27400=CARTESIAN_POINT('Ctrl Pts',(2.05042011318945,-26.2865397062684,11.9902232655323));
#27401=CARTESIAN_POINT('Ctrl Pts',(2.14890000537001,-26.240965322187,11.9693088676812));
#27402=CARTESIAN_POINT('Ctrl Pts',(2.24560160523857,-26.1923564252866,11.9473166525052));
#27403=CARTESIAN_POINT('Ctrl Pts',(2.3427067484564,-26.1435446796528,11.9252326620931));
#27404=CARTESIAN_POINT('Ctrl Pts',(2.43801933205824,-26.091672772653,11.9020618399542));
#27405=CARTESIAN_POINT('Ctrl Pts',(2.53157272698267,-26.0367443718288,11.8779342735337));
#27406=CARTESIAN_POINT('Ctrl Pts',(2.62284040748174,-25.9831579921918,11.8543961964275));
#27407=CARTESIAN_POINT('Ctrl Pts',(2.71243423321569,-25.9266621694752,11.8299475546468));
#27408=CARTESIAN_POINT('Ctrl Pts',(2.8003604129185,-25.8672194000027,11.8047091317359));
#27409=CARTESIAN_POINT('Ctrl Pts',(2.860949369842,-25.8262580457035,11.7873176139452));
#27410=CARTESIAN_POINT('Ctrl Pts',(2.92085135042964,-25.7838189328308,11.7695149004781));
#27411=CARTESIAN_POINT('Ctrl Pts',(2.979771996753,-25.740091387175,11.7514368077031));
#27412=CARTESIAN_POINT('Ctrl Pts',(3.03873246635287,-25.696334286953,11.7333464963097));
#27413=CARTESIAN_POINT('Ctrl Pts',(3.09670997807265,-25.6512872316562,11.7149804332359));
#27414=CARTESIAN_POINT('Ctrl Pts',(3.15344090921893,-25.6051817524524,11.6964747104228));
#27415=CARTESIAN_POINT('Ctrl Pts',(3.16531031431661,-25.5955354343181,11.6926028910069));
#27416=CARTESIAN_POINT('Ctrl Pts',(3.17712526920413,-25.5858429232248,11.6887249580996));
#27417=CARTESIAN_POINT('Ctrl Pts',(3.18888355034015,-25.576106555572,11.6848421581069));
#27418=CARTESIAN_POINT('Ctrl Pts',(3.27071584751788,-25.5083458580709,11.6578196333676));
#27419=CARTESIAN_POINT('Ctrl Pts',(3.35003194509616,-25.4382776550022,11.630495647921));
#27420=CARTESIAN_POINT('Ctrl Pts',(3.42690620703297,-25.3659221150965,11.6030230525742));
#27421=CARTESIAN_POINT('Ctrl Pts',(3.46663172712634,-25.3285316884183,11.5888263226028));
#27422=CARTESIAN_POINT('Ctrl Pts',(3.50570473102955,-25.2905297142222,11.5745899077572));
#27423=CARTESIAN_POINT('Ctrl Pts',(3.54413226871441,-25.2519145810265,11.5603349008083));
#27424=CARTESIAN_POINT('Ctrl Pts',(3.63371231053588,-25.1618972274563,11.5271044573404));
#27425=CARTESIAN_POINT('Ctrl Pts',(3.71989006886463,-25.0684457181042,11.4937239948699));
#27426=CARTESIAN_POINT('Ctrl Pts',(3.80256443311774,-24.9716141951251,11.4605294433205));
#27427=CARTESIAN_POINT('Ctrl Pts',(3.88413333468549,-24.8760774342695,11.4277787456602));
#27428=CARTESIAN_POINT('Ctrl Pts',(3.96229233349035,-24.7772497347628,11.3952090204235));
#27429=CARTESIAN_POINT('Ctrl Pts',(4.03690038853381,-24.6751585132083,11.3631429014686));
#27430=CARTESIAN_POINT('Ctrl Pts',(4.07709703146054,-24.6201547421492,11.3458666122942));
#27431=CARTESIAN_POINT('Ctrl Pts',(4.11626213049796,-24.5642032928262,11.3287365069273));
#27432=CARTESIAN_POINT('Ctrl Pts',(4.1543676039913,-24.5073065630709,11.3118030424508));
#27433=CARTESIAN_POINT('Ctrl Pts',(4.21421033911305,-24.4179531023762,11.2852098857081));
#27434=CARTESIAN_POINT('Ctrl Pts',(4.27098639377895,-24.3269514107848,11.2593090022837));
#27435=CARTESIAN_POINT('Ctrl Pts',(4.32474835890819,-24.2342930542527,11.2342641385601));
#27436=CARTESIAN_POINT('Ctrl Pts',(4.37895464840352,-24.140868907902,11.2090122875516));
#27437=CARTESIAN_POINT('Ctrl Pts',(4.43009721669823,-24.0457600597992,11.1846306641376));
#27438=CARTESIAN_POINT('Ctrl Pts',(4.47818472846866,-23.948929301419,11.1612871082715));
#27439=CARTESIAN_POINT('Ctrl Pts',(4.52627224023909,-23.8520985430388,11.1379435524055));
#27440=CARTESIAN_POINT('Ctrl Pts',(4.57130500244527,-23.7535452679376,11.1156380640875));
#27441=CARTESIAN_POINT('Ctrl Pts',(4.61324143793115,-23.6532124974584,11.0945384832709));
#27442=CARTESIAN_POINT('Ctrl Pts',(4.64779437854339,-23.5705447118047,11.077153778194));
#27443=CARTESIAN_POINT('Ctrl Pts',(4.68032091015781,-23.4864689291325,11.0605827600001));
#27444=CARTESIAN_POINT('Ctrl Pts',(4.71063625737614,-23.401277438461,11.0449609415872));
#27445=CARTESIAN_POINT('Ctrl Pts',(4.74089320150449,-23.316250070808,11.0293692189031));
#27446=CARTESIAN_POINT('Ctrl Pts',(4.76894726681297,-23.2301116686913,11.0147230422201));
#27447=CARTESIAN_POINT('Ctrl Pts',(4.79466151550492,-23.1431752189825,11.0011571427398));
#27448=CARTESIAN_POINT('Ctrl Pts',(4.82036529714633,-23.0562741569773,10.9875967652935));
#27449=CARTESIAN_POINT('Ctrl Pts',(4.84373102103341,-22.9685761046264,10.9751157857696));
#27450=CARTESIAN_POINT('Ctrl Pts',(4.86467135302676,-22.8804101553305,10.9638487709085));
#27451=CARTESIAN_POINT('Ctrl Pts',(4.87800732471196,-22.8242611599954,10.9566733072523));
#27452=CARTESIAN_POINT('Ctrl Pts',(4.8903605993491,-22.7679227065184,10.9499902098156));
#27453=CARTESIAN_POINT('Ctrl Pts',(4.90171939734693,-22.7114821081362,10.9438342370992));
#27454=CARTESIAN_POINT('Ctrl Pts',(4.92224489379668,-22.6094932091403,10.9327103139376));
#27455=CARTESIAN_POINT('Ctrl Pts',(4.9395767042353,-22.5069383142082,10.9232291557851));
#27456=CARTESIAN_POINT('Ctrl Pts',(4.95371419021583,-22.4037604302362,10.9154640387934));
#27457=CARTESIAN_POINT('Ctrl Pts',(4.9677954134181,-22.300993162014,10.9077298245419));
#27458=CARTESIAN_POINT('Ctrl Pts',(4.97870774356615,-22.197607242805,10.9016980200141));
#27459=CARTESIAN_POINT('Ctrl Pts',(4.98639906423008,-22.093543582559,10.8974410299904));
#27460=CARTESIAN_POINT('Ctrl Pts',(4.99400877478537,-21.9905841080553,10.893229209507));
#27461=CARTESIAN_POINT('Ctrl Pts',(4.99846543872905,-21.8869606057259,10.8907547393857));
#27462=CARTESIAN_POINT('Ctrl Pts',(4.99966795889425,-21.7826220513888,10.8900877439848));
#27463=CARTESIAN_POINT('Ctrl Pts',(4.99988904773768,-21.7634389299979,10.8899651138235));
#27464=CARTESIAN_POINT('Ctrl Pts',(5.,-21.7442316692363,10.8899035808404));
#27465=CARTESIAN_POINT('Ctrl Pts',(5.,-21.725,10.8899035808404));
#27466=CARTESIAN_POINT('',(-5.7251211610453,-21.780229807,11.3363568967879));
#27467=CARTESIAN_POINT('Origin',(-5.49972269013801,-21.7802298069994,10.8900436331349));
#27468=CARTESIAN_POINT('',(5.90594023139769E-11,-27.2249981621,12.6999990362978));
#27469=CARTESIAN_POINT('Ctrl Pts',(1.18064065468548E-10,-27.2249963242,
12.6999980725955));
#27470=CARTESIAN_POINT('Ctrl Pts',(-0.171632395971071,-27.2249764687244,
12.6999876622625));
#27471=CARTESIAN_POINT('Ctrl Pts',(-0.34497573023189,-27.2174810037563,
12.6964657742887));
#27472=CARTESIAN_POINT('Ctrl Pts',(-0.515865020136667,-27.202628290705,
12.6895186386625));
#27473=CARTESIAN_POINT('Ctrl Pts',(-0.529884766594002,-27.2014097750724,
12.6889486960983));
#27474=CARTESIAN_POINT('Ctrl Pts',(-0.543892550080955,-27.2001423452679,
12.6883559858665));
#27475=CARTESIAN_POINT('Ctrl Pts',(-0.557888332060774,-27.1988261027941,
12.6877406113709));
#27476=CARTESIAN_POINT('Ctrl Pts',(-0.733011862938552,-27.1823564957489,
12.6800406804463));
#27477=CARTESIAN_POINT('Ctrl Pts',(-0.906349061560203,-27.1582411107519,
12.6687880610839));
#27478=CARTESIAN_POINT('Ctrl Pts',(-1.07794709135125,-27.1266398382469,
12.6541704614814));
#27479=CARTESIAN_POINT('Ctrl Pts',(-1.08722589090208,-27.1249310664534,
12.6533800457826));
#27480=CARTESIAN_POINT('Ctrl Pts',(-1.09649960414915,-27.1232004052766,
12.6525797890944));
#27481=CARTESIAN_POINT('Ctrl Pts',(-1.10576823104768,-27.1214478465577,
12.6517697177991));
#27482=CARTESIAN_POINT('Ctrl Pts',(-1.28133872673209,-27.0882500917697,
12.6364249833093));
#27483=CARTESIAN_POINT('Ctrl Pts',(-1.45513158176923,-27.0471835338455,
12.6175524377448));
#27484=CARTESIAN_POINT('Ctrl Pts',(-1.62701656816808,-26.998245868259,12.5953490259975));
#27485=CARTESIAN_POINT('Ctrl Pts',(-1.63201737474387,-26.9968220801493,
12.594703041902));
#27486=CARTESIAN_POINT('Ctrl Pts',(-1.63701731244541,-26.9953913121635,
12.5940540985787));
#27487=CARTESIAN_POINT('Ctrl Pts',(-1.64201629264252,-26.9939535946684,
12.5934022164756));
#27488=CARTESIAN_POINT('Ctrl Pts',(-1.81762883641368,-26.9434470480164,
12.5705018108212));
#27489=CARTESIAN_POINT('Ctrl Pts',(-1.99221998730359,-26.8843104198491,
12.5439539328558));
#27490=CARTESIAN_POINT('Ctrl Pts',(-2.16210038387339,-26.8177548520731,
12.5146043457249));
#27491=CARTESIAN_POINT('Ctrl Pts',(-2.16326958009573,-26.8172967855746,
12.5144023481602));
#27492=CARTESIAN_POINT('Ctrl Pts',(-2.16443856124667,-26.8168383746705,
12.5142002198446));
#27493=CARTESIAN_POINT('Ctrl Pts',(-2.16560732738127,-26.8163796193749,
12.5139979609133));
#27494=CARTESIAN_POINT('Ctrl Pts',(-2.42817585265368,-26.7133181959941,
12.4685595898275));
#27495=CARTESIAN_POINT('Ctrl Pts',(-2.67998559716822,-26.5928358458073,
12.4165088834739));
#27496=CARTESIAN_POINT('Ctrl Pts',(-2.92148617968103,-26.4551266226912,
12.3594132760708));
#27497=CARTESIAN_POINT('Ctrl Pts',(-2.99451972446863,-26.4134812046575,
12.3421466734106));
#27498=CARTESIAN_POINT('Ctrl Pts',(-3.06661060146402,-26.3702603926359,
12.3244190004151));
#27499=CARTESIAN_POINT('Ctrl Pts',(-3.13777165534967,-26.3254697896135,
12.3062744139855));
#27500=CARTESIAN_POINT('Ctrl Pts',(-3.14194877443755,-26.3228406031045,
12.305209335629));
#27501=CARTESIAN_POINT('Ctrl Pts',(-3.14612271412673,-26.3202059886339,
12.3041428146321));
#27502=CARTESIAN_POINT('Ctrl Pts',(-3.15029347649961,-26.3175659473305,
12.3030748600242));
#27503=CARTESIAN_POINT('Ctrl Pts',(-3.31324758257754,-26.2144180016697,
12.2613492537928));
#27504=CARTESIAN_POINT('Ctrl Pts',(-3.47148910296816,-26.1025701354325,
12.2173084213314));
#27505=CARTESIAN_POINT('Ctrl Pts',(-3.62330617417467,-25.9833742848673,
12.1721206971488));
#27506=CARTESIAN_POINT('Ctrl Pts',(-3.75269317403453,-25.8817889138823,
12.1336091910579));
#27507=CARTESIAN_POINT('Ctrl Pts',(-3.87741323405155,-25.774867164968,12.0942651966009));
#27508=CARTESIAN_POINT('Ctrl Pts',(-3.99639186226798,-25.6634672539009,
12.0548265200017));
#27509=CARTESIAN_POINT('Ctrl Pts',(-4.00274578696789,-25.6575180623772,
12.0527203402185));
#27510=CARTESIAN_POINT('Ctrl Pts',(-4.00908358390065,-25.6515558925673,
12.0506138106243));
#27511=CARTESIAN_POINT('Ctrl Pts',(-4.0154050829856,-25.6455808754667,12.0485070450674));
#27512=CARTESIAN_POINT('Ctrl Pts',(-4.18308716223757,-25.4870894674118,
11.9926236502703));
#27513=CARTESIAN_POINT('Ctrl Pts',(-4.34064777629496,-25.3188565700565,
11.9362388053108));
#27514=CARTESIAN_POINT('Ctrl Pts',(-4.48780703949086,-25.1403669812823,
11.8806468112938));
#27515=CARTESIAN_POINT('Ctrl Pts',(-4.56399636137668,-25.0479568914446,
11.8518649579843));
#27516=CARTESIAN_POINT('Ctrl Pts',(-4.63739813230243,-24.9527977843453,
11.8232962958883));
#27517=CARTESIAN_POINT('Ctrl Pts',(-4.70797686641107,-24.8548201088207,
11.7951242588372));
#27518=CARTESIAN_POINT('Ctrl Pts',(-4.71381080357356,-24.8467214143689,
11.7927955985691));
#27519=CARTESIAN_POINT('Ctrl Pts',(-4.71962549432073,-24.8386033842874,
11.7904696333387));
#27520=CARTESIAN_POINT('Ctrl Pts',(-4.7254209172366,-24.8304659809309,11.7881464680579));
#27521=CARTESIAN_POINT('Ctrl Pts',(-4.849069317038,-24.6568501951343,11.7385805134052));
#27522=CARTESIAN_POINT('Ctrl Pts',(-4.96233092517715,-24.4764189499148,
11.6909386109933));
#27523=CARTESIAN_POINT('Ctrl Pts',(-5.06454613053106,-24.2901935954381,
11.6464866495965));
#27524=CARTESIAN_POINT('Ctrl Pts',(-5.13166827091823,-24.1679041146944,
11.6172961707139));
#27525=CARTESIAN_POINT('Ctrl Pts',(-5.19402747768693,-24.0431170557518,
11.5894817374231));
#27526=CARTESIAN_POINT('Ctrl Pts',(-5.25144368329969,-23.9161310885085,
11.5634052940795));
#27527=CARTESIAN_POINT('Ctrl Pts',(-5.25497935242791,-23.9083113386782,
11.5617995161511));
#27528=CARTESIAN_POINT('Ctrl Pts',(-5.2584964217271,-23.9004829362191,11.5602002646197));
#27529=CARTESIAN_POINT('Ctrl Pts',(-5.26199484288721,-23.8926459553828,
11.5586076269338));
#27530=CARTESIAN_POINT('Ctrl Pts',(-5.33218637120295,-23.7354065502039,
11.5266533057958));
#27531=CARTESIAN_POINT('Ctrl Pts',(-5.39508015392478,-23.5743103376335,
11.4972547885584));
#27532=CARTESIAN_POINT('Ctrl Pts',(-5.45035838176973,-23.4092290587574,
11.4709892437974));
#27533=CARTESIAN_POINT('Ctrl Pts',(-5.4526197177918,-23.4024758711636,11.4699147661084));
#27534=CARTESIAN_POINT('Ctrl Pts',(-5.45486833919957,-23.3957159278597,
11.4688455187614));
#27535=CARTESIAN_POINT('Ctrl Pts',(-5.4571042251612,-23.388949216604,11.4677815411574));
#27536=CARTESIAN_POINT('Ctrl Pts',(-5.50854732838719,-23.2332612112242,
11.4433016210485));
#27537=CARTESIAN_POINT('Ctrl Pts',(-5.55343224177118,-23.0730960972466,
11.4215204228469));
#27538=CARTESIAN_POINT('Ctrl Pts',(-5.59069638198729,-22.911046832253,11.4032502530102));
#27539=CARTESIAN_POINT('Ctrl Pts',(-5.59337746515253,-22.8993876995374,
11.4019357494555));
#27540=CARTESIAN_POINT('Ctrl Pts',(-5.59601909769806,-22.887718835213,11.4006394240543));
#27541=CARTESIAN_POINT('Ctrl Pts',(-5.59862088330176,-22.8760412148246,
11.3993615807472));
#27542=CARTESIAN_POINT('Ctrl Pts',(-5.59971764885756,-22.8711185909937,
11.3988229143317));
#27543=CARTESIAN_POINT('Ctrl Pts',(-5.60080729581453,-22.8661946078742,
11.3982875507515));
#27544=CARTESIAN_POINT('Ctrl Pts',(-5.60188979660494,-22.8612693368901,
11.397755511778));
#27545=CARTESIAN_POINT('Ctrl Pts',(-5.65190530306711,-22.6337037545663,
11.3731733600113));
#27546=CARTESIAN_POINT('Ctrl Pts',(-5.68664788019735,-22.4049656318907,
11.3557815554441));
#27547=CARTESIAN_POINT('Ctrl Pts',(-5.70627364103823,-22.1749701955463,
11.3458925282718));
#27548=CARTESIAN_POINT('Ctrl Pts',(-5.71746617897322,-22.043804190466,11.3402528329416));
#27549=CARTESIAN_POINT('Ctrl Pts',(-5.72374125703581,-21.9122292652076,
11.3370537800739));
#27550=CARTESIAN_POINT('Ctrl Pts',(-5.7251211610453,-21.780229807,11.3363568967879));
#27551=CARTESIAN_POINT('',(5.72518221930917,-21.6759575456936,11.3363260607529));
#27552=CARTESIAN_POINT('Ctrl Pts',(5.72518221930917,-21.6759575456936,11.3363260607529));
#27553=CARTESIAN_POINT('Ctrl Pts',(5.72869753618992,-22.054656247908,11.3345507210535));
#27554=CARTESIAN_POINT('Ctrl Pts',(5.69169600405042,-22.4271933388261,11.353483157288));
#27555=CARTESIAN_POINT('Ctrl Pts',(5.54179856043293,-23.1557233325998,11.4273991757061));
#27556=CARTESIAN_POINT('Ctrl Pts',(5.42683471955466,-23.515723594293,11.4832806925781));
#27557=CARTESIAN_POINT('Ctrl Pts',(5.13200755045586,-24.1906498178588,11.6180363676468));
#27558=CARTESIAN_POINT('Ctrl Pts',(4.95210182586657,-24.5091884261888,11.6969653793332));
#27559=CARTESIAN_POINT('Ctrl Pts',(4.52772048446401,-25.1108860436928,11.8676896990794));
#27560=CARTESIAN_POINT('Ctrl Pts',(4.28895572693526,-25.3857672051624,11.9570844402389));
#27561=CARTESIAN_POINT('Ctrl Pts',(3.89416364467019,-25.7607959445649,12.0890339520237));
#27562=CARTESIAN_POINT('Ctrl Pts',(3.75631023962589,-25.8796597515521,12.132715698208));
#27563=CARTESIAN_POINT('Ctrl Pts',(3.46769878466619,-26.105090547267,12.218335482736));
#27564=CARTESIAN_POINT('Ctrl Pts',(3.31654194508705,-26.2117959753026,12.2603439327474));
#27565=CARTESIAN_POINT('Ctrl Pts',(2.85271276315387,-26.5069617657877,12.3795785542984));
#27566=CARTESIAN_POINT('Ctrl Pts',(2.52697785378788,-26.673150598635,12.4509224724164));
#27567=CARTESIAN_POINT('Ctrl Pts',(1.84139507760884,-26.9449521303425,12.5706146093107));
#27568=CARTESIAN_POINT('Ctrl Pts',(1.47783781121532,-27.0506741288963,12.6190624489701));
#27569=CARTESIAN_POINT('Ctrl Pts',(0.746514761693329,-27.1897926257461,
12.6833535548702));
#27570=CARTESIAN_POINT('Ctrl Pts',(0.375845029736948,-27.225,12.7));
#27571=CARTESIAN_POINT('Ctrl Pts',(5.47391594054725E-14,-27.225,12.7));
#27572=CARTESIAN_POINT('',(4.99980122230293,-21.6804159506306,10.890014011117));
#27573=CARTESIAN_POINT('Origin',(5.49978134453322,-21.6759575456936,10.890014011117));
#27574=CARTESIAN_POINT('Ctrl Pts',(5.00000186381615,-21.7249999998502,10.8899037053764));
#27575=CARTESIAN_POINT('Ctrl Pts',(5.00000067893857,-21.710138258254,10.889903626456));
#27576=CARTESIAN_POINT('Ctrl Pts',(4.99993373995471,-21.6952769138386,10.8899403932703));
#27577=CARTESIAN_POINT('Ctrl Pts',(4.99980122230293,-21.6804159506306,10.890014011117));
#27578=CARTESIAN_POINT('Ctrl Pts',(0.187614356002326,-16.7285211545107,
-12.1982543436608));
#27579=CARTESIAN_POINT('Ctrl Pts',(0.196065836120502,-16.7288385017964,
-12.6985003258571));
#27580=CARTESIAN_POINT('Ctrl Pts',(0.214833815848565,-16.2288732699618,
-12.6981828003682));
#27581=CARTESIAN_POINT('Ctrl Pts',(-0.147150608123537,-16.7159509595597,
-12.2044844246647));
#27582=CARTESIAN_POINT('Ctrl Pts',(-0.153364144532674,-16.7151512337624,
-12.7038460495061));
#27583=CARTESIAN_POINT('Ctrl Pts',(-0.168499981233245,-16.2150460406695,
-12.7046682214451));
#27584=CARTESIAN_POINT('Ctrl Pts',(-0.477103276237398,-16.736913068974,
-12.1939867058945));
#27585=CARTESIAN_POINT('Ctrl Pts',(-0.500337628562375,-16.7382895625106,
-12.6946996408902));
#27586=CARTESIAN_POINT('Ctrl Pts',(-0.546322358158132,-16.2381043757634,
-12.6937402597205));
#27587=CARTESIAN_POINT('Ctrl Pts',(-1.1277665069231,-16.8427073547839,-12.1420671135872));
#27588=CARTESIAN_POINT('Ctrl Pts',(-1.17908021929114,-16.8534749528196,
-12.6502386327239));
#27589=CARTESIAN_POINT('Ctrl Pts',(-1.29138509026417,-16.3544780903702,
-12.639692814658));
#27590=CARTESIAN_POINT('Ctrl Pts',(-1.45180549185659,-16.9291924465061,
-12.0998581413745));
#27591=CARTESIAN_POINT('Ctrl Pts',(-1.51789645660857,-16.9485764266167,
-12.6138005825543));
#27592=CARTESIAN_POINT('Ctrl Pts',(-1.6624362885213,-16.4496116918588,-12.5957539678988));
#27593=CARTESIAN_POINT('Ctrl Pts',(-2.06567044084562,-17.1598587200229,
-11.9914081040113));
#27594=CARTESIAN_POINT('Ctrl Pts',(-2.15329340789673,-17.1983479333955,
-12.5221940651536));
#27595=CARTESIAN_POINT('Ctrl Pts',(-2.36536197212213,-16.7033445913232,
-12.4828592547569));
#27596=CARTESIAN_POINT('Ctrl Pts',(-2.35751884362729,-17.3036147067357,
-11.9253357164031));
#27597=CARTESIAN_POINT('Ctrl Pts',(-2.4544528650964,-17.3549880636414,-12.4663842122447));
#27598=CARTESIAN_POINT('Ctrl Pts',(-2.69955231567642,-16.8614761770065,
-12.4140789843431));
#27599=CARTESIAN_POINT('Ctrl Pts',(-2.91233266304311,-17.6476403801818,
-11.7760710934922));
#27600=CARTESIAN_POINT('Ctrl Pts',(-3.02007704204278,-17.7234499869819,
-12.3435601844791));
#27601=CARTESIAN_POINT('Ctrl Pts',(-3.33485961450271,-17.2399044186028,
-12.2586969571052));
#27602=CARTESIAN_POINT('Ctrl Pts',(-3.17086067768701,-17.8456812804081,
-11.6939431718919));
#27603=CARTESIAN_POINT('Ctrl Pts',(-3.28059025491442,-17.9355317918585,
-12.2768183621404));
#27604=CARTESIAN_POINT('Ctrl Pts',(-3.63089538292129,-17.4577494084836,
-12.1732031391639));
#27605=CARTESIAN_POINT('Ctrl Pts',(-3.52407060676517,-18.1743952416661,
-11.5685539618248));
#27606=CARTESIAN_POINT('Ctrl Pts',(-3.62848602121164,-18.2778735858662,
-12.1788301241707));
#27607=CARTESIAN_POINT('Ctrl Pts',(-4.0353497028142,-17.8193347658154,-12.0426750252286));
#27608=CARTESIAN_POINT('Ctrl Pts',(-3.63648642665548,-18.2895856083501,
-11.5262563077414));
#27609=CARTESIAN_POINT('Ctrl Pts',(-3.7392140074201,-18.398386108395,-12.1459008906374));
#27610=CARTESIAN_POINT('Ctrl Pts',(-4.16407503160209,-17.946044168994,-11.998643861893));
#27611=CARTESIAN_POINT('Ctrl Pts',(-3.85069511498075,-18.5315296768142,
-11.4417639857172));
#27612=CARTESIAN_POINT('Ctrl Pts',(-3.94847315831418,-18.6493371688439,
-12.0811442331505));
#27613=CARTESIAN_POINT('Ctrl Pts',(-4.40936153697645,-18.2121826446868,
-11.9106887386745));
#27614=CARTESIAN_POINT('Ctrl Pts',(-3.95295516857438,-18.65898775844,-11.3993577635689));
#27615=CARTESIAN_POINT('Ctrl Pts',(-4.04721398913553,-18.7806881323527,
-12.0491838773451));
#27616=CARTESIAN_POINT('Ctrl Pts',(-4.52645768074693,-18.3523865344591,
-11.866544557826));
#27617=CARTESIAN_POINT('Ctrl Pts',(-4.23843895754273,-19.052776632876,-11.2762442535035));
#27618=CARTESIAN_POINT('Ctrl Pts',(-4.32309558726455,-19.1866873378205,
-11.9570751357176));
#27619=CARTESIAN_POINT('Ctrl Pts',(-4.85336001939467,-18.7855542958133,
-11.7383854100975));
#27620=CARTESIAN_POINT('Ctrl Pts',(-4.40155791261274,-19.330923757405,-11.1993211789935));
#27621=CARTESIAN_POINT('Ctrl Pts',(-4.47343443863781,-19.4655205022704,
-11.9028712224275));
#27622=CARTESIAN_POINT('Ctrl Pts',(-5.04014459444579,-19.0915161328719,
-11.6583097529126));
#27623=CARTESIAN_POINT('Ctrl Pts',(-4.67409657173356,-19.9199697089661,
-11.0648949485446));
#27624=CARTESIAN_POINT('Ctrl Pts',(-4.72137264525855,-20.0436505033221,
-11.8111411860372));
#27625=CARTESIAN_POINT('Ctrl Pts',(-5.35222369623599,-19.7394666801363,
-11.5183742487049));
#27626=CARTESIAN_POINT('Ctrl Pts',(-4.78415488912749,-20.2350602306099,
-11.0070077703532));
#27627=CARTESIAN_POINT('Ctrl Pts',(-4.81645131220685,-20.3443906592467,
-11.7743644929088));
#27628=CARTESIAN_POINT('Ctrl Pts',(-5.47824949189502,-20.0860662537499,
-11.4581146468883));
#27629=CARTESIAN_POINT('Ctrl Pts',(-4.9380429612508,-20.8742413782898,-10.92446348534));
#27630=CARTESIAN_POINT('Ctrl Pts',(-4.94915052970332,-20.945781637773,-11.7227342826741));
#27631=CARTESIAN_POINT('Ctrl Pts',(-5.65446394825126,-20.7891655160397,
-11.3721873979728));
#27632=CARTESIAN_POINT('Ctrl Pts',(-4.98336003428014,-21.1995722326102,
-10.8991403351018));
#27633=CARTESIAN_POINT('Ctrl Pts',(-4.98610318476649,-21.2430778372018,
-11.7080708691409));
#27634=CARTESIAN_POINT('Ctrl Pts',(-5.70635571235477,-21.1470294558371,
-11.3458264145314));
#27635=CARTESIAN_POINT('Ctrl Pts',(-5.00266731696081,-21.6965815497726,
-10.8884241164298));
#27636=CARTESIAN_POINT('Ctrl Pts',(-5.00223861227093,-21.6991431073381,
-11.701699163389));
#27637=CARTESIAN_POINT('Ctrl Pts',(-5.72846413213322,-21.6937397047669,
-11.3346710063863));
#27638=CARTESIAN_POINT('Ctrl Pts',(-5.00081507698038,-21.8648821580315,
-10.8894579454085));
#27639=CARTESIAN_POINT('Ctrl Pts',(-5.00070606285703,-21.8530375538916,
-11.7023056251899));
#27640=CARTESIAN_POINT('Ctrl Pts',(-5.72634316547121,-21.8788703738055,
-11.3357472053704));
#27641=CARTESIAN_POINT('Ctrl Pts',(-4.98043297347855,-22.1972349510333,
-10.9007548048105));
#27642=CARTESIAN_POINT('Ctrl Pts',(-4.98363102603109,-22.1586640753178,
-11.7090448681742));
#27643=CARTESIAN_POINT('Ctrl Pts',(-5.70300398739036,-22.2444584461659,
-11.3475070510051));
#27644=CARTESIAN_POINT('Ctrl Pts',(-4.96204457374108,-22.3615907720529,
-10.9109377917453));
#27645=CARTESIAN_POINT('Ctrl Pts',(-4.96829032931648,-22.3098890090207,
-11.7150991169685));
#27646=CARTESIAN_POINT('Ctrl Pts',(-5.6819477616063,-22.4252498492313,-11.358107373132));
#27647=CARTESIAN_POINT('Ctrl Pts',(-4.9093856138036,-22.6868040641598,-10.939723249135));
#27648=CARTESIAN_POINT('Ctrl Pts',(-4.92360447493945,-22.6120103473265,
-11.7326382945398));
#27649=CARTESIAN_POINT('Ctrl Pts',(-5.62164893675429,-22.7829844706028,
-11.3880725628663));
#27650=CARTESIAN_POINT('Ctrl Pts',(-4.87511405974385,-22.8476613354423,
-10.9583260040355));
#27651=CARTESIAN_POINT('Ctrl Pts',(-4.89447456049345,-22.762190236406,-11.7440423570031));
#27652=CARTESIAN_POINT('Ctrl Pts',(-5.58240519787203,-22.9599274690212,
-11.4074377251331));
#27653=CARTESIAN_POINT('Ctrl Pts',(-4.79070121415266,-23.1659328389365,
-11.0032799996246));
#27654=CARTESIAN_POINT('Ctrl Pts',(-4.82128305228624,-23.0629430253274,
-11.7724161026754));
#27655=CARTESIAN_POINT('Ctrl Pts',(-5.48574557067997,-23.3100261227954,
-11.4542340983491));
#27656=CARTESIAN_POINT('Ctrl Pts',(-4.7402188334464,-23.3241960981967,-11.0298051346839));
#27657=CARTESIAN_POINT('Ctrl Pts',(-4.77724221450061,-23.2137337054447,
-11.7893815268673));
#27658=CARTESIAN_POINT('Ctrl Pts',(-5.42793910607718,-23.4841157078226,
-11.4818463282827));
#27659=CARTESIAN_POINT('Ctrl Pts',(-4.56702528419482,-23.786720410559,-11.118533581845));
#27660=CARTESIAN_POINT('Ctrl Pts',(-4.62424876201954,-23.6565280040077,
-11.8473998555161));
#27661=CARTESIAN_POINT('Ctrl Pts',(-5.22961829823042,-23.9928924520025,
-11.5742111885494));
#27662=CARTESIAN_POINT('Ctrl Pts',(-4.42359387417642,-24.0780740234331,
-11.1894473143436));
#27663=CARTESIAN_POINT('Ctrl Pts',(-4.49512814194823,-23.9435243529638,
-11.8955241760204));
#27664=CARTESIAN_POINT('Ctrl Pts',(-5.06537757524903,-24.3133814258724,
-11.6480312194488));
#27665=CARTESIAN_POINT('Ctrl Pts',(-4.0826233928351,-24.6297076196551,-11.3451830142359));
#27666=CARTESIAN_POINT('Ctrl Pts',(-4.17463759955658,-24.4989465486276,
-12.007578812027));
#27667=CARTESIAN_POINT('Ctrl Pts',(-4.67493842640269,-24.9201783815246,
-11.8101495324332));
#27668=CARTESIAN_POINT('Ctrl Pts',(-3.88372647707385,-24.8904795903893,
-11.4304106025715));
#27669=CARTESIAN_POINT('Ctrl Pts',(-3.984687402115,-24.7673934661874,-12.0711004171962));
#27670=CARTESIAN_POINT('Ctrl Pts',(-4.44718515387294,-25.2070275492461,
-11.8988700523303));
#27671=CARTESIAN_POINT('Ctrl Pts',(-3.44582145714119,-25.3622938940098,
-11.5990498723692));
#27672=CARTESIAN_POINT('Ctrl Pts',(-3.55485430361312,-25.2585891943117,
-12.2013450525302));
#27673=CARTESIAN_POINT('Ctrl Pts',(-3.94574801342084,-25.7260232835929,
-12.074420769944));
#27674=CARTESIAN_POINT('Ctrl Pts',(-3.20535762385381,-25.5762156720902,
-11.6832544101698));
#27675=CARTESIAN_POINT('Ctrl Pts',(-3.31545222283543,-25.4856903005333,
-12.2684573033505));
#27676=CARTESIAN_POINT('Ctrl Pts',(-3.67039721375693,-25.9613372401021,
-12.1620763107896));
#27677=CARTESIAN_POINT('Ctrl Pts',(-2.67839739753851,-25.9596625639606,
-11.8427211591104));
#27678=CARTESIAN_POINT('Ctrl Pts',(-2.78262411189189,-25.8938959406292,
-12.3978587657656));
#27679=CARTESIAN_POINT('Ctrl Pts',(-3.06698456073902,-26.3831288195538,
-12.3280785851005));
#27680=CARTESIAN_POINT('Ctrl Pts',(-2.39696430629599,-26.1249947589536,
-11.9162456328691));
#27681=CARTESIAN_POINT('Ctrl Pts',(-2.4943047005054,-26.0731137579165,-12.4592173527027));
#27682=CARTESIAN_POINT('Ctrl Pts',(-2.74472060313364,-26.5649942351177,
-12.4046163545475));
#27683=CARTESIAN_POINT('Ctrl Pts',(-1.95514407670351,-26.3297540195379,
-12.010074542758));
#27684=CARTESIAN_POINT('Ctrl Pts',(-2.03642325226439,-26.2954089354032,
-12.5382912282518));
#27685=CARTESIAN_POINT('Ctrl Pts',(-2.23880022556642,-26.7902294213573,
-12.5022907130333));
#27686=CARTESIAN_POINT('Ctrl Pts',(-1.8041850263858,-26.3910270775503,-12.038729313121));
#27687=CARTESIAN_POINT('Ctrl Pts',(-1.88026792843652,-26.3618640243966,
-12.5625025239243));
#27688=CARTESIAN_POINT('Ctrl Pts',(-2.06593973930607,-26.8576297857395,
-12.5321198581943));
#27689=CARTESIAN_POINT('Ctrl Pts',(-1.49456627687956,-26.4992186734461,
-12.0899480274511));
#27690=CARTESIAN_POINT('Ctrl Pts',(-1.55940548436926,-26.4791137879929,
-12.6058593233335));
#27691=CARTESIAN_POINT('Ctrl Pts',(-1.71140089238387,-26.9766405403565,
-12.5854377012537));
#27692=CARTESIAN_POINT('Ctrl Pts',(-1.33496957447932,-26.5463513373705,
-12.1126168837253));
#27693=CARTESIAN_POINT('Ctrl Pts',(-1.3934130031268,-26.53043167763,-12.6251936475194));
#27694=CARTESIAN_POINT('Ctrl Pts',(-1.5286495864113,-27.0284864707345,-12.6090356083803));
#27695=CARTESIAN_POINT('Ctrl Pts',(-0.850736429631688,-26.6632727202837,
-12.1692968738296));
#27696=CARTESIAN_POINT('Ctrl Pts',(-0.891162980629814,-26.6570899117739,
-12.6733724473115));
#27697=CARTESIAN_POINT('Ctrl Pts',(-0.974162944628781,-27.1570999930582,
-12.6680385491623));
#27698=CARTESIAN_POINT('Ctrl Pts',(-0.524308161271277,-26.7083885177163,
-12.1917667337562));
#27699=CARTESIAN_POINT('Ctrl Pts',(-0.548298037730936,-26.7068758397837,
-12.6929211630165));
#27700=CARTESIAN_POINT('Ctrl Pts',(-0.600375360890449,-27.2067273858123,
-12.691429313444));
#27701=CARTESIAN_POINT('Ctrl Pts',(-0.194315056429422,-26.7212227391145,
-12.19812741396));
#27702=CARTESIAN_POINT('Ctrl Pts',(-0.203067890451753,-26.7208823204571,
-12.6983912923617));
#27703=CARTESIAN_POINT('Ctrl Pts',(-0.22250666707533,-27.220845013026,-12.6980506686305));
#27704=CARTESIAN_POINT('',(-0.194315056429421,-26.7212227391145,-12.19812741396));
#27705=CARTESIAN_POINT('',(-4.99997666922215,-21.7249999973104,-10.8899189904778));
#27706=CARTESIAN_POINT('Ctrl Pts',(-0.194315056429422,-26.7212227391145,
-12.19812741396));
#27707=CARTESIAN_POINT('Ctrl Pts',(-0.517160507287741,-26.7086665070814,
-12.1919045066935));
#27708=CARTESIAN_POINT('Ctrl Pts',(-0.836463039682296,-26.6652181206119,
-12.1702661146494));
#27709=CARTESIAN_POINT('Ctrl Pts',(-1.15221063656178,-26.5904306273565,
-12.1339863259509));
#27710=CARTESIAN_POINT('Ctrl Pts',(-1.15932821021372,-26.5887447697388,
-12.1331685079511));
#27711=CARTESIAN_POINT('Ctrl Pts',(-1.16644419664539,-26.5870429349294,
-12.1323432328462));
#27712=CARTESIAN_POINT('Ctrl Pts',(-1.17355855615956,-26.5853251244403,
-12.1315105117548));
#27713=CARTESIAN_POINT('Ctrl Pts',(-1.28870992706902,-26.5575210427949,
-12.1180322815532));
#27714=CARTESIAN_POINT('Ctrl Pts',(-1.40296893847855,-26.5255529604411,
-12.1026290557827));
#27715=CARTESIAN_POINT('Ctrl Pts',(-1.51509695636072,-26.4899107581404,
-12.0856261426525));
#27716=CARTESIAN_POINT('Ctrl Pts',(-1.54970069744001,-26.4789112455903,
-12.080378886751));
#27717=CARTESIAN_POINT('Ctrl Pts',(-1.58410165154691,-26.4675621170884,
-12.0749794082388));
#27718=CARTESIAN_POINT('Ctrl Pts',(-1.61826401078079,-26.4558785310263,
-12.0694375775779));
#27719=CARTESIAN_POINT('Ctrl Pts',(-1.62865497627132,-26.4523248028207,
-12.0677519512791));
#27720=CARTESIAN_POINT('Ctrl Pts',(-1.6390259358195,-26.4487394280122,-12.0660528643397));
#27721=CARTESIAN_POINT('Ctrl Pts',(-1.64937590712078,-26.4451227862257,
-12.0643405765949));
#27722=CARTESIAN_POINT('Ctrl Pts',(-1.77283478811392,-26.4019819373357,
-12.0439156765873));
#27723=CARTESIAN_POINT('Ctrl Pts',(-1.89390130238185,-26.3542523700039,
-12.0215442646662));
#27724=CARTESIAN_POINT('Ctrl Pts',(-2.01251390952204,-26.3020956687674,
-11.9974687191318));
#27725=CARTESIAN_POINT('Ctrl Pts',(-2.02912714643473,-26.2947904450216,
-11.9940966261359));
#27726=CARTESIAN_POINT('Ctrl Pts',(-2.045692280223,-26.2873984411356,-11.9906911291611));
#27727=CARTESIAN_POINT('Ctrl Pts',(-2.0622091772275,-26.2799201687114,-11.9872529194329));
#27728=CARTESIAN_POINT('Ctrl Pts',(-2.0756450403253,-26.2738368805203,-11.9844560675063));
#27729=CARTESIAN_POINT('Ctrl Pts',(-2.08904768019195,-26.2676970992911,
-11.9816378653946));
#27730=CARTESIAN_POINT('Ctrl Pts',(-2.1024175425648,-26.261500906725,-11.9787985918042));
#27731=CARTESIAN_POINT('Ctrl Pts',(-2.21132292398046,-26.2110292791262,
-11.9556710408476));
#27732=CARTESIAN_POINT('Ctrl Pts',(-2.31827772862944,-26.1566946235418,
-11.931080510528));
#27733=CARTESIAN_POINT('Ctrl Pts',(-2.42319901808342,-26.0985597639666,
-11.9052366875763));
#27734=CARTESIAN_POINT('Ctrl Pts',(-2.52888872249225,-26.0399991405094,
-11.8792035915023));
#27735=CARTESIAN_POINT('Ctrl Pts',(-2.63251551612309,-25.9775822592216,
-11.8518983286854));
#27736=CARTESIAN_POINT('Ctrl Pts',(-2.7339708470621,-25.9113288079885,-11.8235203387557));
#27737=CARTESIAN_POINT('Ctrl Pts',(-2.78507559609586,-25.8779558352078,
-11.809225870047));
#27738=CARTESIAN_POINT('Ctrl Pts',(-2.83562895803816,-25.8436087250795,
-11.7946590258624));
#27739=CARTESIAN_POINT('Ctrl Pts',(-2.88561417754537,-25.8082859864259,
-11.779844436313));
#27740=CARTESIAN_POINT('Ctrl Pts',(-2.90446611947081,-25.7949640039616,
-11.7742571090072));
#27741=CARTESIAN_POINT('Ctrl Pts',(-2.92322108539097,-25.78151462425,-11.7686394723173));
#27742=CARTESIAN_POINT('Ctrl Pts',(-2.94187845550005,-25.767938430567,-11.7629930373066));
#27743=CARTESIAN_POINT('Ctrl Pts',(-3.0425574043087,-25.6946785391229,-11.7325237301066));
#27744=CARTESIAN_POINT('Ctrl Pts',(-3.1396582516418,-25.6183409709246,-11.7014704274661));
#27745=CARTESIAN_POINT('Ctrl Pts',(-3.2334263268648,-25.5388634611819,-11.670037162782));
#27746=CARTESIAN_POINT('Ctrl Pts',(-3.32861176523931,-25.4581845991302,
-11.6381287646264));
#27747=CARTESIAN_POINT('Ctrl Pts',(-3.42036283885039,-25.3742702133662,
-11.6058283875819));
#27748=CARTESIAN_POINT('Ctrl Pts',(-3.50889796434986,-25.2870183297407,
-11.5733422163248));
#27749=CARTESIAN_POINT('Ctrl Pts',(-3.53974158547149,-25.256621760859,-11.5620247742102));
#27750=CARTESIAN_POINT('Ctrl Pts',(-3.57019456758852,-25.2258198031469,
-11.5506847507283));
#27751=CARTESIAN_POINT('Ctrl Pts',(-3.60026510628155,-25.1946070957922,
-11.539330816509));
#27752=CARTESIAN_POINT('Ctrl Pts',(-3.62197219419989,-25.1720755079936,
-11.5311347262815));
#27753=CARTESIAN_POINT('Ctrl Pts',(-3.6434747277823,-25.1493352947599,-11.5229334023544));
#27754=CARTESIAN_POINT('Ctrl Pts',(-3.66477406772298,-25.1263866337935,
-11.5147308584899));
#27755=CARTESIAN_POINT('Ctrl Pts',(-3.85657011471908,-24.9197388001296,
-11.4408686875071));
#27756=CARTESIAN_POINT('Ctrl Pts',(-4.03300769662632,-24.6939781027987,
-11.3662983799433));
#27757=CARTESIAN_POINT('Ctrl Pts',(-4.18844906630108,-24.4556967542556,
-11.2965847525213));
#27758=CARTESIAN_POINT('Ctrl Pts',(-4.21042496844413,-24.4220091483818,
-11.2867288186893));
#27759=CARTESIAN_POINT('Ctrl Pts',(-4.23198378752848,-24.3880673310623,
-11.2769688262287));
#27760=CARTESIAN_POINT('Ctrl Pts',(-4.2531092519528,-24.3538898210574,-11.2673205519542));
#27761=CARTESIAN_POINT('Ctrl Pts',(-4.39800384639207,-24.1194743141768,
-11.2011453067637));
#27762=CARTESIAN_POINT('Ctrl Pts',(-4.52349271816479,-23.8736165952387,
-11.1399302880314));
#27763=CARTESIAN_POINT('Ctrl Pts',(-4.62889730420505,-23.6153672379701,
-11.0866584152499));
#27764=CARTESIAN_POINT('Ctrl Pts',(-4.6473789897824,-23.5700856842835,-11.0773177021002));
#27765=CARTESIAN_POINT('Ctrl Pts',(-4.66524387253178,-23.5244214900292,
-11.068221540643));
#27766=CARTESIAN_POINT('Ctrl Pts',(-4.68248793936805,-23.4783700972512,
-11.0593863294591));
#27767=CARTESIAN_POINT('Ctrl Pts',(-4.74018839941497,-23.3242772968511,
-11.0298227842256));
#27768=CARTESIAN_POINT('Ctrl Pts',(-4.79068137810927,-23.1660076341135,
-11.0032913774002));
#27769=CARTESIAN_POINT('Ctrl Pts',(-4.83290764702189,-23.006797049208,-10.980803318434));
#27770=CARTESIAN_POINT('Ctrl Pts',(-4.86052680718277,-22.902661335657,-10.966094434171));
#27771=CARTESIAN_POINT('Ctrl Pts',(-4.8847554208306,-22.7977602493764,-10.9530409731728));
#27772=CARTESIAN_POINT('Ctrl Pts',(-4.90558490800675,-22.6920927561039,
-10.9417401310877));
#27773=CARTESIAN_POINT('Ctrl Pts',(-4.91657436602273,-22.6363434968373,
-10.9357779041453));
#27774=CARTESIAN_POINT('Ctrl Pts',(-4.92661811613177,-22.5803788932101,
-10.9303032859972));
#27775=CARTESIAN_POINT('Ctrl Pts',(-4.93571509377234,-22.5241974181064,
-10.9253305204401));
#27776=CARTESIAN_POINT('Ctrl Pts',(-4.94895331108583,-22.4424403108779,
-10.9180939904964));
#27777=CARTESIAN_POINT('Ctrl Pts',(-4.96018681042669,-22.3602239878914,
-10.9119201550834));
#27778=CARTESIAN_POINT('Ctrl Pts',(-4.96938050763009,-22.2775381706359,
-10.906851659997));
#27779=CARTESIAN_POINT('Ctrl Pts',(-4.97359143004183,-22.2396661858064,
-10.9045301739745));
#27780=CARTESIAN_POINT('Ctrl Pts',(-4.97737405981722,-22.2017009246778,
-10.9024407792168));
#27781=CARTESIAN_POINT('Ctrl Pts',(-4.98072713948359,-22.1636141852628,
-10.9005864070342));
#27782=CARTESIAN_POINT('Ctrl Pts',(-4.98460401281169,-22.1195778130665,
-10.8984423583474));
#27783=CARTESIAN_POINT('Ctrl Pts',(-4.98790553699991,-22.0753865188053,
-10.8966131076855));
#27784=CARTESIAN_POINT('Ctrl Pts',(-4.99062402522946,-22.0310585545324,
-10.8951063751095));
#27785=CARTESIAN_POINT('Ctrl Pts',(-4.99646709998867,-21.935780743007,-10.8918678284097));
#27786=CARTESIAN_POINT('Ctrl Pts',(-4.99956713935828,-21.8397718638307,
-10.8901472474313));
#27787=CARTESIAN_POINT('Ctrl Pts',(-4.99993867929236,-21.7441269948327,
-10.8899402435468));
#27788=CARTESIAN_POINT('Ctrl Pts',(-4.99996345275608,-21.7377496058228,
-10.8899264409841));
#27789=CARTESIAN_POINT('Ctrl Pts',(-4.9999761122425,-21.7313738326033,-10.8899193583874));
#27790=CARTESIAN_POINT('Ctrl Pts',(-4.99997666922209,-21.7249999979848,
-10.8899189904778));
#27791=CARTESIAN_POINT('',(-0.222506667109494,-27.2208450130247,-12.6980506686299));
#27792=CARTESIAN_POINT('Origin',(-0.213746562105115,-27.2208450130247,-12.1981274139594));
#27793=CARTESIAN_POINT('',(6.27271730358628E-11,-16.2250000002193,-12.7000029635389));
#27794=CARTESIAN_POINT('Ctrl Pts',(6.27271660968204E-11,-16.2250000002193,
-12.7000029635389));
#27795=CARTESIAN_POINT('Ctrl Pts',(-0.160551351076563,-16.2250000007214,
-12.7000063618174));
#27796=CARTESIAN_POINT('Ctrl Pts',(-0.320152850111539,-16.2314747517667,
-12.6969639953539));
#27797=CARTESIAN_POINT('Ctrl Pts',(-0.478672850296259,-16.244274252264,
-12.6909831439331));
#27798=CARTESIAN_POINT('Ctrl Pts',(-0.626368403327257,-16.2561997462222,
-12.6854106915159));
#27799=CARTESIAN_POINT('Ctrl Pts',(-0.773125198619939,-16.2736151280446,
-12.6772876607414));
#27800=CARTESIAN_POINT('Ctrl Pts',(-0.918842228003057,-16.296362307571,
-12.6667173659353));
#27801=CARTESIAN_POINT('Ctrl Pts',(-0.978670211742676,-16.3057017642741,
-12.6623774515927));
#27802=CARTESIAN_POINT('Ctrl Pts',(-1.03842121787906,-16.315986503065,-12.6576040485612));
#27803=CARTESIAN_POINT('Ctrl Pts',(-1.09801247670689,-16.3271894613611,
-12.6524178644869));
#27804=CARTESIAN_POINT('Ctrl Pts',(-1.27977392123081,-16.3613600078959,
-12.6365992976794));
#27805=CARTESIAN_POINT('Ctrl Pts',(-1.46078267828966,-16.4042424440069,
-12.6168750403301));
#27806=CARTESIAN_POINT('Ctrl Pts',(-1.63879216927802,-16.4552660581236,
-12.5937448757344));
#27807=CARTESIAN_POINT('Ctrl Pts',(-1.76562069343311,-16.4916194550102,
-12.5772650542213));
#27808=CARTESIAN_POINT('Ctrl Pts',(-1.89092589627654,-16.5321045091344,
-12.5590568756658));
#27809=CARTESIAN_POINT('Ctrl Pts',(-2.01389066817964,-16.5765012422573,
-12.5393079697913));
#27810=CARTESIAN_POINT('Ctrl Pts',(-2.06065103568712,-16.5933841878752,
-12.5317979644274));
#27811=CARTESIAN_POINT('Ctrl Pts',(-2.10711393447791,-16.6108244062646,
-12.5240683173945));
#27812=CARTESIAN_POINT('Ctrl Pts',(-2.15327890344298,-16.628821268942,-12.5161272078686));
#27813=CARTESIAN_POINT('Ctrl Pts',(-2.2785130815824,-16.6776423199905,-12.4945849357239));
#27814=CARTESIAN_POINT('Ctrl Pts',(-2.40149825470153,-16.7305125267001,
-12.4714978808614));
#27815=CARTESIAN_POINT('Ctrl Pts',(-2.52242557701601,-16.7875152782616,
-12.4469915584264));
#27816=CARTESIAN_POINT('Ctrl Pts',(-2.64440787895254,-16.8450153263822,
-12.4222714408764));
#27817=CARTESIAN_POINT('Ctrl Pts',(-2.76429623934248,-16.9067202916339,
-12.3961068901205));
#27818=CARTESIAN_POINT('Ctrl Pts',(-2.88226076887571,-16.9727602251875,
-12.3686145128557));
#27819=CARTESIAN_POINT('Ctrl Pts',(-2.92752129411295,-16.9980983678572,
-12.3580662621235));
#27820=CARTESIAN_POINT('Ctrl Pts',(-2.97249834394842,-17.0240751256557,
-12.3473224388959));
#27821=CARTESIAN_POINT('Ctrl Pts',(-3.01720053215441,-17.0506995836214,
-12.3363892993782));
#27822=CARTESIAN_POINT('Ctrl Pts',(-3.05217654869923,-17.0715311697178,
-12.327834960452));
#27823=CARTESIAN_POINT('Ctrl Pts',(-3.08692270139852,-17.0927295755552,
-12.3191781477242));
#27824=CARTESIAN_POINT('Ctrl Pts',(-3.12143510339615,-17.1142923538109,
-12.3104257191235));
#27825=CARTESIAN_POINT('Ctrl Pts',(-3.2295983220598,-17.1818709448236,-12.2829952653223));
#27826=CARTESIAN_POINT('Ctrl Pts',(-3.33495104508456,-17.2526947376596,
-12.2547577203916));
#27827=CARTESIAN_POINT('Ctrl Pts',(-3.43746722042114,-17.3266314645754,
-12.2259329280528));
#27828=CARTESIAN_POINT('Ctrl Pts',(-3.54078845940789,-17.4011488195829,
-12.1968817734598));
#27829=CARTESIAN_POINT('Ctrl Pts',(-3.64122887555301,-17.478828602327,-12.167233589157));
#27830=CARTESIAN_POINT('Ctrl Pts',(-3.73872681749338,-17.5595740196141,
-12.1372060767936));
#27831=CARTESIAN_POINT('Ctrl Pts',(-3.79359932791705,-17.605018094264,-12.1203063868887));
#27832=CARTESIAN_POINT('Ctrl Pts',(-3.84753913837293,-17.6514338734209,
-12.1032864556262));
#27833=CARTESIAN_POINT('Ctrl Pts',(-3.90052960838985,-17.6988086717544,
-12.0861850380435));
#27834=CARTESIAN_POINT('Ctrl Pts',(-3.92560168088156,-17.7212237282301,
-12.0780936212056));
#27835=CARTESIAN_POINT('Ctrl Pts',(-3.95047870207009,-17.7438665863787,
-12.0699791062562));
#27836=CARTESIAN_POINT('Ctrl Pts',(-3.97516256360717,-17.7667417119757,
-12.061844261215));
#27837=CARTESIAN_POINT('Ctrl Pts',(-4.07214610519881,-17.8566186824578,
-12.029882240961));
#27838=CARTESIAN_POINT('Ctrl Pts',(-4.16604631669613,-17.9499957710841,
-11.997638384144));
#27839=CARTESIAN_POINT('Ctrl Pts',(-4.25671783397987,-18.0468318032717,
-11.9653814957961));
#27840=CARTESIAN_POINT('Ctrl Pts',(-4.26675558549422,-18.0575519947702,
-11.9618105107772));
#27841=CARTESIAN_POINT('Ctrl Pts',(-4.27675380593103,-18.0683145412742,
-11.9582393689533));
#27842=CARTESIAN_POINT('Ctrl Pts',(-4.28671232658364,-18.0791193597846,
-11.9546684365246));
#27843=CARTESIAN_POINT('Ctrl Pts',(-4.30808442495687,-18.1023077079503,
-11.9470048164136));
#27844=CARTESIAN_POINT('Ctrl Pts',(-4.32928991266167,-18.1257142901536,
-11.9393354731834));
#27845=CARTESIAN_POINT('Ctrl Pts',(-4.35031349209773,-18.1493216466888,
-11.9316693999324));
#27846=CARTESIAN_POINT('Ctrl Pts',(-4.42593746646665,-18.234239732639,-11.904093747137));
#27847=CARTESIAN_POINT('Ctrl Pts',(-4.49941729284665,-18.3220081127293,
-11.8764827830282));
#27848=CARTESIAN_POINT('Ctrl Pts',(-4.56995033927333,-18.4117704764363,
-11.8492830907707));
#27849=CARTESIAN_POINT('Ctrl Pts',(-4.5920703872979,-18.4399210795449,-11.8407529261249));
#27850=CARTESIAN_POINT('Ctrl Pts',(-4.61390078044836,-18.4682674406524,
-11.8322632536808));
#27851=CARTESIAN_POINT('Ctrl Pts',(-4.6354173416563,-18.4967822997718,-11.8238278939559));
#27852=CARTESIAN_POINT('Ctrl Pts',(-4.65353301373796,-18.5207901248266,
-11.8167258199213));
#27853=CARTESIAN_POINT('Ctrl Pts',(-4.67143565529656,-18.5449204374923,
-11.8096599383198));
#27854=CARTESIAN_POINT('Ctrl Pts',(-4.68912315776799,-18.5691708542537,
-11.8026338819312));
#27855=CARTESIAN_POINT('Ctrl Pts',(-4.78633495947354,-18.7024529108523,
-11.7640181643344));
#27856=CARTESIAN_POINT('Ctrl Pts',(-4.87725397819097,-18.8396319188562,
-11.7265223047439));
#27857=CARTESIAN_POINT('Ctrl Pts',(-4.96178027815071,-18.9806973912532,
-11.6906454810317));
#27858=CARTESIAN_POINT('Ctrl Pts',(-5.04630657811045,-19.1217628636502,
-11.6547686573195));
#27859=CARTESIAN_POINT('Ctrl Pts',(-5.12444023116057,-19.2667148316449,
-11.6205113851506));
#27860=CARTESIAN_POINT('Ctrl Pts',(-5.19612983342037,-19.4155215868604,
-11.5883663492601));
#27861=CARTESIAN_POINT('Ctrl Pts',(-5.20862363940037,-19.4414550928302,
-11.5827642280462));
#27862=CARTESIAN_POINT('Ctrl Pts',(-5.22092652900315,-19.4675351737443,
-11.5772236713179));
#27863=CARTESIAN_POINT('Ctrl Pts',(-5.23303411516651,-19.4937521092468,
-11.5717487071689));
#27864=CARTESIAN_POINT('Ctrl Pts',(-5.2881331110772,-19.6130596906717,-11.5468333340149));
#27865=CARTESIAN_POINT('Ctrl Pts',(-5.33931133249327,-19.7355273100298,
-11.5232195967625));
#27866=CARTESIAN_POINT('Ctrl Pts',(-5.38606864208178,-19.8601850940752,
-11.5013248529885));
#27867=CARTESIAN_POINT('Ctrl Pts',(-5.43394641197694,-19.9878300923159,
-11.4789054384938));
#27868=CARTESIAN_POINT('Ctrl Pts',(-5.47718805239988,-20.1177702057423,
-11.4582890473383));
#27869=CARTESIAN_POINT('Ctrl Pts',(-5.51529287795625,-20.2489262530324,
-11.4399142062654));
#27870=CARTESIAN_POINT('Ctrl Pts',(-5.53349773916788,-20.3115870211403,
-11.4311354905349));
#27871=CARTESIAN_POINT('Ctrl Pts',(-5.55053071326472,-20.3745249014908,
-11.4228682121373));
#27872=CARTESIAN_POINT('Ctrl Pts',(-5.56634084337765,-20.4376206162029,
-11.4151587639929));
#27873=CARTESIAN_POINT('Ctrl Pts',(-5.57372038673109,-20.4670712000253,
-11.411560298553));
#27874=CARTESIAN_POINT('Ctrl Pts',(-5.58084550385779,-20.496565737035,-11.4080784831432));
#27875=CARTESIAN_POINT('Ctrl Pts',(-5.58771530165224,-20.5261026282267,
-11.4047148520531));
#27876=CARTESIAN_POINT('Ctrl Pts',(-5.62523447933326,-20.6874174007898,
-11.3863444900279));
#27877=CARTESIAN_POINT('Ctrl Pts',(-5.65520198469204,-20.8502556764816,
-11.3714677743116));
#27878=CARTESIAN_POINT('Ctrl Pts',(-5.67746909575661,-21.0145222008876,
-11.3603357097898));
#27879=CARTESIAN_POINT('Ctrl Pts',(-5.69973620682117,-21.1787887252936,
-11.3492036452679));
#27880=CARTESIAN_POINT('Ctrl Pts',(-5.7143028423889,-21.344483527548,-11.3418164518137));
#27881=CARTESIAN_POINT('Ctrl Pts',(-5.72106920988503,-21.5115041954204,
-11.3384023158398));
#27882=CARTESIAN_POINT('Ctrl Pts',(-5.72241125095109,-21.5446310681913,
-11.3377251562435));
#27883=CARTESIAN_POINT('Ctrl Pts',(-5.72343991250265,-21.577851098803,-11.3372063173585));
#27884=CARTESIAN_POINT('Ctrl Pts',(-5.72415500646433,-21.6111318063052,
-11.3368457725736));
#27885=CARTESIAN_POINT('Ctrl Pts',(-5.72623376206871,-21.7078777738921,
-11.3357976802496));
#27886=CARTESIAN_POINT('Ctrl Pts',(-5.72565676881658,-21.8053972850323,
-11.3360902643429));
#27887=CARTESIAN_POINT('Ctrl Pts',(-5.72239835662252,-21.9027047860458,
-11.3377334731175));
#27888=CARTESIAN_POINT('Ctrl Pts',(-5.72062014903454,-21.9558082383917,
-11.3386302185682));
#27889=CARTESIAN_POINT('Ctrl Pts',(-5.7180441674224,-22.0088482095149,-11.3399287986014));
#27890=CARTESIAN_POINT('Ctrl Pts',(-5.71467206515978,-22.0616642937744,
-11.3416278896644));
#27891=CARTESIAN_POINT('Ctrl Pts',(-5.71244343540748,-22.0965705592471,
-11.3427508226598));
#27892=CARTESIAN_POINT('Ctrl Pts',(-5.70987306068047,-22.1313912428016,
-11.3440456125498));
#27893=CARTESIAN_POINT('Ctrl Pts',(-5.70696482992104,-22.1661172689757,
-11.3455089795396));
#27894=CARTESIAN_POINT('Ctrl Pts',(-5.69462104364358,-22.3135095087314,
-11.351720140504));
#27895=CARTESIAN_POINT('Ctrl Pts',(-5.67617402862204,-22.4594930247,-11.3609766046823));
#27896=CARTESIAN_POINT('Ctrl Pts',(-5.65179657073802,-22.6041168008349,
-11.3730908517823));
#27897=CARTESIAN_POINT('Ctrl Pts',(-5.64581627910689,-22.6395959866547,
-11.3760627256707));
#27898=CARTESIAN_POINT('Ctrl Pts',(-5.63947902636718,-22.674993314026,-11.37920660631));
#27899=CARTESIAN_POINT('Ctrl Pts',(-5.63278512402843,-22.7103090990635,
-11.3825196496405));
#27900=CARTESIAN_POINT('Ctrl Pts',(-5.60992706383812,-22.8309039776864,
-11.3938328926529));
#27901=CARTESIAN_POINT('Ctrl Pts',(-5.5828943210023,-22.9506186766624,-11.407126368778));
#27902=CARTESIAN_POINT('Ctrl Pts',(-5.55175036832976,-23.0692983375885,
-11.4222623891215));
#27903=CARTESIAN_POINT('Ctrl Pts',(-5.54599612621493,-23.0912259172459,
-11.425058961754));
#27904=CARTESIAN_POINT('Ctrl Pts',(-5.54010166696578,-23.113118194875,-11.4279183783432));
#27905=CARTESIAN_POINT('Ctrl Pts',(-5.53406756508731,-23.1349742360145,
-11.4308396971981));
#27906=CARTESIAN_POINT('Ctrl Pts',(-5.52421074093538,-23.1706765092787,
-11.4356117290306));
#27907=CARTESIAN_POINT('Ctrl Pts',(-5.51396503368307,-23.2063209196587,
-11.440556474689));
#27908=CARTESIAN_POINT('Ctrl Pts',(-5.50334318984205,-23.2418731602839,
-11.4456638614209));
#27909=CARTESIAN_POINT('Ctrl Pts',(-5.47422129239668,-23.3393466988651,
-11.4596667779433));
#27910=CARTESIAN_POINT('Ctrl Pts',(-5.44216808041369,-23.4364412947893,
-11.4749420848567));
#27911=CARTESIAN_POINT('Ctrl Pts',(-5.40744548628297,-23.5323334983927,
-11.4912810885387));
#27912=CARTESIAN_POINT('Ctrl Pts',(-5.39271029600427,-23.5730271706748,
-11.4982148541241));
#27913=CARTESIAN_POINT('Ctrl Pts',(-5.37749497084478,-23.6135044192064,
-11.5053399237658));
#27914=CARTESIAN_POINT('Ctrl Pts',(-5.36182198105209,-23.6537033130043,
-11.5126393602804));
#27915=CARTESIAN_POINT('Ctrl Pts',(-5.34807804106611,-23.6889544802143,
-11.5190403736616));
#27916=CARTESIAN_POINT('Ctrl Pts',(-5.33399487567552,-23.7239839927291,
-11.5255704863632));
#27917=CARTESIAN_POINT('Ctrl Pts',(-5.31957905406975,-23.7587842426349,
-11.5322217060459));
#27918=CARTESIAN_POINT('Ctrl Pts',(-5.21968477345348,-23.9999321996973,
-11.5783112612298));
#27919=CARTESIAN_POINT('Ctrl Pts',(-5.10354433287028,-24.2309165425076,
-11.6303378369389));
#27920=CARTESIAN_POINT('Ctrl Pts',(-4.97181336051486,-24.4524305274384,
-11.6863685750191));
#27921=CARTESIAN_POINT('Ctrl Pts',(-4.9388890927989,-24.507794771794,-11.7003726546057));
#27922=CARTESIAN_POINT('Ctrl Pts',(-4.90499097869716,-24.5625673949196,
-11.7146271094503));
#27923=CARTESIAN_POINT('Ctrl Pts',(-4.87012937260121,-24.6167591578513,
-11.7291022614585));
#27924=CARTESIAN_POINT('Ctrl Pts',(-4.85012818139547,-24.6478506631936,
-11.7374071078345));
#27925=CARTESIAN_POINT('Ctrl Pts',(-4.82979351783297,-24.6787566452107,
-11.7457890364924));
#27926=CARTESIAN_POINT('Ctrl Pts',(-4.8091365289925,-24.7094657995178,-11.7542385964132));
#27927=CARTESIAN_POINT('Ctrl Pts',(-4.75805163579853,-24.7854097756689,
-11.7751344234586));
#27928=CARTESIAN_POINT('Ctrl Pts',(-4.70484306691042,-24.8603526764483,
-11.7965054522725));
#27929=CARTESIAN_POINT('Ctrl Pts',(-4.64981679274065,-24.9339036057569,
-11.8181502989304));
#27930=CARTESIAN_POINT('Ctrl Pts',(-4.59674139491384,-25.0048468940766,
-11.8390277591002));
#27931=CARTESIAN_POINT('Ctrl Pts',(-4.54197565148049,-25.074494762381,-11.86015946751));
#27932=CARTESIAN_POINT('Ctrl Pts',(-4.48582982272794,-25.1425250797796,
-11.8813605121747));
#27933=CARTESIAN_POINT('Ctrl Pts',(-4.41553127291297,-25.2277038501857,
-11.9079057200309));
#27934=CARTESIAN_POINT('Ctrl Pts',(-4.34292780254635,-25.3105340896975,
-11.9346152987756));
#27935=CARTESIAN_POINT('Ctrl Pts',(-4.26816207748717,-25.3908946583701,
-11.9613004937469));
#27936=CARTESIAN_POINT('Ctrl Pts',(-4.24447716774308,-25.4163519493211,
-11.9697540522979));
#27937=CARTESIAN_POINT('Ctrl Pts',(-4.22057495581456,-25.4415611563123,
-11.9782052033095));
#27938=CARTESIAN_POINT('Ctrl Pts',(-4.19645917443268,-25.4665176968915,
-11.9866480049388));
#27939=CARTESIAN_POINT('Ctrl Pts',(-4.17286608252751,-25.4909333252386,
-11.9949078158743));
#27940=CARTESIAN_POINT('Ctrl Pts',(-4.14905382008069,-25.5151351607172,
-12.0031669432351));
#27941=CARTESIAN_POINT('Ctrl Pts',(-4.12501614907756,-25.5391273663444,
-12.0114232046958));
#27942=CARTESIAN_POINT('Ctrl Pts',(-4.02840878195849,-25.6355520081795,
-12.0446051082944));
#27943=CARTESIAN_POINT('Ctrl Pts',(-3.92850678614335,-25.7282868705338,
-12.077622403484));
#27944=CARTESIAN_POINT('Ctrl Pts',(-3.82511519986933,-25.8174762702012,
-12.1102803913693));
#27945=CARTESIAN_POINT('Ctrl Pts',(-3.72253229275247,-25.9059680733701,
-12.1426829442132));
#27946=CARTESIAN_POINT('Ctrl Pts',(-3.61651425633536,-25.990969588709,-12.174732203639));
#27947=CARTESIAN_POINT('Ctrl Pts',(-3.50683570393584,-26.0725844683868,
-12.2062367240606));
#27948=CARTESIAN_POINT('Ctrl Pts',(-3.46142078356523,-26.106378981357,-12.2192818933754));
#27949=CARTESIAN_POINT('Ctrl Pts',(-3.41537782072005,-26.1395923956987,
-12.2322336131407));
#27950=CARTESIAN_POINT('Ctrl Pts',(-3.36868898142294,-26.1722302124877,
-12.2450779722361));
#27951=CARTESIAN_POINT('Ctrl Pts',(-3.34494120197565,-26.1888310894085,
-12.2516111183056));
#27952=CARTESIAN_POINT('Ctrl Pts',(-3.32106222794322,-26.2052544591287,
-12.2581052773238));
#27953=CARTESIAN_POINT('Ctrl Pts',(-3.2970531911292,-26.2214997110646,-12.2645583708621));
#27954=CARTESIAN_POINT('Ctrl Pts',(-3.18926116062163,-26.2944351105913,
-12.2935304642011));
#27955=CARTESIAN_POINT('Ctrl Pts',(-3.07933993096031,-26.3634600160092,
-12.321543437565));
#27956=CARTESIAN_POINT('Ctrl Pts',(-2.96741633131083,-26.4286185085995,
-12.348436395749));
#27957=CARTESIAN_POINT('Ctrl Pts',(-2.85491302458214,-26.4941144889006,
-12.3754686457203));
#27958=CARTESIAN_POINT('Ctrl Pts',(-2.74038608933694,-26.555704132313,-12.4013696670383));
#27959=CARTESIAN_POINT('Ctrl Pts',(-2.62393179659187,-26.613391646093,-12.4259692635982));
#27960=CARTESIAN_POINT('Ctrl Pts',(-2.55248788444691,-26.6487825412605,
-12.4410609478462));
#27961=CARTESIAN_POINT('Ctrl Pts',(-2.4803179587437,-26.6827039703826,-12.4556626512271));
#27962=CARTESIAN_POINT('Ctrl Pts',(-2.40743936726011,-26.7151488232138,
-12.469732783537));
#27963=CARTESIAN_POINT('Ctrl Pts',(-2.38826730991567,-26.7236840400223,
-12.4734341912893));
#27964=CARTESIAN_POINT('Ctrl Pts',(-2.36904016562544,-26.7321202559583,
-12.4771004338297));
#27965=CARTESIAN_POINT('Ctrl Pts',(-2.34975691726018,-26.7404574419512,
-12.4807309908139));
#27966=CARTESIAN_POINT('Ctrl Pts',(-2.22751843903057,-26.7933077143316,
-12.5037454618446));
#27967=CARTESIAN_POINT('Ctrl Pts',(-2.10312858729452,-26.8421272940633,
-12.5253046284089));
#27968=CARTESIAN_POINT('Ctrl Pts',(-1.9766937777278,-26.8868045823368,-12.545225735693));
#27969=CARTESIAN_POINT('Ctrl Pts',(-1.94746069254071,-26.8971344509743,
-12.5498317095404));
#27970=CARTESIAN_POINT('Ctrl Pts',(-1.91811838175776,-26.9072430607902,
-12.554350193968));
#27971=CARTESIAN_POINT('Ctrl Pts',(-1.88866833366658,-26.9171293622485,
-12.5587790777787));
#27972=CARTESIAN_POINT('Ctrl Pts',(-1.87307483841099,-26.9223640564129,
-12.5611241258573));
#27973=CARTESIAN_POINT('Ctrl Pts',(-1.85744283727076,-26.9275382488964,
-12.5634448995501));
#27974=CARTESIAN_POINT('Ctrl Pts',(-1.84177501360111,-26.9326510488533,
-12.5657408000865));
#27975=CARTESIAN_POINT('Ctrl Pts',(-1.70170427568277,-26.9783596091414,
-12.5862662086628));
#27976=CARTESIAN_POINT('Ctrl Pts',(-1.55841542310951,-27.019262367169,-12.6048539316864));
#27977=CARTESIAN_POINT('Ctrl Pts',(-1.41371523767078,-27.0546908316659,
-12.6210683091496));
#27978=CARTESIAN_POINT('Ctrl Pts',(-1.39045059543795,-27.0603869581005,
-12.623675228343));
#27979=CARTESIAN_POINT('Ctrl Pts',(-1.36714948897486,-27.0659416747688,
-12.6262208411194));
#27980=CARTESIAN_POINT('Ctrl Pts',(-1.34381943497189,-27.0713523220188,
-12.6287033905082));
#27981=CARTESIAN_POINT('Ctrl Pts',(-1.33278908881188,-27.0739104520647,
-12.6298771288593));
#27982=CARTESIAN_POINT('Ctrl Pts',(-1.32175599390771,-27.0764361857391,
-12.6310365715612));
#27983=CARTESIAN_POINT('Ctrl Pts',(-1.31072022027439,-27.0789295403597,
-12.6321816971157));
#27984=CARTESIAN_POINT('Ctrl Pts',(-0.951608746146348,-27.1600649716452,
-12.6694448505291));
#27985=CARTESIAN_POINT('Ctrl Pts',(-0.588860750681474,-27.207157585446,
-12.6916310828017));
#27986=CARTESIAN_POINT('Ctrl Pts',(-0.222506667109494,-27.2208450130247,
-12.6980506686299));
#27987=CARTESIAN_POINT('',(0.214833815848646,-16.2288732699618,-12.6981828003682));
#27988=CARTESIAN_POINT('Origin',(-7.67065009257134E-6,-21.1105838635361,
-10.4083425226561));
#27989=CARTESIAN_POINT('',(0.187614356002326,-16.7285211545107,-12.1982543436608));
#27990=CARTESIAN_POINT('Origin',(0.206375791602559,-16.2288732699618,-12.1982543436608));
#27991=CARTESIAN_POINT('Ctrl Pts',(-4.99997666922215,-21.7249999972923,
-10.8899189904778));
#27992=CARTESIAN_POINT('Ctrl Pts',(-4.99998234101381,-21.6600944959454,
-10.8899160716605));
#27993=CARTESIAN_POINT('Ctrl Pts',(-4.99873301488811,-21.595304502466,-10.8906091337332));
#27994=CARTESIAN_POINT('Ctrl Pts',(-4.99623155731798,-21.530911809512,-10.8919978308171));
#27995=CARTESIAN_POINT('Ctrl Pts',(-4.98793986214795,-21.3174664216997,
-10.8966010081967));
#27996=CARTESIAN_POINT('Ctrl Pts',(-4.96617998392237,-21.106513506024,-10.9087478277567));
#27997=CARTESIAN_POINT('Ctrl Pts',(-4.93119702679394,-20.8980705932228,
-10.9278316856883));
#27998=CARTESIAN_POINT('Ctrl Pts',(-4.92101994987409,-20.8374313639778,
-10.9333834716446));
#27999=CARTESIAN_POINT('Ctrl Pts',(-4.90972407973498,-20.7770045122468,
-10.9395221982223));
#28000=CARTESIAN_POINT('Ctrl Pts',(-4.89731618003943,-20.7167903516954,
-10.9462325729994));
#28001=CARTESIAN_POINT('Ctrl Pts',(-4.88614901395925,-20.6625973337186,
-10.952271940776));
#28002=CARTESIAN_POINT('Ctrl Pts',(-4.87407481030087,-20.608546748349,-10.9587774566803));
#28003=CARTESIAN_POINT('Ctrl Pts',(-4.86109898192199,-20.5546510400728,
-10.9657377511903));
#28004=CARTESIAN_POINT('Ctrl Pts',(-4.83174926734893,-20.432745631922,-10.9814810741789));
#28005=CARTESIAN_POINT('Ctrl Pts',(-4.79756722607834,-20.3114529823632,
-10.9996494442541));
#28006=CARTESIAN_POINT('Ctrl Pts',(-4.75898711148544,-20.1918167377945,
-11.0198136305987));
#28007=CARTESIAN_POINT('Ctrl Pts',(-4.720655625942,-20.0729514874565,-11.0398478691053));
#28008=CARTESIAN_POINT('Ctrl Pts',(-4.67798326007562,-19.9557228113236,
-11.0618515925471));
#28009=CARTESIAN_POINT('Ctrl Pts',(-4.63143601061823,-19.8411294983212,
-11.0853880635562));
#28010=CARTESIAN_POINT('Ctrl Pts',(-4.61955732598353,-19.8118857117974,
-11.091394483265));
#28011=CARTESIAN_POINT('Ctrl Pts',(-4.60742646402923,-19.7828133652514,
-11.0975006724954));
#28012=CARTESIAN_POINT('Ctrl Pts',(-4.5950515077976,-19.7539286231138,-11.1036992902712));
#28013=CARTESIAN_POINT('Ctrl Pts',(-4.5765422227149,-19.7107255671386,-11.1129705944588));
#28014=CARTESIAN_POINT('Ctrl Pts',(-4.55746124119458,-19.6678824271789,
-11.1224592641773));
#28015=CARTESIAN_POINT('Ctrl Pts',(-4.53783003076107,-19.625452757179,-11.1321433191472));
#28016=CARTESIAN_POINT('Ctrl Pts',(-4.47768226052557,-19.4954531297508,
-11.1618141494433));
#28017=CARTESIAN_POINT('Ctrl Pts',(-4.41224167944152,-19.3685202707715,
-11.1933951840664));
#28018=CARTESIAN_POINT('Ctrl Pts',(-4.34153092407304,-19.244728467047,-11.2264766384861));
#28019=CARTESIAN_POINT('Ctrl Pts',(-4.27166647685399,-19.122418276859,-11.2591621544898));
#28020=CARTESIAN_POINT('Ctrl Pts',(-4.19665731093853,-19.0031743253473,
-11.2933118568733));
#28021=CARTESIAN_POINT('Ctrl Pts',(-4.11656733346088,-18.887044107912,-11.3285184255984));
#28022=CARTESIAN_POINT('Ctrl Pts',(-4.09415340249297,-18.8545439779474,
-11.3383713138857));
#28023=CARTESIAN_POINT('Ctrl Pts',(-4.07133677950163,-18.8222802633444,
-11.3483085153344));
#28024=CARTESIAN_POINT('Ctrl Pts',(-4.04811668956903,-18.7902510724644,
-11.3583218371279));
#28025=CARTESIAN_POINT('Ctrl Pts',(-3.95293798793259,-18.6589640356236,
-11.3993662503985));
#28026=CARTESIAN_POINT('Ctrl Pts',(-3.85068360691524,-18.5315166896151,
-11.4417695249564));
#28027=CARTESIAN_POINT('Ctrl Pts',(-3.74359091922971,-18.4105578102084,
-11.4840110886132));
#28028=CARTESIAN_POINT('Ctrl Pts',(-3.65812755471859,-18.3140287845111,
-11.5177211974015));
#28029=CARTESIAN_POINT('Ctrl Pts',(-3.56928502721573,-18.221183434314,-11.5514631987063));
#28030=CARTESIAN_POINT('Ctrl Pts',(-3.47704521778017,-18.1319269682117,
-11.5849605673345));
#28031=CARTESIAN_POINT('Ctrl Pts',(-3.45368649324617,-18.1093237428005,
-11.5934434101676));
#28032=CARTESIAN_POINT('Ctrl Pts',(-3.43011673544645,-18.0869573014828,
-11.6019082045496));
#28033=CARTESIAN_POINT('Ctrl Pts',(-3.40633409590771,-18.0648240442483,
-11.610351129418));
#28034=CARTESIAN_POINT('Ctrl Pts',(-3.31351007565654,-17.9784375893547,
-11.6433039994176));
#28035=CARTESIAN_POINT('Ctrl Pts',(-3.21717077395441,-17.8953870071991,
-11.6760079177476));
#28036=CARTESIAN_POINT('Ctrl Pts',(-3.11744419797313,-17.8158628991426,
-11.7081356286851));
#28037=CARTESIAN_POINT('Ctrl Pts',(-3.01974880409736,-17.7379584992096,
-11.7396089781255));
#28038=CARTESIAN_POINT('Ctrl Pts',(-2.91880218367213,-17.6634380085559,
-11.7705299357143));
#28039=CARTESIAN_POINT('Ctrl Pts',(-2.81469354777058,-17.5925182788626,
-11.8005824061336));
#28040=CARTESIAN_POINT('Ctrl Pts',(-2.77718074687106,-17.5669642248997,
-11.8114110211627));
#28041=CARTESIAN_POINT('Ctrl Pts',(-2.73925715163687,-17.5418780564676,
-11.822126755195));
#28042=CARTESIAN_POINT('Ctrl Pts',(-2.70092611220132,-17.5172712981393,
-11.8327143231594));
#28043=CARTESIAN_POINT('Ctrl Pts',(-2.67904116891535,-17.5032221745467,
-11.838759249878));
#28044=CARTESIAN_POINT('Ctrl Pts',(-2.65704081181229,-17.4893405226794,
-11.844757694435));
#28045=CARTESIAN_POINT('Ctrl Pts',(-2.63492637900982,-17.475627931408,-11.8507069466921));
#28046=CARTESIAN_POINT('Ctrl Pts',(-2.52129478005667,-17.4051678980948,
-11.8812762609759));
#28047=CARTESIAN_POINT('Ctrl Pts',(-2.40539761260767,-17.339541832115,-11.9103691828862));
#28048=CARTESIAN_POINT('Ctrl Pts',(-2.28706438300499,-17.2786609863284,
-11.9378018380373));
#28049=CARTESIAN_POINT('Ctrl Pts',(-2.17007764129556,-17.2184728903471,
-11.9649223430159));
#28050=CARTESIAN_POINT('Ctrl Pts',(-2.05070998244525,-17.1629227076627,
-11.990420463892));
#28051=CARTESIAN_POINT('Ctrl Pts',(-1.9287742755276,-17.111967992304,-12.0141038891066));
#28052=CARTESIAN_POINT('Ctrl Pts',(-1.88971247615946,-17.0956447764183,
-12.0216908152619));
#28053=CARTESIAN_POINT('Ctrl Pts',(-1.85038696231078,-17.0797934904909,
-12.0290913799705));
#28054=CARTESIAN_POINT('Ctrl Pts',(-1.81079108152958,-17.0644136789109,
-12.0362988569225));
#28055=CARTESIAN_POINT('Ctrl Pts',(-1.79349000894213,-17.0576936052245,
-12.039448100719));
#28056=CARTESIAN_POINT('Ctrl Pts',(-1.77613909683667,-17.051064243726,-12.0425602292707));
#28057=CARTESIAN_POINT('Ctrl Pts',(-1.75873817661222,-17.0445256622699,
-12.0456346167024));
#28058=CARTESIAN_POINT('Ctrl Pts',(-1.57559193939589,-16.9757065093197,
-12.0779928186019));
#28059=CARTESIAN_POINT('Ctrl Pts',(-1.38618282670759,-16.9170929190887,
-12.106111409062));
#28060=CARTESIAN_POINT('Ctrl Pts',(-1.19382360958483,-16.8697505421426,
-12.1290510506316));
#28061=CARTESIAN_POINT('Ctrl Pts',(-1.07428552506051,-16.840330495931,-12.1433064674186));
#28062=CARTESIAN_POINT('Ctrl Pts',(-0.953608844790518,-16.8152636561332,
-12.1555615926741));
#28063=CARTESIAN_POINT('Ctrl Pts',(-0.832596678325463,-16.794811151152,
-12.1655876027153));
#28064=CARTESIAN_POINT('Ctrl Pts',(-0.822547136999614,-16.7931126583473,
-12.1664202198413));
#28065=CARTESIAN_POINT('Ctrl Pts',(-0.812493307657583,-16.7914456570965,
-12.1672376753802));
#28066=CARTESIAN_POINT('Ctrl Pts',(-0.80243580320674,-16.789810359935,-12.1680398086835));
#28067=CARTESIAN_POINT('Ctrl Pts',(-0.695016219010128,-16.772344502277,
-12.1766070259623));
#28068=CARTESIAN_POINT('Ctrl Pts',(-0.586813990430978,-16.7583188314844,
-12.1835103776808));
#28069=CARTESIAN_POINT('Ctrl Pts',(-0.477998355044125,-16.7478515832007,
-12.1886740113227));
#28070=CARTESIAN_POINT('Ctrl Pts',(-0.368071624253781,-16.7372774558695,
-12.1938903698289));
#28071=CARTESIAN_POINT('Ctrl Pts',(-0.257518864835462,-16.7303350234902,
-12.1973311475917));
#28072=CARTESIAN_POINT('Ctrl Pts',(-0.146521659500288,-16.7270973793117,
-12.1989418461153));
#28073=CARTESIAN_POINT('Ctrl Pts',(-0.0355244541651161,-16.7238597351332,
-12.200552544639));
#28074=CARTESIAN_POINT('Ctrl Pts',(0.0759172118544166,-16.7243270033065,
-12.2003330628352));
#28075=CARTESIAN_POINT('Ctrl Pts',(0.187614356002326,-16.7285211545107,
-12.1982543436608));
#28076=CARTESIAN_POINT('Origin',(0.,-0.999999999999945,0.));
#28077=CARTESIAN_POINT('',(1.68059064192457,0.,-11.5786706963397));
#28078=CARTESIAN_POINT('',(-1.68059064192455,0.,-11.5786706963397));
#28079=CARTESIAN_POINT('Origin',(0.,0.,0.));
#28080=CARTESIAN_POINT('',(3.46944695195361E-15,-0.848960155852397,-12.5489601558525));
#28081=CARTESIAN_POINT('Ctrl Pts',(1.68059064192456,5.84411658722412E-15,
-11.5786706963397));
#28082=CARTESIAN_POINT('Ctrl Pts',(0.869714200879421,-0.346830427858442,
-12.0468304278567));
#28083=CARTESIAN_POINT('Ctrl Pts',(2.62089735138893E-11,-0.848960155837265,
-12.5489601558373));
#28084=CARTESIAN_POINT('Ctrl Pts',(-2.62073916106111E-11,-0.84896015583726,
-12.5489601558373));
#28085=CARTESIAN_POINT('Ctrl Pts',(-0.869714200879411,-0.346830427858444,
-12.0468304278567));
#28086=CARTESIAN_POINT('Ctrl Pts',(-1.68059064192454,1.5245521531889E-15,
-11.5786706963397));
#28087=CARTESIAN_POINT('Origin',(0.,-21.725,-21.5));
#28088=CARTESIAN_POINT('',(5.00001172195141,-21.7250000023451,-10.8899050240605));
#28089=CARTESIAN_POINT('Ctrl Pts',(5.00002344390285,-21.725000004566,-10.8899064672807));
#28090=CARTESIAN_POINT('Ctrl Pts',(5.00001152141201,-21.7882748865493,-10.8899059311929));
#28091=CARTESIAN_POINT('Ctrl Pts',(4.99879927122167,-21.8516587474073,-10.8905724964452));
#28092=CARTESIAN_POINT('Ctrl Pts',(4.99638310479926,-21.9151469697699,-10.8919139762305));
#28093=CARTESIAN_POINT('Ctrl Pts',(4.990060963821,-22.0812702502336,-10.8954240921909));
#28094=CARTESIAN_POINT('Ctrl Pts',(4.97522566801055,-22.2490604010701,-10.9036628526843));
#28095=CARTESIAN_POINT('Ctrl Pts',(4.95239190657507,-22.4133417782704,-10.9161966077095));
#28096=CARTESIAN_POINT('Ctrl Pts',(4.93706818544299,-22.5235908941913,-10.9246080018325));
#28097=CARTESIAN_POINT('Ctrl Pts',(4.91817280124604,-22.6326091834789,-10.9349360548822));
#28098=CARTESIAN_POINT('Ctrl Pts',(4.89581131018126,-22.7404136161556,-10.947035666435));
#28099=CARTESIAN_POINT('Ctrl Pts',(4.88482334405882,-22.7933864456807,-10.9529811609215));
#28100=CARTESIAN_POINT('Ctrl Pts',(4.87299763343813,-22.8460709434397,-10.9593547795652));
#28101=CARTESIAN_POINT('Ctrl Pts',(4.86034588878338,-22.8984725567251,-10.9661397284499));
#28102=CARTESIAN_POINT('Ctrl Pts',(4.79422159663562,-23.1723493761247,-11.0016012362895));
#28103=CARTESIAN_POINT('Ctrl Pts',(4.70571139778224,-23.4385476398574,-11.048296021071));
#28104=CARTESIAN_POINT('Ctrl Pts',(4.5945753052774,-23.6973148396108,-11.1039144219712));
#28105=CARTESIAN_POINT('Ctrl Pts',(4.57643367394708,-23.7395554747861,-11.1129934574274));
#28106=CARTESIAN_POINT('Ctrl Pts',(4.55767872580587,-23.7816218623763,-11.1223160148244));
#28107=CARTESIAN_POINT('Ctrl Pts',(4.53831397330642,-23.8235009601411,-11.1318694619704));
#28108=CARTESIAN_POINT('Ctrl Pts',(4.49243330473491,-23.9227245884666,-11.1545043261255));
#28109=CARTESIAN_POINT('Ctrl Pts',(4.44358835177731,-24.0198695778208,-11.1781944567248));
#28110=CARTESIAN_POINT('Ctrl Pts',(4.39196253677333,-24.1147721393631,-11.2026884744858));
#28111=CARTESIAN_POINT('Ctrl Pts',(4.38586624978507,-24.1259788050794,-11.2055808755405));
#28112=CARTESIAN_POINT('Ctrl Pts',(4.37973123224749,-24.1371542364042,-11.2084844733256));
#28113=CARTESIAN_POINT('Ctrl Pts',(4.37355782324247,-24.1482981914757,-11.211398844494));
#28114=CARTESIAN_POINT('Ctrl Pts',(4.30980965679331,-24.2633734606211,-11.241493370579));
#28115=CARTESIAN_POINT('Ctrl Pts',(4.24191254319682,-24.3752010240399,-11.2727586116446));
#28116=CARTESIAN_POINT('Ctrl Pts',(4.16995158407907,-24.4839330077148,-11.3048712900011));
#28117=CARTESIAN_POINT('Ctrl Pts',(4.15102174685418,-24.5125357219829,-11.3133187562606));
#28118=CARTESIAN_POINT('Ctrl Pts',(4.13181047583863,-24.540924060519,-11.321824927182));
#28119=CARTESIAN_POINT('Ctrl Pts',(4.11231885863813,-24.5691004415348,-11.330384030271));
#28120=CARTESIAN_POINT('Ctrl Pts',(4.09072627107986,-24.6003139097607,-11.3398657054427));
#28121=CARTESIAN_POINT('Ctrl Pts',(4.06879087060822,-24.631265442764,-11.349411600643));
#28122=CARTESIAN_POINT('Ctrl Pts',(4.04651664935594,-24.6619547164646,-11.3590125548681));
#28123=CARTESIAN_POINT('Ctrl Pts',(3.95198509136906,-24.7921996675026,-11.3997589024409));
#28124=CARTESIAN_POINT('Ctrl Pts',(3.85121377604902,-24.9178494050859,-11.4415547761407));
#28125=CARTESIAN_POINT('Ctrl Pts',(3.74406673020293,-25.0389046938329,-11.4838238526989));
#28126=CARTESIAN_POINT('Ctrl Pts',(3.65760774291518,-25.1365865066,-11.5179315737653));
#28127=CARTESIAN_POINT('Ctrl Pts',(3.56661037535839,-25.2315979421455,-11.5524774355491));
#28128=CARTESIAN_POINT('Ctrl Pts',(3.47237289989047,-25.32257642859,-11.5866541000274));
#28129=CARTESIAN_POINT('Ctrl Pts',(3.44980057505032,-25.3443681408498,-11.5948402995061));
#28130=CARTESIAN_POINT('Ctrl Pts',(3.42703985515985,-25.365930928998,-11.6030062755313));
#28131=CARTESIAN_POINT('Ctrl Pts',(3.40410824423346,-25.3872461770815,-11.6111410187316));
#28132=CARTESIAN_POINT('Ctrl Pts',(3.18470052889287,-25.5911886693441,-11.6889735541861));
#28133=CARTESIAN_POINT('Ctrl Pts',(2.94900150199431,-25.7739299727301,-11.7643260370852));
#28134=CARTESIAN_POINT('Ctrl Pts',(2.696322025512,-25.9356885348437,-11.8339822109817));
#28135=CARTESIAN_POINT('Ctrl Pts',(2.67583165664485,-25.9488059144238,-11.8396307928011));
#28136=CARTESIAN_POINT('Ctrl Pts',(2.65522784224586,-25.9617864319314,-11.8452425778975));
#28137=CARTESIAN_POINT('Ctrl Pts',(2.63451048821384,-25.9746299235927,-11.850815697453));
#28138=CARTESIAN_POINT('Ctrl Pts',(2.49198588806835,-26.0629864536144,-11.8891558559009));
#28139=CARTESIAN_POINT('Ctrl Pts',(2.34348714532903,-26.1448951794979,-11.925708481326));
#28140=CARTESIAN_POINT('Ctrl Pts',(2.19098226277494,-26.2192493576819,-11.9595228911452));
#28141=CARTESIAN_POINT('Ctrl Pts',(2.06371540788928,-26.2812986655245,-11.9877413554686));
#28142=CARTESIAN_POINT('Ctrl Pts',(1.93366011679675,-26.3380870977829,-12.0140526922932));
#28143=CARTESIAN_POINT('Ctrl Pts',(1.80197549472834,-26.3889932854301,-12.0379121302175));
#28144=CARTESIAN_POINT('Ctrl Pts',(1.78615368929159,-26.3951096244819,-12.0407788232203));
#28145=CARTESIAN_POINT('Ctrl Pts',(1.77030548911759,-26.4011421911994,-12.0436108293463));
#28146=CARTESIAN_POINT('Ctrl Pts',(1.75443286313541,-26.4070898465095,-12.0464071869036));
#28147=CARTESIAN_POINT('Ctrl Pts',(1.58749408431246,-26.4696437248303,-12.0758176018078));
#28148=CARTESIAN_POINT('Ctrl Pts',(1.41707113919231,-26.5234254396691,-12.1015564914957));
#28149=CARTESIAN_POINT('Ctrl Pts',(1.24311481949365,-26.5680679342181,-12.1231373121445));
#28150=CARTESIAN_POINT('Ctrl Pts',(1.10701123067326,-26.6029962641146,-12.1400221666015));
#28151=CARTESIAN_POINT('Ctrl Pts',(0.968744958017119,-26.6323308041622,
-12.1543618446964));
#28152=CARTESIAN_POINT('Ctrl Pts',(0.82829974493686,-26.655915398572,-12.1659311274838));
#28153=CARTESIAN_POINT('Ctrl Pts',(0.819544689390747,-26.6573856119709,
-12.1666523319394));
#28154=CARTESIAN_POINT('Ctrl Pts',(0.810782077925004,-26.6588333343054,
-12.1673626945561));
#28155=CARTESIAN_POINT('Ctrl Pts',(0.802011826845791,-26.6602585575249,
-12.1680621755967));
#28156=CARTESIAN_POINT('Ctrl Pts',(0.686607364415905,-26.6790125382266,
-12.1772663856868));
#28157=CARTESIAN_POINT('Ctrl Pts',(0.570129714195444,-26.6936648092245,
-12.1844828834562));
#28158=CARTESIAN_POINT('Ctrl Pts',(0.453284493692702,-26.704253353433,-12.1897098761392));
#28159=CARTESIAN_POINT('Ctrl Pts',(0.338620856724135,-26.7146442019755,
-12.1948392771438));
#28160=CARTESIAN_POINT('Ctrl Pts',(0.223601703868209,-26.7211215084667,
-12.1980527358992));
#28161=CARTESIAN_POINT('Ctrl Pts',(0.108892707969018,-26.7236778818544,
-12.1993273015262));
#28162=CARTESIAN_POINT('Ctrl Pts',(0.00742336080110954,-26.7259392000425,
-12.200454757495));
#28163=CARTESIAN_POINT('Ctrl Pts',(-0.0938039899970676,-26.7251318549737,
-12.200064783988));
#28164=CARTESIAN_POINT('Ctrl Pts',(-0.194315056429422,-26.7212227391145,
-12.19812741396));
#28165=CARTESIAN_POINT('',(-4.99999160226712,-21.72500000341,10.8899098036299));
#28166=CARTESIAN_POINT('',(-5.,-21.725,-21.5));
#28167=CARTESIAN_POINT('Origin',(-3.89307326486085,-21.3390068413815,11.5111137315767));
#28168=CARTESIAN_POINT('Ctrl Pts',(4.99980122230293,-21.6804159506306,10.890014011117));
#28169=CARTESIAN_POINT('Ctrl Pts',(4.99681149794833,-21.3451384759755,10.8916749023389));
#28170=CARTESIAN_POINT('Ctrl Pts',(4.96051653026192,-21.0171256611318,10.9120450197627));
#28171=CARTESIAN_POINT('Ctrl Pts',(4.89293081575696,-20.695811954881,10.94859196248));
#28172=CARTESIAN_POINT('Ctrl Pts',(4.89289834722306,-20.6956575940809,10.9486095198242));
#28173=CARTESIAN_POINT('Ctrl Pts',(4.89286587140735,-20.6955032348325,10.9486270809002));
#28174=CARTESIAN_POINT('Ctrl Pts',(4.89283338830974,-20.6953488771359,10.9486446457078));
#28175=CARTESIAN_POINT('Ctrl Pts',(4.86683621968048,-20.5718119190493,10.9627022725655));
#28176=CARTESIAN_POINT('Ctrl Pts',(4.83616535482728,-20.4492430359115,10.9791550395257));
#28177=CARTESIAN_POINT('Ctrl Pts',(4.80081433199506,-20.3277880416923,10.9978254612168));
#28178=CARTESIAN_POINT('Ctrl Pts',(4.79028605113857,-20.2916161805093,11.0033859069275));
#28179=CARTESIAN_POINT('Ctrl Pts',(4.77934296232174,-20.2555430495807,11.0091429015769));
#28180=CARTESIAN_POINT('Ctrl Pts',(4.76798568777015,-20.2195723261415,11.0150913877129));
#28181=CARTESIAN_POINT('Ctrl Pts',(4.73197766638454,-20.1055278365969,11.0339509490475));
#28182=CARTESIAN_POINT('Ctrl Pts',(4.69162361143881,-19.9922070920438,11.054822610137));
#28183=CARTESIAN_POINT('Ctrl Pts',(4.64765781272916,-19.8813291049973,11.0771437849085));
#28184=CARTESIAN_POINT('Ctrl Pts',(4.63098022901674,-19.839269664134,11.0856108950654));
#28185=CARTESIAN_POINT('Ctrl Pts',(4.61378318693029,-19.7975612928432,11.0942865168028));
#28186=CARTESIAN_POINT('Ctrl Pts',(4.5961074869497,-19.7562958657012,11.1031398492434));
#28187=CARTESIAN_POINT('Ctrl Pts',(4.59601302641415,-19.7560753395353,11.1031871622508));
#28188=CARTESIAN_POINT('Ctrl Pts',(4.59591855188769,-19.7558548240601,11.1032344805497));
#28189=CARTESIAN_POINT('Ctrl Pts',(4.59582406337146,-19.7556343192758,11.1032818041376));
#28190=CARTESIAN_POINT('Ctrl Pts',(4.50148136442582,-19.535469824063,11.1505323610586));
#28191=CARTESIAN_POINT('Ctrl Pts',(4.39280939934476,-19.3250607724011,11.2032466660903));
#28192=CARTESIAN_POINT('Ctrl Pts',(4.27010858683285,-19.1237335109746,11.2595416663626));
#28193=CARTESIAN_POINT('Ctrl Pts',(4.22574734402706,-19.0509456675633,11.2798945566549));
#28194=CARTESIAN_POINT('Ctrl Pts',(4.1795520246957,-18.9793451745005,11.3007157428127));
#28195=CARTESIAN_POINT('Ctrl Pts',(4.13153565263822,-18.9089010457424,11.3219170106647));
#28196=CARTESIAN_POINT('Ctrl Pts',(4.13080975140498,-18.9078360864848,11.3222375268933));
#28197=CARTESIAN_POINT('Ctrl Pts',(4.13008343381006,-18.9067713912948,11.3225581300807));
#28198=CARTESIAN_POINT('Ctrl Pts',(4.12935669989677,-18.9057069600664,11.3228788199229));
#28199=CARTESIAN_POINT('Ctrl Pts',(3.99139364898032,-18.7036355043609,11.3837585287321));
#28200=CARTESIAN_POINT('Ctrl Pts',(3.8371376032085,-18.510168652598,11.4481955970778));
#28201=CARTESIAN_POINT('Ctrl Pts',(3.67050413426203,-18.3298890659559,11.5125041611507));
#28202=CARTESIAN_POINT('Ctrl Pts',(3.61935966431457,-18.2745562210031,11.532242257245));
#28203=CARTESIAN_POINT('Ctrl Pts',(3.56704882610507,-18.220465779807,11.551968361796));
#28204=CARTESIAN_POINT('Ctrl Pts',(3.51368401016484,-18.1677506558258,11.5715760913822));
#28205=CARTESIAN_POINT('Ctrl Pts',(3.51140243577175,-18.165496858546,11.5724144057836));
#28206=CARTESIAN_POINT('Ctrl Pts',(3.50911892302814,-18.1632455637268,11.5732525081862));
#28207=CARTESIAN_POINT('Ctrl Pts',(3.5068334807527,-18.1609967819498,11.5740903902315));
#28208=CARTESIAN_POINT('Ctrl Pts',(3.28058390602085,-17.9383764488207,11.6570373359732));
#28209=CARTESIAN_POINT('Ctrl Pts',(3.03441230305267,-17.7380727100291,11.7384462854316));
#28210=CARTESIAN_POINT('Ctrl Pts',(2.76690911959257,-17.560361184534,11.8142501978774));
#28211=CARTESIAN_POINT('Ctrl Pts',(2.76267967067482,-17.5575514167792,11.8154487210923));
#28212=CARTESIAN_POINT('Ctrl Pts',(2.75844487664652,-17.554747289089,11.8166458456229));
#28213=CARTESIAN_POINT('Ctrl Pts',(2.75420473161427,-17.5519488025721,11.8178415553647));
#28214=CARTESIAN_POINT('Ctrl Pts',(2.61812893871101,-17.4621390746436,11.8562145709011));
#28215=CARTESIAN_POINT('Ctrl Pts',(2.4765031260948,-17.3783234220784,11.8930824769717));
#28216=CARTESIAN_POINT('Ctrl Pts',(2.33205830830434,-17.3021610874157,11.9272556062802));
#28217=CARTESIAN_POINT('Ctrl Pts',(2.1934549885892,-17.2290788364705,11.9600467388363));
#28218=CARTESIAN_POINT('Ctrl Pts',(2.0516181351631,-17.1625961247258,11.9905469912575));
#28219=CARTESIAN_POINT('Ctrl Pts',(1.90647238682508,-17.1027317310734,12.018406332931));
#28220=CARTESIAN_POINT('Ctrl Pts',(1.90049463025599,-17.1002662453358,12.0195537062755));
#28221=CARTESIAN_POINT('Ctrl Pts',(1.89451126025318,-17.0978119855393,12.0206965994529));
#28222=CARTESIAN_POINT('Ctrl Pts',(1.88852227143256,-17.0953689531127,12.0218349879028));
#28223=CARTESIAN_POINT('Ctrl Pts',(1.74366730051123,-17.0362796140396,12.0493690559644));
#28224=CARTESIAN_POINT('Ctrl Pts',(1.59552621727336,-16.9837569593759,12.0742699322544));
#28225=CARTESIAN_POINT('Ctrl Pts',(1.44393008546716,-16.9380315409714,12.0961660723804));
#28226=CARTESIAN_POINT('Ctrl Pts',(1.4372414835026,-16.9360140810288,12.0971321561724));
#28227=CARTESIAN_POINT('Ctrl Pts',(1.43054599105914,-16.9340098044762,12.0980924221045));
#28228=CARTESIAN_POINT('Ctrl Pts',(1.42384361790784,-16.9320187407269,12.0990468327269));
#28229=CARTESIAN_POINT('Ctrl Pts',(1.30167033908194,-16.8957249114949,12.1164441743029));
#28230=CARTESIAN_POINT('Ctrl Pts',(1.17692640634316,-16.8638307026676,12.1318926790276));
#28231=CARTESIAN_POINT('Ctrl Pts',(1.05166758402415,-16.8368632173258,12.145026869394));
#28232=CARTESIAN_POINT('Ctrl Pts',(1.02161405873619,-16.8303928706655,12.1481781741485));
#28233=CARTESIAN_POINT('Ctrl Pts',(0.991530972260571,-16.824205939237,12.1511963433226));
#28234=CARTESIAN_POINT('Ctrl Pts',(0.961446789444828,-16.8183093004312,
12.1540765186724));
#28235=CARTESIAN_POINT('Ctrl Pts',(0.954305426975421,-16.8169095603977,
12.154760212701));
#28236=CARTESIAN_POINT('Ctrl Pts',(0.94716354233454,-16.8155260870371,12.1554361899411));
#28237=CARTESIAN_POINT('Ctrl Pts',(0.9400214921796,-16.8141589728088,12.1561043861852));
#28238=CARTESIAN_POINT('Ctrl Pts',(0.740888611067521,-16.7760414310389,
12.1747348690792));
#28239=CARTESIAN_POINT('Ctrl Pts',(0.540319367334083,-16.7500849358455,
12.1875483549967));
#28240=CARTESIAN_POINT('Ctrl Pts',(0.338393099035631,-16.7364089056273,
12.1943261791738));
#28241=CARTESIAN_POINT('Ctrl Pts',(0.218276230812764,-16.7282736494599,
12.1983580023754));
#28242=CARTESIAN_POINT('Ctrl Pts',(0.0976792709987591,-16.7244829836586,
12.2002544963976));
#28243=CARTESIAN_POINT('Ctrl Pts',(-0.0233802237688804,-16.7250541700989,
12.1999734032215));
#28244=CARTESIAN_POINT('Ctrl Pts',(-0.0310072465875391,-16.7250901561405,
12.1999556937137));
#28245=CARTESIAN_POINT('Ctrl Pts',(-0.038636314214975,-16.7251434546806,
12.1999293526452));
#28246=CARTESIAN_POINT('Ctrl Pts',(-0.0462674058931988,-16.7252140718672,
12.1998943671571));
#28247=CARTESIAN_POINT('Ctrl Pts',(-0.18722183044295,-16.7265184468272,
12.1992481477764));
#28248=CARTESIAN_POINT('Ctrl Pts',(-0.329643856273163,-16.7338997864519,
12.1955863398144));
#28249=CARTESIAN_POINT('Ctrl Pts',(-0.470516177416762,-16.7471945727973,
12.1890167310796));
#28250=CARTESIAN_POINT('Ctrl Pts',(-0.48794375998246,-16.7488392960818,
12.1882039922979));
#28251=CARTESIAN_POINT('Ctrl Pts',(-0.50534763266374,-16.7505744639994,
12.1873467792465));
#28252=CARTESIAN_POINT('Ctrl Pts',(-0.522722097817875,-16.752399717777,
12.186445319834));
#28253=CARTESIAN_POINT('Ctrl Pts',(-0.530415524002231,-16.7532079415169,
12.1860461529309));
#28254=CARTESIAN_POINT('Ctrl Pts',(-0.538103390625485,-16.7540338501271,
12.1856383264121));
#28255=CARTESIAN_POINT('Ctrl Pts',(-0.54578521940695,-16.7548774165665,
12.1852218592229));
#28256=CARTESIAN_POINT('Ctrl Pts',(-0.703274852129899,-16.7721718620023,
12.1766836235324));
#28257=CARTESIAN_POINT('Ctrl Pts',(-0.85856929506714,-16.7967821156056,
12.1645667163415));
#28258=CARTESIAN_POINT('Ctrl Pts',(-1.01171262550948,-16.8284257973864,
12.1491355438321));
#28259=CARTESIAN_POINT('Ctrl Pts',(-1.01938094710419,-16.8300102864244,
12.1483628611887));
#28260=CARTESIAN_POINT('Ctrl Pts',(-1.02704392334188,-16.8316124164775,
12.1475818645961));
#28261=CARTESIAN_POINT('Ctrl Pts',(-1.03470156646483,-16.83323215306,12.1467925870816));
#28262=CARTESIAN_POINT('Ctrl Pts',(-1.34782292335014,-16.8994632516321,
12.1145189955418));
#28263=CARTESIAN_POINT('Ctrl Pts',(-1.65208339548054,-16.9949098339779,
12.0684105022407));
#28264=CARTESIAN_POINT('Ctrl Pts',(-1.94762155723166,-17.1199183744877,
12.0104202812587));
#28265=CARTESIAN_POINT('Ctrl Pts',(-1.95561400152696,-17.1232990674938,
12.0088520113333));
#28266=CARTESIAN_POINT('Ctrl Pts',(-1.96360003997595,-17.1267013710748,
12.0072750551016));
#28267=CARTESIAN_POINT('Ctrl Pts',(-1.97157967297179,-17.1301252908132,
12.0056894514984));
#28268=CARTESIAN_POINT('Ctrl Pts',(-2.24657951621896,-17.248122871886,11.9510452413496));
#28269=CARTESIAN_POINT('Ctrl Pts',(-2.50646165958052,-17.3887242213049,
11.8876066014172));
#28270=CARTESIAN_POINT('Ctrl Pts',(-2.75051310584763,-17.5495107130101,
11.8188822479445));
#28271=CARTESIAN_POINT('Ctrl Pts',(-2.76764198236856,-17.560795595787,11.814058793781));
#28272=CARTESIAN_POINT('Ctrl Pts',(-2.78469289361425,-17.5721799027812,
11.8092092914112));
#28273=CARTESIAN_POINT('Ctrl Pts',(-2.80166560080175,-17.5836627944812,
11.804334948629));
#28274=CARTESIAN_POINT('Ctrl Pts',(-2.80984000984178,-17.5891931941211,
11.8019873636937));
#28275=CARTESIAN_POINT('Ctrl Pts',(-2.81799647167743,-17.594746591815,11.7996339650656));
#28276=CARTESIAN_POINT('Ctrl Pts',(-2.82613496059901,-17.6003228993675,
11.797274885726));
#28277=CARTESIAN_POINT('Ctrl Pts',(-2.95920726957285,-17.6915010196188,
11.758701615208));
#28278=CARTESIAN_POINT('Ctrl Pts',(-3.08768365836285,-17.7889671040843,
11.7185499987111));
#28279=CARTESIAN_POINT('Ctrl Pts',(-3.21161242246995,-17.8928275550485,
11.6773084639027));
#28280=CARTESIAN_POINT('Ctrl Pts',(-3.32656816409712,-17.9891680233194,
11.6390530092155));
#28281=CARTESIAN_POINT('Ctrl Pts',(-3.43810167779714,-18.0915480029184,
11.5996663706253));
#28282=CARTESIAN_POINT('Ctrl Pts',(-3.5442103899849,-18.1981656868409,11.5603064707464));
#28283=CARTESIAN_POINT('Ctrl Pts',(-3.55253769572624,-18.2065329361755,
11.5572175451202));
#28284=CARTESIAN_POINT('Ctrl Pts',(-3.56083171048927,-18.2149264067726,
11.5541287493587));
#28285=CARTESIAN_POINT('Ctrl Pts',(-3.56909146879911,-18.2233452358416,
11.5510406406348));
#28286=CARTESIAN_POINT('Ctrl Pts',(-3.74708806780088,-18.4047697867366,
11.4844923435088));
#28287=CARTESIAN_POINT('Ctrl Pts',(-3.90975366927737,-18.597920472388,11.4181748287074));
#28288=CARTESIAN_POINT('Ctrl Pts',(-4.05749346642025,-18.8031764790736,
11.3542801320666));
#28289=CARTESIAN_POINT('Ctrl Pts',(-4.09019119673731,-18.8486036806967,
11.3401389757914));
#28290=CARTESIAN_POINT('Ctrl Pts',(-4.12215767289834,-18.8946239569954,
11.326116534228));
#28291=CARTESIAN_POINT('Ctrl Pts',(-4.15339703200001,-18.9412416390385,
11.3122366565339));
#28292=CARTESIAN_POINT('Ctrl Pts',(-4.16101062698528,-18.9526032085596,
11.3088538801183));
#28293=CARTESIAN_POINT('Ctrl Pts',(-4.16858130744644,-18.9640006749311,
11.3054794637819));
#28294=CARTESIAN_POINT('Ctrl Pts',(-4.17610909058629,-18.9754340590648,
11.3021137712519));
#28295=CARTESIAN_POINT('Ctrl Pts',(-4.27733878375571,-19.1291842330849,
11.2568536972321));
#28296=CARTESIAN_POINT('Ctrl Pts',(-4.37098435674311,-19.2903091486333,
11.2130472316835));
#28297=CARTESIAN_POINT('Ctrl Pts',(-4.45554758708343,-19.4563285341691,
11.1722457075528));
#28298=CARTESIAN_POINT('Ctrl Pts',(-4.51249022059306,-19.5681215793025,
11.1447710447962));
#28299=CARTESIAN_POINT('Ctrl Pts',(-4.56531514750588,-19.6821327615954,
11.1186590444948));
#28300=CARTESIAN_POINT('Ctrl Pts',(-4.61357514386104,-19.7975966837424,
11.0943808405147));
#28301=CARTESIAN_POINT('Ctrl Pts',(-4.61949338394989,-19.8117563038103,
11.0914035456343));
#28302=CARTESIAN_POINT('Ctrl Pts',(-4.62534375904922,-19.8259396168614,
11.088453350286));
#28303=CARTESIAN_POINT('Ctrl Pts',(-4.631125403848,-19.8401452323389,11.0855311429861));
#28304=CARTESIAN_POINT('Ctrl Pts',(-4.70435613436058,-20.0200745837608,
11.0485182543125));
#28305=CARTESIAN_POINT('Ctrl Pts',(-4.76726266141392,-20.2043492164639,
11.0156989175618));
#28306=CARTESIAN_POINT('Ctrl Pts',(-4.81941146141461,-20.3931233167233,
10.9880108622482));
#28307=CARTESIAN_POINT('Ctrl Pts',(-4.85028537022025,-20.5048841694408,
10.9716185676078));
#28308=CARTESIAN_POINT('Ctrl Pts',(-4.87738947269955,-20.6182217880058,
10.9570246661856));
#28309=CARTESIAN_POINT('Ctrl Pts',(-4.90064154479525,-20.7331649364595,
10.944421333994));
#28310=CARTESIAN_POINT('Ctrl Pts',(-4.90391515449991,-20.7493475375075,
10.9426469376992));
#28311=CARTESIAN_POINT('Ctrl Pts',(-4.90711191771618,-20.7655594581114,
10.9409122343397));
#28312=CARTESIAN_POINT('Ctrl Pts',(-4.91023176158242,-20.7818011622264,
10.9392176722592));
#28313=CARTESIAN_POINT('Ctrl Pts',(-4.93378311546319,-20.9044079777082,
10.9264256118414));
#28314=CARTESIAN_POINT('Ctrl Pts',(-4.95272914746289,-21.0287068137377,
10.9160511524931));
#28315=CARTESIAN_POINT('Ctrl Pts',(-4.96704580471618,-21.1536260169313,
10.9081724913842));
#28316=CARTESIAN_POINT('Ctrl Pts',(-4.98091661294089,-21.2746549890179,
10.9005391873681));
#28317=CARTESIAN_POINT('Ctrl Pts',(-4.99044175459251,-21.396268070175,10.8952486342404));
#28318=CARTESIAN_POINT('Ctrl Pts',(-4.99555846674246,-21.5174896076691,
10.8923943107704));
#28319=CARTESIAN_POINT('Ctrl Pts',(-4.99848614792585,-21.586850166548,10.8907611235069));
#28320=CARTESIAN_POINT('Ctrl Pts',(-4.99996980849573,-21.6560823781017,
10.8899259483772));
#28321=CARTESIAN_POINT('Ctrl Pts',(-4.9999916022669,-21.7250000027207,10.88990980363));
#28322=CARTESIAN_POINT('Ctrl Pts',(0.187614356002326,-16.7285211545107,
-12.1982543436608));
#28323=CARTESIAN_POINT('Ctrl Pts',(0.5158722932195,-16.7408470150613,-12.1921453596449));
#28324=CARTESIAN_POINT('Ctrl Pts',(0.83589624549473,-16.7849264922226,-12.1702069739155));
#28325=CARTESIAN_POINT('Ctrl Pts',(1.30454329276147,-16.8955146240847,-12.1165436423938));
#28326=CARTESIAN_POINT('Ctrl Pts',(1.45884748782628,-16.9398479007978,-12.0951867686849));
#28327=CARTESIAN_POINT('Ctrl Pts',(1.76364451604006,-17.0436033466199,-12.0459567376793));
#28328=CARTESIAN_POINT('Ctrl Pts',(1.91480729566499,-17.1034045601589,-12.0179123563443));
#28329=CARTESIAN_POINT('Ctrl Pts',(2.35241421703558,-17.3013507250399,-11.9268899925891));
#28330=CARTESIAN_POINT('Ctrl Pts',(2.62606025966841,-17.4585239024972,-11.8567015361229));
#28331=CARTESIAN_POINT('Ctrl Pts',(3.14021868341892,-17.8214071167348,-11.7044430212222));
#28332=CARTESIAN_POINT('Ctrl Pts',(3.38265418689342,-18.0295254408124,-11.6214946028354));
#28333=CARTESIAN_POINT('Ctrl Pts',(3.81899306541419,-18.4824433648695,-11.4567396232169));
#28334=CARTESIAN_POINT('Ctrl Pts',(4.01441011445594,-18.727563041203,-11.3746407517478));
#28335=CARTESIAN_POINT('Ctrl Pts',(4.36024299024928,-19.2575320761983,-11.2195371333797));
#28336=CARTESIAN_POINT('Ctrl Pts',(4.50951743476146,-19.5419625548479,-11.1469697786176));
#28337=CARTESIAN_POINT('Ctrl Pts',(4.68989568786932,-19.9842448672363,-11.0558220109167));
#28338=CARTESIAN_POINT('Ctrl Pts',(4.74315776047347,-20.134924483598,-11.0281977430586));
#28339=CARTESIAN_POINT('Ctrl Pts',(4.83557077179125,-20.4431493848349,-10.9795288829077));
#28340=CARTESIAN_POINT('Ctrl Pts',(4.87488907212697,-20.6016955942573,-10.9583929606265));
#28341=CARTESIAN_POINT('Ctrl Pts',(4.96879046717059,-21.0795960122762,-10.9074448087627));
#28342=CARTESIAN_POINT('Ctrl Pts',(4.99999999999992,-21.4009211496768,-10.8899035808404));
#28343=CARTESIAN_POINT('Ctrl Pts',(5.,-21.7249999999987,-10.8899035808404));
#28344=CARTESIAN_POINT('Origin',(0.,-244.63,0.));
#28345=CARTESIAN_POINT('',(9.10831056865844E-16,-237.1925,-7.4375));
#28346=CARTESIAN_POINT('',(-9.10831056865844E-16,-237.1925,7.4375));
#28347=CARTESIAN_POINT('Origin',(0.,-237.1925,0.));
#28348=CARTESIAN_POINT('Origin',(0.,-237.1925,0.));
#28349=CARTESIAN_POINT('',(-9.10831056865844E-16,-212.63,7.4375));
#28350=CARTESIAN_POINT('',(-9.10831056865844E-16,-244.63,7.4375));
#28351=CARTESIAN_POINT('Origin',(0.,-212.63,0.));
#28352=CARTESIAN_POINT('Origin',(0.,-237.1925,0.));
#28353=CARTESIAN_POINT('',(0.,-244.63,0.));
#28354=CARTESIAN_POINT('',(-9.10831056865844E-16,-237.1925,-7.4375));
#28355=CARTESIAN_POINT('Origin',(0.,-44.45,0.));
#28356=CARTESIAN_POINT('',(1.55530143491714E-15,-43.45,12.7));
#28357=CARTESIAN_POINT('',(-1.55530143491714E-15,-43.45,-12.7));
#28358=CARTESIAN_POINT('Origin',(0.,-43.45,0.));
#28359=CARTESIAN_POINT('Origin',(0.,-43.45,0.));
#28360=CARTESIAN_POINT('',(-1.4328367550024E-15,-44.45,-11.7));
#28361=CARTESIAN_POINT('',(-1.43283675500241E-15,-44.45,-11.7));
#28362=CARTESIAN_POINT('Origin',(0.,-44.45,0.));
#28363=CARTESIAN_POINT('Origin',(0.,-244.63,0.));
#28364=CARTESIAN_POINT('',(-9.42978035343463E-16,-47.63,7.70000000000001));
#28365=CARTESIAN_POINT('Origin',(0.,-47.63,0.));
#28366=CARTESIAN_POINT('',(-9.42978035343463E-16,-44.45,7.70000000000001));
#28367=CARTESIAN_POINT('',(-9.42978035343463E-16,-244.63,7.70000000000001));
#28368=CARTESIAN_POINT('Origin',(0.,-44.45,0.));
#28369=CARTESIAN_POINT('Origin',(0.,-244.63,0.));
#28370=CARTESIAN_POINT('',(-1.55530143491714E-15,-244.63,12.7));
#28371=CARTESIAN_POINT('',(-1.71325927436869E-11,-16.2250000000013,12.7000002117864));
#28372=CARTESIAN_POINT('Ctrl Pts',(-5.7251211610453,-21.780229807,11.3363568967879));
#28373=CARTESIAN_POINT('Ctrl Pts',(-5.72592155092587,-21.7036657452032,
11.3359526814757));
#28374=CARTESIAN_POINT('Ctrl Pts',(-5.7250008654272,-21.6269621693104,11.3364279110386));
#28375=CARTESIAN_POINT('Ctrl Pts',(-5.72240032932084,-21.550122887081,11.3377497611332));
#28376=CARTESIAN_POINT('Ctrl Pts',(-5.71973912251023,-21.4714909385792,
11.3391024500906));
#28377=CARTESIAN_POINT('Ctrl Pts',(-5.71531887266977,-21.3927158329317,
11.3413417249685));
#28378=CARTESIAN_POINT('Ctrl Pts',(-5.70913701129969,-21.3137889985803,
11.3444562327139));
#28379=CARTESIAN_POINT('Ctrl Pts',(-5.70665440520126,-21.2820923576238,
11.3457070041984));
#28380=CARTESIAN_POINT('Ctrl Pts',(-5.70388716149817,-21.250371194257,11.3470991961792));
#28381=CARTESIAN_POINT('Ctrl Pts',(-5.70083299908356,-21.2186249953703,
11.3486331200433));
#28382=CARTESIAN_POINT('Ctrl Pts',(-5.69081304792642,-21.1144735721361,
11.3536655446856));
#28383=CARTESIAN_POINT('Ctrl Pts',(-5.67772497916359,-21.0103130463191,
11.3602133443104));
#28384=CARTESIAN_POINT('Ctrl Pts',(-5.6616113424946,-20.906924066588,11.3682258570849));
#28385=CARTESIAN_POINT('Ctrl Pts',(-5.65013554789805,-20.8332926003141,
11.3739322008911));
#28386=CARTESIAN_POINT('Ctrl Pts',(-5.63712616237809,-20.7600526651473,
11.3803809524082));
#28387=CARTESIAN_POINT('Ctrl Pts',(-5.62261270070195,-20.6874823252654,
11.3875469885781));
#28388=CARTESIAN_POINT('Ctrl Pts',(-5.62071109870733,-20.6779739180949,
11.3884859064585));
#28389=CARTESIAN_POINT('Ctrl Pts',(-5.61878497703484,-20.6684770185026,
11.389436447028));
#28390=CARTESIAN_POINT('Ctrl Pts',(-5.61683442793834,-20.6589917496983,
11.3903985013602));
#28391=CARTESIAN_POINT('Ctrl Pts',(-5.57286731662002,-20.4451853553105,
11.4120840615902));
#28392=CARTESIAN_POINT('Ctrl Pts',(-5.51634888901757,-20.2366355634731,
11.4396871913827));
#28393=CARTESIAN_POINT('Ctrl Pts',(-5.44783320687091,-20.0331524601257,
11.4722129615946));
#28394=CARTESIAN_POINT('Ctrl Pts',(-5.40433526811686,-19.9039689609678,
11.4928623066246));
#28395=CARTESIAN_POINT('Ctrl Pts',(-5.35600285931867,-19.7768269845679,
11.5154955399265));
#28396=CARTESIAN_POINT('Ctrl Pts',(-5.30298711896009,-19.651672639573,11.5398582133199));
#28397=CARTESIAN_POINT('Ctrl Pts',(-5.29614565259561,-19.6355219787341,
11.5430021175536));
#28398=CARTESIAN_POINT('Ctrl Pts',(-5.28922082277232,-19.6193988034393,
11.5461768842716));
#28399=CARTESIAN_POINT('Ctrl Pts',(-5.28221377395364,-19.603304781917,11.5493814791098));
#28400=CARTESIAN_POINT('Ctrl Pts',(-5.21348500003055,-19.4454462603995,
11.5808138095882));
#28401=CARTESIAN_POINT('Ctrl Pts',(-5.13672427863156,-19.2901792507329,
11.6151706224263));
#28402=CARTESIAN_POINT('Ctrl Pts',(-5.05299140769763,-19.1391643487573,
11.6514834037853));
#28403=CARTESIAN_POINT('Ctrl Pts',(-4.97563621249873,-18.9996517882781,
11.6850303520615));
#28404=CARTESIAN_POINT('Ctrl Pts',(-4.89233170424652,-18.8637690311732,
11.7202458572368));
#28405=CARTESIAN_POINT('Ctrl Pts',(-4.80393880809263,-18.7327852615055,
11.7563670702825));
#28406=CARTESIAN_POINT('Ctrl Pts',(-4.79665111102847,-18.7219860901332,
11.7593451428395));
#28407=CARTESIAN_POINT('Ctrl Pts',(-4.78932883567085,-18.7112201915641,
11.7623293760803));
#28408=CARTESIAN_POINT('Ctrl Pts',(-4.78197246933197,-18.7004882614148,
11.7653193451523));
#28409=CARTESIAN_POINT('Ctrl Pts',(-4.76879514041666,-18.6812643447474,
11.7706752238692));
#28410=CARTESIAN_POINT('Ctrl Pts',(-4.75550582199898,-18.6621369757864,
11.7760511749375));
#28411=CARTESIAN_POINT('Ctrl Pts',(-4.74210471042919,-18.6431061081163,
11.7814457754623));
#28412=CARTESIAN_POINT('Ctrl Pts',(-4.60834180066191,-18.4531499077152,
11.8352918657269));
#28413=CARTESIAN_POINT('Ctrl Pts',(-4.46337134494643,-18.2726619633985,
11.8910215785681));
#28414=CARTESIAN_POINT('Ctrl Pts',(-4.3070685843823,-18.1012807046439,11.9473601508487));
#28415=CARTESIAN_POINT('Ctrl Pts',(-4.23602178678706,-18.0233800357215,
11.9729686246029));
#28416=CARTESIAN_POINT('Ctrl Pts',(-4.16263331204804,-17.9473613616324,
11.9987034169121));
#28417=CARTESIAN_POINT('Ctrl Pts',(-4.08689000518079,-17.8731928595689,
12.0244471838457));
#28418=CARTESIAN_POINT('Ctrl Pts',(-4.06785307389009,-17.8545517315786,
12.0309174891776));
#28419=CARTESIAN_POINT('Ctrl Pts',(-4.04866165056352,-17.8360279422144,
12.0373891632641));
#28420=CARTESIAN_POINT('Ctrl Pts',(-4.02932492572199,-17.817629051679,12.043857485744));
#28421=CARTESIAN_POINT('Ctrl Pts',(-3.91639267653785,-17.7101740349846,
12.0816344211914));
#28422=CARTESIAN_POINT('Ctrl Pts',(-3.79852390663081,-17.6070014770466,
12.1192899300043));
#28423=CARTESIAN_POINT('Ctrl Pts',(-3.67755706750205,-17.5096130464424,
12.1558863936335));
#28424=CARTESIAN_POINT('Ctrl Pts',(-3.53535623962652,-17.3951294775805,
12.1989068400869));
#28425=CARTESIAN_POINT('Ctrl Pts',(-3.38821406470576,-17.2879449005781,
12.2406999056768));
#28426=CARTESIAN_POINT('Ctrl Pts',(-3.23615133134969,-17.1878625428924,
12.2807705197441));
#28427=CARTESIAN_POINT('Ctrl Pts',(-3.21342145855415,-17.1729025378401,
12.28676015271));
#28428=CARTESIAN_POINT('Ctrl Pts',(-3.19057632043218,-17.1580972322623,
12.2927127051079));
#28429=CARTESIAN_POINT('Ctrl Pts',(-3.16761661322188,-17.1434477682921,
12.2986262265451));
#28430=CARTESIAN_POINT('Ctrl Pts',(-2.97069010100861,-17.0177986117496,
12.3493467841231));
#28431=CARTESIAN_POINT('Ctrl Pts',(-2.7651980604181,-16.9035088337294,12.3972286024479));
#28432=CARTESIAN_POINT('Ctrl Pts',(-2.55156492209342,-16.8013656927296,
12.4410424599757));
#28433=CARTESIAN_POINT('Ctrl Pts',(-2.45522310210993,-16.7553023517146,
12.4608011304135));
#28434=CARTESIAN_POINT('Ctrl Pts',(-2.35722584962307,-16.7117088138121,
12.4797328794738));
#28435=CARTESIAN_POINT('Ctrl Pts',(-2.25761329062413,-16.6706547188598,
12.4977270822136));
#28436=CARTESIAN_POINT('Ctrl Pts',(-2.23350870399902,-16.6607203090019,
12.5020813807383));
#28437=CARTESIAN_POINT('Ctrl Pts',(-2.20935990045449,-16.6509543847314,
12.5063717966401));
#28438=CARTESIAN_POINT('Ctrl Pts',(-2.18516698386428,-16.6413565854661,
12.5105976886306));
#28439=CARTESIAN_POINT('Ctrl Pts',(-1.8843086225196,-16.5220002379706,12.5631500518289));
#28440=CARTESIAN_POINT('Ctrl Pts',(-1.57625905934626,-16.4284075359873,
12.6057869924533));
#28441=CARTESIAN_POINT('Ctrl Pts',(-1.26100785637197,-16.3600575419048,
12.6372413556761));
#28442=CARTESIAN_POINT('Ctrl Pts',(-1.23565759797098,-16.3545613217624,
12.6397706917357));
#28443=CARTESIAN_POINT('Ctrl Pts',(-1.21026079827882,-16.3492283346357,
12.6422277248466));
#28444=CARTESIAN_POINT('Ctrl Pts',(-1.18481746577651,-16.3440583132815,
12.6446117999945));
#28445=CARTESIAN_POINT('Ctrl Pts',(-1.16292712550636,-16.3396102510382,
12.6466629548978));
#28446=CARTESIAN_POINT('Ctrl Pts',(-1.14100210430354,-16.3352837242408,
12.6486600728867));
#28447=CARTESIAN_POINT('Ctrl Pts',(-1.11904222815108,-16.3310792360298,
12.6506026687393));
#28448=CARTESIAN_POINT('Ctrl Pts',(-0.956285503636157,-16.2999174605833,
12.6650003154217));
#28449=CARTESIAN_POINT('Ctrl Pts',(-0.791601235446541,-16.2754586182219,
12.6764033427023));
#28450=CARTESIAN_POINT('Ctrl Pts',(-0.624967432599858,-16.2578763159761,
12.6846133447174));
#28451=CARTESIAN_POINT('Ctrl Pts',(-0.604806175958912,-16.2557490086599,
12.6856066843329));
#28452=CARTESIAN_POINT('Ctrl Pts',(-0.584611468485983,-16.2537238228531,
12.686552593652));
#28453=CARTESIAN_POINT('Ctrl Pts',(-0.564389928132223,-16.2518009854779,
12.6874508724902));
#28454=CARTESIAN_POINT('Ctrl Pts',(-0.394675486070499,-16.2356630817079,
12.6949899070625));
#28455=CARTESIAN_POINT('Ctrl Pts',(-0.222970110451938,-16.2267466956113,
12.6991803470038));
#28456=CARTESIAN_POINT('Ctrl Pts',(-0.052979955040351,-16.2252370584114,
12.6998894926019));
#28457=CARTESIAN_POINT('Ctrl Pts',(-0.0353121499055092,-16.2250801553495,
12.6999631971421));
#28458=CARTESIAN_POINT('Ctrl Pts',(-0.0176522202715522,-16.2250011418722,
12.7000000775714));
#28459=CARTESIAN_POINT('Ctrl Pts',(-1.713259621314E-11,-16.2250000000013,
12.7000002117864));
#28460=CARTESIAN_POINT('',(-1.55530143491714E-15,-15.875,12.7));
#28461=CARTESIAN_POINT('',(-1.55530143491714E-15,-244.63,12.7));
#28462=CARTESIAN_POINT('Origin',(0.,-15.875,0.));
#28463=CARTESIAN_POINT('Ctrl Pts',(-1.713259621314E-11,-16.2250000000013,
12.7000002117864));
#28464=CARTESIAN_POINT('Ctrl Pts',(0.221363672027344,-16.2250000000212,
12.7000018947916));
#28465=CARTESIAN_POINT('Ctrl Pts',(0.441513190754386,-16.2372332268251,
12.6942230208429));
#28466=CARTESIAN_POINT('Ctrl Pts',(0.660354951916768,-16.2616652077622,
12.6828260961163));
#28467=CARTESIAN_POINT('Ctrl Pts',(0.799573752842758,-16.2772079043309,
12.6755758062894));
#28468=CARTESIAN_POINT('Ctrl Pts',(0.938263335008136,-16.2976865147767,
12.6660523329633));
#28469=CARTESIAN_POINT('Ctrl Pts',(1.07639994840503,-16.3230822291724,12.6543021597253));
#28470=CARTESIAN_POINT('Ctrl Pts',(1.08491495480765,-16.3246476698283,12.6535778564585));
#28471=CARTESIAN_POINT('Ctrl Pts',(1.09342994759773,-16.3262326511218,12.6528447542495));
#28472=CARTESIAN_POINT('Ctrl Pts',(1.10194446509101,-16.3278370612125,12.6521029273764));
#28473=CARTESIAN_POINT('Ctrl Pts',(1.27949553558937,-16.3612934172959,12.6366338000235));
#28474=CARTESIAN_POINT('Ctrl Pts',(1.45703513698099,-16.4032419539272,12.6173536765979));
#28475=CARTESIAN_POINT('Ctrl Pts',(1.63041748363299,-16.4527210984502,12.5949092425891));
#28476=CARTESIAN_POINT('Ctrl Pts',(1.6346503273299,-16.4539290500616,12.5943612987941));
#28477=CARTESIAN_POINT('Ctrl Pts',(1.63888098675367,-16.4551414837025,12.593811470957));
#28478=CARTESIAN_POINT('Ctrl Pts',(1.64310946414815,-16.4563583966121,12.5932597642597));
#28479=CARTESIAN_POINT('Ctrl Pts',(1.81996315945393,-16.507255096502,12.5701849410938));
#28480=CARTESIAN_POINT('Ctrl Pts',(1.99304998846898,-16.5660000215187,12.5438162804331));
#28481=CARTESIAN_POINT('Ctrl Pts',(2.16251275385891,-16.63240593341,12.5145330951417));
#28482=CARTESIAN_POINT('Ctrl Pts',(2.1630668666123,-16.6326230687942,12.5144373443944));
#28483=CARTESIAN_POINT('Ctrl Pts',(2.16362094061177,-16.6328402860942,12.5143415624717));
#28484=CARTESIAN_POINT('Ctrl Pts',(2.16417497585848,-16.6330575853119,12.5142457493862));
#28485=CARTESIAN_POINT('Ctrl Pts',(2.33666764411718,-16.7007112627337,12.484415418421));
#28486=CARTESIAN_POINT('Ctrl Pts',(2.50538039674436,-16.7762931353467,12.4515685497952));
#28487=CARTESIAN_POINT('Ctrl Pts',(2.6703975412241,-16.8598778146148,12.4160773584821));
#28488=CARTESIAN_POINT('Ctrl Pts',(2.83063219705356,-16.9410400620732,12.381614764653));
#28489=CARTESIAN_POINT('Ctrl Pts',(2.98813248544786,-17.0302527035357,12.3444553838994));
#28490=CARTESIAN_POINT('Ctrl Pts',(3.14001471210688,-17.1259429702128,12.3057021386053));
#28491=CARTESIAN_POINT('Ctrl Pts',(3.14461081664355,-17.1288386511523,12.3045294275487));
#28492=CARTESIAN_POINT('Ctrl Pts',(3.14920178649894,-17.131740271378,12.3033552545028));
#28493=CARTESIAN_POINT('Ctrl Pts',(3.15378754001488,-17.1346477865787,12.3021796504457));
#28494=CARTESIAN_POINT('Ctrl Pts',(3.38076485787962,-17.2785587053891,12.2439917310906));
#28495=CARTESIAN_POINT('Ctrl Pts',(3.59505414777261,-17.4364785198026,12.1824013050721));
#28496=CARTESIAN_POINT('Ctrl Pts',(3.79709489785007,-17.6085262541715,12.1190881100363));
#28497=CARTESIAN_POINT('Ctrl Pts',(3.86478108590455,-17.666164405378,12.097877394753));
#28498=CARTESIAN_POINT('Ctrl Pts',(3.93109267813204,-17.7253882661821,12.0764737353512));
#28499=CARTESIAN_POINT('Ctrl Pts',(3.99604650387532,-17.7862025795357,12.0549415457737));
#28500=CARTESIAN_POINT('Ctrl Pts',(4.00258006511678,-17.7923197564087,12.0527756705899));
#28501=CARTESIAN_POINT('Ctrl Pts',(4.00909996613724,-17.7984531203158,12.0506084698285));
#28502=CARTESIAN_POINT('Ctrl Pts',(4.01560621589262,-17.8046026712755,12.0484400117636));
#28503=CARTESIAN_POINT('Ctrl Pts',(4.14721247732648,-17.9289937478159,12.0045771614675));
#28504=CARTESIAN_POINT('Ctrl Pts',(4.27353389575726,-18.0606680305253,11.9600313905221));
#28505=CARTESIAN_POINT('Ctrl Pts',(4.39314902114322,-18.198165116782,11.9159327227938));
#28506=CARTESIAN_POINT('Ctrl Pts',(4.50543725205698,-18.3272399684927,11.8745352710177));
#28507=CARTESIAN_POINT('Ctrl Pts',(4.61181501935763,-18.4614451487399,11.8335324557008));
#28508=CARTESIAN_POINT('Ctrl Pts',(4.71110159808237,-18.5995347793932,11.7938760921501));
#28509=CARTESIAN_POINT('Ctrl Pts',(4.71690460935499,-18.6076057160052,11.7915582932323));
#28510=CARTESIAN_POINT('Ctrl Pts',(4.72268368303533,-18.6156902524801,11.7892449830829));
#28511=CARTESIAN_POINT('Ctrl Pts',(4.7284385795538,-18.6237881449308,11.7869363530806));
#28512=CARTESIAN_POINT('Ctrl Pts',(4.8696838599945,-18.8225387369724,11.7302745015473));
#28513=CARTESIAN_POINT('Ctrl Pts',(4.99754710031512,-19.0301338086101,11.6760653892489));
#28514=CARTESIAN_POINT('Ctrl Pts',(5.11150237280828,-19.2471420652657,11.6259546820761));
#28515=CARTESIAN_POINT('Ctrl Pts',(5.16114959164122,-19.3416866718558,11.6041228072496));
#28516=CARTESIAN_POINT('Ctrl Pts',(5.20815730681002,-19.4380178471292,11.583069405877));
#28517=CARTESIAN_POINT('Ctrl Pts',(5.2524838589806,-19.5361817726934,11.5629328655827));
#28518=CARTESIAN_POINT('Ctrl Pts',(5.25597752321097,-19.5439187109091,11.5613457737132));
#28519=CARTESIAN_POINT('Ctrl Pts',(5.25945467845056,-19.5516673853462,11.5597643117532));
#28520=CARTESIAN_POINT('Ctrl Pts',(5.2629152811409,-19.5594277771001,11.5581885580222));
#28521=CARTESIAN_POINT('Ctrl Pts',(5.31419025317372,-19.6744117569871,11.5348409692573));
#28522=CARTESIAN_POINT('Ctrl Pts',(5.36191135925266,-19.7924554425857,11.5126967199581));
#28523=CARTESIAN_POINT('Ctrl Pts',(5.40532924820431,-19.9118553979064,11.4922758454265));
#28524=CARTESIAN_POINT('Ctrl Pts',(5.42197752137286,-19.9576384408062,11.4844456098773));
#28525=CARTESIAN_POINT('Ctrl Pts',(5.43799345603299,-20.0036204551374,11.4768686567325));
#28526=CARTESIAN_POINT('Ctrl Pts',(5.45333635060538,-20.0497042730614,11.4695737653081));
#28527=CARTESIAN_POINT('Ctrl Pts',(5.45548050920907,-20.0561444538387,11.4685543094201));
#28528=CARTESIAN_POINT('Ctrl Pts',(5.45761164744171,-20.0625869137453,11.4675403033073));
#28529=CARTESIAN_POINT('Ctrl Pts',(5.45972965702712,-20.0690314064627,11.4665318240264));
#28530=CARTESIAN_POINT('Ctrl Pts',(5.5149605904824,-20.2370832183523,11.4402339014689));
#28531=CARTESIAN_POINT('Ctrl Pts',(5.56163184513152,-20.4071281981078,11.4175334462604));
#28532=CARTESIAN_POINT('Ctrl Pts',(5.59976054259138,-20.5790716204159,11.3988017977733));
#28533=CARTESIAN_POINT('Ctrl Pts',(5.60078189485067,-20.5836774636401,11.398300033675));
#28534=CARTESIAN_POINT('Ctrl Pts',(5.60179713081954,-20.588284691568,11.3978011111594));
#28535=CARTESIAN_POINT('Ctrl Pts',(5.6028062520001,-20.5928933047512,11.3973050368294));
#28536=CARTESIAN_POINT('Ctrl Pts',(5.66132456308721,-20.8601439235408,11.3685379942569));
#28537=CARTESIAN_POINT('Ctrl Pts',(5.69945338485962,-21.1320367632465,11.3493502464404));
#28538=CARTESIAN_POINT('Ctrl Pts',(5.71598745130091,-21.4089064857561,11.3409866054978));
#28539=CARTESIAN_POINT('Ctrl Pts',(5.72127276086345,-21.4974111616721,11.3383130689174));
#28540=CARTESIAN_POINT('Ctrl Pts',(5.72435111690867,-21.5864244670614,11.3367457922127));
#28541=CARTESIAN_POINT('Ctrl Pts',(5.72518221930917,-21.6759575456936,11.3363260607529));
#28542=CARTESIAN_POINT('',(-3.98168013490685E-8,-27.2249172597151,-12.6999510078656));
#28543=CARTESIAN_POINT('Origin',(-0.00396284819304756,-22.4165755189871,
-10.43604364865));
#28544=CARTESIAN_POINT('Ctrl Pts',(-1.7019301551402E-8,-27.2249172597024,
-12.6999510078581));
#28545=CARTESIAN_POINT('Ctrl Pts',(0.0919620281499745,-27.2248657333756,
-12.6999204986825));
#28546=CARTESIAN_POINT('Ctrl Pts',(0.184353662992845,-27.2226823876497,
-12.6988891026387));
#28547=CARTESIAN_POINT('Ctrl Pts',(0.276862348897653,-27.2183634804325,
-12.6968621751401));
#28548=CARTESIAN_POINT('Ctrl Pts',(0.462124174604044,-27.2097142533001,
-12.6928029639936));
#28549=CARTESIAN_POINT('Ctrl Pts',(0.647839459875023,-27.1925034530069,
-12.6847525512908));
#28550=CARTESIAN_POINT('Ctrl Pts',(0.831475394891656,-27.1666637039099,
-12.6727423017414));
#28551=CARTESIAN_POINT('Ctrl Pts',(0.860494367798756,-27.1625803910283,
-12.6708443883169));
#28552=CARTESIAN_POINT('Ctrl Pts',(0.889461358294665,-27.1582815166792,
-12.6688475550619));
#28553=CARTESIAN_POINT('Ctrl Pts',(0.918366295604896,-27.1537667230844,
-12.6667518858992));
#28554=CARTESIAN_POINT('Ctrl Pts',(0.98055647506929,-27.144052956163,-12.662242966197));
#28555=CARTESIAN_POINT('Ctrl Pts',(1.04239650412929,-27.1333908258806,-12.6573008409862));
#28556=CARTESIAN_POINT('Ctrl Pts',(1.10389408971677,-27.1217856443861,-12.6519371017105));
#28557=CARTESIAN_POINT('Ctrl Pts',(1.2625620332833,-27.0918434886922,-12.6380982904371));
#28558=CARTESIAN_POINT('Ctrl Pts',(1.41904274673861,-27.0556254034858,-12.6214427615578));
#28559=CARTESIAN_POINT('Ctrl Pts',(1.57325978677928,-27.0132680486838,-12.6021877405304));
#28560=CARTESIAN_POINT('Ctrl Pts',(1.72057085549696,-26.9728074925592,-12.5837949758593));
#28561=CARTESIAN_POINT('Ctrl Pts',(1.86581664047618,-26.9267456378757,-12.5630306730307));
#28562=CARTESIAN_POINT('Ctrl Pts',(2.00894530566494,-26.8752398114438,-12.5401012219179));
#28563=CARTESIAN_POINT('Ctrl Pts',(2.05715126527635,-26.8578925680705,-12.5323785467096));
#28564=CARTESIAN_POINT('Ctrl Pts',(2.10517405230903,-26.8398844404735,-12.524392320235));
#28565=CARTESIAN_POINT('Ctrl Pts',(2.15296898450167,-26.8212387765873,-12.5161611890146));
#28566=CARTESIAN_POINT('Ctrl Pts',(2.29352047974884,-26.7664071068085,-12.491955739869));
#28567=CARTESIAN_POINT('Ctrl Pts',(2.43251125386155,-26.7058815234932,-12.4655601671862));
#28568=CARTESIAN_POINT('Ctrl Pts',(2.5687690002987,-26.6401870104483,-12.4374255022749));
#28569=CARTESIAN_POINT('Ctrl Pts',(2.71342992195853,-26.5704410396425,-12.4075557395416));
#28570=CARTESIAN_POINT('Ctrl Pts',(2.85500904214592,-26.4948690946154,-12.3757261024131));
#28571=CARTESIAN_POINT('Ctrl Pts',(2.992100362019,-26.4141509519538,-12.3425004113455));
#28572=CARTESIAN_POINT('Ctrl Pts',(3.00032253918009,-26.4093098076006,-12.3405076701675));
#28573=CARTESIAN_POINT('Ctrl Pts',(3.00852857598774,-26.4044501657706,-12.3385099130153));
#28574=CARTESIAN_POINT('Ctrl Pts',(3.01671817046085,-26.3995721783131,-12.3365072636135));
#28575=CARTESIAN_POINT('Ctrl Pts',(3.05290384570193,-26.3780188192859,-12.3276585689542));
#28576=CARTESIAN_POINT('Ctrl Pts',(3.0888021169251,-26.3561051263587,-12.318712157291));
#28577=CARTESIAN_POINT('Ctrl Pts',(3.12441174007421,-26.333831450486,-12.309674813074));
#28578=CARTESIAN_POINT('Ctrl Pts',(3.34125762189574,-26.198195224688,-12.2546416309523));
#28579=CARTESIAN_POINT('Ctrl Pts',(3.54772308859836,-26.0490733658479,-12.1961505100754));
#28580=CARTESIAN_POINT('Ctrl Pts',(3.74391756194467,-25.8861282255617,-12.1356158763297));
#28581=CARTESIAN_POINT('Ctrl Pts',(3.79599109572935,-25.8428796614048,-12.1195488982863));
#28582=CARTESIAN_POINT('Ctrl Pts',(3.84734106675829,-25.7986573538643,-12.1033382387448));
#28583=CARTESIAN_POINT('Ctrl Pts',(3.89796951692403,-25.7534551371196,-12.087010947047));
#28584=CARTESIAN_POINT('Ctrl Pts',(3.92454494649468,-25.7297279970707,-12.0784405723036));
#28585=CARTESIAN_POINT('Ctrl Pts',(3.9509298956712,-25.7057129097212,-12.069833672881));
#28586=CARTESIAN_POINT('Ctrl Pts',(3.97710293758018,-25.6814305242753,-12.061202131027));
#28587=CARTESIAN_POINT('Ctrl Pts',(4.08451935206046,-25.5817735264872,-12.0257775410761));
#28588=CARTESIAN_POINT('Ctrl Pts',(4.18841193528078,-25.4775729320852,-11.9899221486096));
#28589=CARTESIAN_POINT('Ctrl Pts',(4.28726008864082,-25.3702924740377,-11.954472005567));
#28590=CARTESIAN_POINT('Ctrl Pts',(4.40974977111969,-25.2373537311704,-11.9105432459744));
#28591=CARTESIAN_POINT('Ctrl Pts',(4.5251682098118,-25.0991480820203,-11.867030450089));
#28592=CARTESIAN_POINT('Ctrl Pts',(4.6335846329197,-24.9556438900871,-11.8245462258172));
#28593=CARTESIAN_POINT('Ctrl Pts',(4.65262203277703,-24.9304452476239,-11.8170862013864));
#28594=CARTESIAN_POINT('Ctrl Pts',(4.67144842031647,-24.9050788727734,-11.8096560552095));
#28595=CARTESIAN_POINT('Ctrl Pts',(4.69006145813723,-24.8795447530719,-11.8022598374611));
#28596=CARTESIAN_POINT('Ctrl Pts',(4.7723035961848,-24.7667216546804,-11.7695794782985));
#28597=CARTESIAN_POINT('Ctrl Pts',(4.85034730639964,-24.650651948875,-11.7375752393652));
#28598=CARTESIAN_POINT('Ctrl Pts',(4.92411608245589,-24.5311963270221,-11.7065464803374));
#28599=CARTESIAN_POINT('Ctrl Pts',(4.94459812070782,-24.4980292508281,-11.6979312875242));
#28600=CARTESIAN_POINT('Ctrl Pts',(4.96475039072747,-24.4646009375596,-11.6893913462764));
#28601=CARTESIAN_POINT('Ctrl Pts',(4.98457075206297,-24.4309079012617,-11.6809332077249));
#28602=CARTESIAN_POINT('Ctrl Pts',(5.03933188484637,-24.3378183352667,-11.6575644486756));
#28603=CARTESIAN_POINT('Ctrl Pts',(5.09161161619109,-24.2425967726689,-11.6347969726201));
#28604=CARTESIAN_POINT('Ctrl Pts',(5.14119233544617,-24.1453998846143,-11.612845006953));
#28605=CARTESIAN_POINT('Ctrl Pts',(5.16010085472048,-24.1083320635178,-11.604473221062));
#28606=CARTESIAN_POINT('Ctrl Pts',(5.17861722716774,-24.0709772880951,-11.596219974711));
#28607=CARTESIAN_POINT('Ctrl Pts',(5.19673091228954,-24.0333455211125,-11.5880968161816));
#28608=CARTESIAN_POINT('Ctrl Pts',(5.21022735894756,-24.0053062164479,-11.5820442777252));
#28609=CARTESIAN_POINT('Ctrl Pts',(5.22346537779254,-23.9771875661639,-11.576080555973));
#28610=CARTESIAN_POINT('Ctrl Pts',(5.23644298045248,-23.9489937764396,-11.5702090530435));
#28611=CARTESIAN_POINT('Ctrl Pts',(5.34709859392846,-23.7085949000134,-11.5201447402644));
#28612=CARTESIAN_POINT('Ctrl Pts',(5.43928172673109,-23.4620964725225,-11.4765736062942));
#28613=CARTESIAN_POINT('Ctrl Pts',(5.51299566525125,-23.2092865166259,-11.4410293714832));
#28614=CARTESIAN_POINT('Ctrl Pts',(5.53168082450053,-23.1452037341757,-11.4320195464601));
#28615=CARTESIAN_POINT('Ctrl Pts',(5.54917921254299,-23.0807155378359,-11.4235256980846));
#28616=CARTESIAN_POINT('Ctrl Pts',(5.56549076766331,-23.0158187456202,-11.4155732451165));
#28617=CARTESIAN_POINT('Ctrl Pts',(5.57329864162245,-22.98475451108,-11.4117666337921));
#28618=CARTESIAN_POINT('Ctrl Pts',(5.58083243181111,-22.9535960971172,-11.4080840716811));
#28619=CARTESIAN_POINT('Ctrl Pts',(5.5880897436265,-22.9223425326086,-11.4045284354039));
#28620=CARTESIAN_POINT('Ctrl Pts',(5.62167888031574,-22.7776911414314,-11.3880718250264));
#28621=CARTESIAN_POINT('Ctrl Pts',(5.64935105012608,-22.6309587679954,-11.3743312617738));
#28622=CARTESIAN_POINT('Ctrl Pts',(5.67088043129442,-22.4821735999493,-11.3635872473284));
#28623=CARTESIAN_POINT('Ctrl Pts',(5.67570457147357,-22.4488349497754,-11.361179810191));
#28624=CARTESIAN_POINT('Ctrl Pts',(5.68021785890798,-22.4153642376299,-11.3589241136083));
#28625=CARTESIAN_POINT('Ctrl Pts',(5.68441662585656,-22.3817978431521,-11.3568229803739));
#28626=CARTESIAN_POINT('Ctrl Pts',(5.69835045506675,-22.2704059955969,-11.3498502590979));
#28627=CARTESIAN_POINT('Ctrl Pts',(5.70882198550556,-22.1578045395964,-11.3445789402659));
#28628=CARTESIAN_POINT('Ctrl Pts',(5.71566537362297,-22.0454619815195,-11.3411284191284));
#28629=CARTESIAN_POINT('Ctrl Pts',(5.71792815975813,-22.0083155887615,-11.3399874943036));
#28630=CARTESIAN_POINT('Ctrl Pts',(5.71979464301309,-21.9711976311711,-11.3390454595814));
#28631=CARTESIAN_POINT('Ctrl Pts',(5.72125994327243,-21.9341613129817,-11.3383060753985));
#28632=CARTESIAN_POINT('Ctrl Pts',(5.72265809038181,-21.8988223298017,-11.3376005764051));
#28633=CARTESIAN_POINT('Ctrl Pts',(5.72370246038071,-21.8635184569659,-11.337075434071));
#28634=CARTESIAN_POINT('Ctrl Pts',(5.72439386792677,-21.8282553410221,-11.336729461383));
#28635=CARTESIAN_POINT('Ctrl Pts',(5.72763135267748,-21.6631373859456,-11.3351094598252));
#28636=CARTESIAN_POINT('Ctrl Pts',(5.72315277323322,-21.4986115543393,-11.3374063209502));
#28637=CARTESIAN_POINT('Ctrl Pts',(5.71101505935482,-21.3347960248396,-11.3435120227631));
#28638=CARTESIAN_POINT('Ctrl Pts',(5.69891170879394,-21.1714442766673,-11.3496004386051));
#28639=CARTESIAN_POINT('Ctrl Pts',(5.67919259864153,-21.0087987989881,-11.3594760501232));
#28640=CARTESIAN_POINT('Ctrl Pts',(5.65196058833497,-20.8469737346032,-11.3730093420465));
#28641=CARTESIAN_POINT('Ctrl Pts',(5.64564096375417,-20.8094196340002,-11.3761499594059));
#28642=CARTESIAN_POINT('Ctrl Pts',(5.63889928922109,-20.7718633753357,-11.379494165011));
#28643=CARTESIAN_POINT('Ctrl Pts',(5.63174531056276,-20.7343459984228,-11.3830339551735));
#28644=CARTESIAN_POINT('Ctrl Pts',(5.61323924531877,-20.6372952441373,-11.3921907601945));
#28645=CARTESIAN_POINT('Ctrl Pts',(5.59191445744438,-20.5402412872527,-11.4026858495865));
#28646=CARTESIAN_POINT('Ctrl Pts',(5.56795652307117,-20.4440800872431,-11.4143716869199));
#28647=CARTESIAN_POINT('Ctrl Pts',(5.55687489104712,-20.3996011677796,-11.4197769170705));
#28648=CARTESIAN_POINT('Ctrl Pts',(5.54523057951688,-20.3553132317987,-11.4254365819491));
#28649=CARTESIAN_POINT('Ctrl Pts',(5.53304526406038,-20.3113039893352,-11.4313345723834));
#28650=CARTESIAN_POINT('Ctrl Pts',(5.52253653690031,-20.2733500173415,-11.436421053114));
#28651=CARTESIAN_POINT('Ctrl Pts',(5.51163177819215,-20.2355988095398,-11.4416817157982));
#28652=CARTESIAN_POINT('Ctrl Pts',(5.50033952748779,-20.198060350804,-11.4471079837937));
#28653=CARTESIAN_POINT('Ctrl Pts',(5.46317549856261,-20.0745171880821,-11.4649664237118));
#28654=CARTESIAN_POINT('Ctrl Pts',(5.42172773120231,-19.9529931589739,-11.4846598695274));
#28655=CARTESIAN_POINT('Ctrl Pts',(5.37619491489848,-19.8335655490195,-11.5059345966497));
#28656=CARTESIAN_POINT('Ctrl Pts',(5.37127472611302,-19.8206604305824,-11.5082335028518));
#28657=CARTESIAN_POINT('Ctrl Pts',(5.36630688151358,-19.8077797714875,-11.510550858192));
#28658=CARTESIAN_POINT('Ctrl Pts',(5.36129166305822,-19.7949236552371,-11.5128863323853));
#28659=CARTESIAN_POINT('Ctrl Pts',(5.34691188376625,-19.7580622271897,-11.519582671486));
#28660=CARTESIAN_POINT('Ctrl Pts',(5.33212860288283,-19.7213755536174,-11.5264349197701));
#28661=CARTESIAN_POINT('Ctrl Pts',(5.31695054271167,-19.6848766190699,-11.533433113328));
#28662=CARTESIAN_POINT('Ctrl Pts',(5.27638526845153,-19.5873286272035,-11.5521366655475));
#28663=CARTESIAN_POINT('Ctrl Pts',(5.23300493090568,-19.4911313617358,-11.5718807649671));
#28664=CARTESIAN_POINT('Ctrl Pts',(5.18683768202814,-19.3962495630333,-11.5925387023274));
#28665=CARTESIAN_POINT('Ctrl Pts',(5.1539521155395,-19.3286639525485,-11.6072536352961));
#28666=CARTESIAN_POINT('Ctrl Pts',(5.11965146781014,-19.2617460640714,-11.6224327042036));
#28667=CARTESIAN_POINT('Ctrl Pts',(5.0839318381286,-19.1954891982059,-11.6380349922324));
#28668=CARTESIAN_POINT('Ctrl Pts',(5.04090598405321,-19.115679909374,-11.6568286296232));
#28669=CARTESIAN_POINT('Ctrl Pts',(4.99577829317954,-19.0367621135859,-11.6762543884676));
#28670=CARTESIAN_POINT('Ctrl Pts',(4.94872505777747,-18.9590662319327,-11.6961606247422));
#28671=CARTESIAN_POINT('Ctrl Pts',(4.92227129859887,-18.9153848968479,-11.7073520927902));
#28672=CARTESIAN_POINT('Ctrl Pts',(4.89520974043141,-18.8720893817075,-11.7186951745409));
#28673=CARTESIAN_POINT('Ctrl Pts',(4.8675778112301,-18.8292348509718,-11.7301613905388));
#28674=CARTESIAN_POINT('Ctrl Pts',(4.84627354591299,-18.7961939334816,-11.739001862951));
#28675=CARTESIAN_POINT('Ctrl Pts',(4.82466820516189,-18.7634613348383,-11.7478998973589));
#28676=CARTESIAN_POINT('Ctrl Pts',(4.80277580072744,-18.7310503313297,-11.7568440949918));
#28677=CARTESIAN_POINT('Ctrl Pts',(4.69567916281518,-18.5724971894157,-11.8005986993878));
#28678=CARTESIAN_POINT('Ctrl Pts',(4.58107418642852,-18.4206274814446,-11.8457174546917));
#28679=CARTESIAN_POINT('Ctrl Pts',(4.45915446310147,-18.2752432087695,-11.8914321663685));
#28680=CARTESIAN_POINT('Ctrl Pts',(4.37478828667904,-18.1746400014881,-11.9230658949006));
#28681=CARTESIAN_POINT('Ctrl Pts',(4.28692040782722,-18.0771416225569,-11.9549851094832));
#28682=CARTESIAN_POINT('Ctrl Pts',(4.1956265966026,-17.9826746468627,-11.9869394509486));
#28683=CARTESIAN_POINT('Ctrl Pts',(4.17052053334575,-17.95669595416,-11.9957269876655));
#28684=CARTESIAN_POINT('Ctrl Pts',(4.14512819596976,-17.9309341256672,-12.004523640522));
#28685=CARTESIAN_POINT('Ctrl Pts',(4.11946314917148,-17.9053995464596,-12.0133206849436));
#28686=CARTESIAN_POINT('Ctrl Pts',(3.99766032356665,-17.7842159023165,-12.0550702627233));
#28687=CARTESIAN_POINT('Ctrl Pts',(3.86946339986725,-17.6679311930972,-12.0969136064702));
#28688=CARTESIAN_POINT('Ctrl Pts',(3.73626746162298,-17.557697063915,-12.1379220118173));
#28689=CARTESIAN_POINT('Ctrl Pts',(3.61575222290182,-17.4579575931118,-12.1750262795984));
#28690=CARTESIAN_POINT('Ctrl Pts',(3.49114538313714,-17.3631715319409,-12.2114466943468));
#28691=CARTESIAN_POINT('Ctrl Pts',(3.36348515525031,-17.2741576657265,-12.2465083840004));
#28692=CARTESIAN_POINT('Ctrl Pts',(3.33817437369643,-17.2565091736291,-12.2534599520998));
#28693=CARTESIAN_POINT('Ctrl Pts',(3.31273120437577,-17.2390694750856,-12.2603640039171));
#28694=CARTESIAN_POINT('Ctrl Pts',(3.28715560804173,-17.2218389907719,-12.2672180913233));
#28695=CARTESIAN_POINT('Ctrl Pts',(3.13817522652918,-17.1214697132324,-12.3071438292555));
#28696=CARTESIAN_POINT('Ctrl Pts',(2.98455940472934,-17.028087697893,-12.345410271681));
#28697=CARTESIAN_POINT('Ctrl Pts',(2.82627288516427,-16.9417913892476,-12.3815390224694));
#28698=CARTESIAN_POINT('Ctrl Pts',(2.68919781167141,-16.8670593597467,-12.4128262804313));
#28699=CARTESIAN_POINT('Ctrl Pts',(2.5486203623837,-16.7976406813461,-12.4425104528035));
#28700=CARTESIAN_POINT('Ctrl Pts',(2.40453611326549,-16.7335765984635,-12.4702929425024));
#28701=CARTESIAN_POINT('Ctrl Pts',(2.38315623382809,-16.7240704770333,-12.4744154353069));
#28702=CARTESIAN_POINT('Ctrl Pts',(2.36168266030452,-16.7146790116667,-12.4784979351355));
#28703=CARTESIAN_POINT('Ctrl Pts',(2.3401251353203,-16.7054060581952,-12.4825380108379));
#28704=CARTESIAN_POINT('Ctrl Pts',(2.22756904715961,-16.6569901398923,-12.5036320426096));
#28705=CARTESIAN_POINT('Ctrl Pts',(2.11250061650078,-16.6117209023858,-12.5236098153468));
#28706=CARTESIAN_POINT('Ctrl Pts',(1.99642655688378,-16.5702166143712,-12.5420945500035));
#28707=CARTESIAN_POINT('Ctrl Pts',(1.95758723480752,-16.5563289428702,-12.5482796921893));
#28708=CARTESIAN_POINT('Ctrl Pts',(1.91863542297512,-16.5428624279043,-12.5542978218573));
#28709=CARTESIAN_POINT('Ctrl Pts',(1.87962761015771,-16.5298389828478,-12.5601353514636));
#28710=CARTESIAN_POINT('Ctrl Pts',(1.8619346620097,-16.5239318806175,-12.5627831058794));
#28711=CARTESIAN_POINT('Ctrl Pts',(1.84422418636504,-16.5181122065921,-12.5653952768144));
#28712=CARTESIAN_POINT('Ctrl Pts',(1.82649684649618,-16.5123799001449,-12.5679716062491));
#28713=CARTESIAN_POINT('Ctrl Pts',(1.66534273955609,-16.4602691642401,-12.5913922701672));
#28714=CARTESIAN_POINT('Ctrl Pts',(1.50261810408699,-16.4153143921165,-12.611876524808));
#28715=CARTESIAN_POINT('Ctrl Pts',(1.3383391466942,-16.3773802058618,-12.6292853450775));
#28716=CARTESIAN_POINT('Ctrl Pts',(1.32563644048517,-16.374446982819,-12.6306314647075));
#28717=CARTESIAN_POINT('Ctrl Pts',(1.31292448911361,-16.3715553979143,-12.6319592494833));
#28718=CARTESIAN_POINT('Ctrl Pts',(1.30020327362486,-16.3687055245917,-12.6332686220619));
#28719=CARTESIAN_POINT('Ctrl Pts',(1.01314339992633,-16.3043968681773,-12.6628151954506));
#28720=CARTESIAN_POINT('Ctrl Pts',(0.721379562021647,-16.2612760127206,
-12.68298231415));
#28721=CARTESIAN_POINT('Ctrl Pts',(0.42469199194604,-16.2401281321735,-12.6929008886698));
#28722=CARTESIAN_POINT('Ctrl Pts',(0.355011601791331,-16.2351613161822,
-12.695230376697));
#28723=CARTESIAN_POINT('Ctrl Pts',(0.285059746695848,-16.2314063896488,
-12.6969946851133));
#28724=CARTESIAN_POINT('Ctrl Pts',(0.214833815848646,-16.2288732699618,
-12.6981828003682));
#28725=CARTESIAN_POINT('Origin',(0.,-44.45,12.7));
#28726=CARTESIAN_POINT('Origin',(0.,-47.63,7.70000000000001));
#28727=CARTESIAN_POINT('',(2.55537495509676,-47.63,-8.00360031633711));
#28728=CARTESIAN_POINT('',(-7.96780251527898,-47.63,-2.66489817109789));
#28729=CARTESIAN_POINT('Ctrl Pts',(2.55537495509679,-47.63,-8.0036003163371));
#28730=CARTESIAN_POINT('Ctrl Pts',(1.86263429679466,-47.63,-8.16654376028585));
#28731=CARTESIAN_POINT('Ctrl Pts',(0.765908078329645,-47.63,-8.37785612188963));
#28732=CARTESIAN_POINT('Ctrl Pts',(-1.6692617677719,-47.63,-8.16209001543163));
#28733=CARTESIAN_POINT('Ctrl Pts',(-2.74375110300835,-47.63,-7.85437659041765));
#28734=CARTESIAN_POINT('Ctrl Pts',(-4.69944968573892,-47.63,-6.8614528643732));
#28735=CARTESIAN_POINT('Ctrl Pts',(-5.56511466324777,-47.63,-6.19428529183315));
#28736=CARTESIAN_POINT('Ctrl Pts',(-7.19394906010722,-47.63,-4.37070183094962));
#28737=CARTESIAN_POINT('Ctrl Pts',(-7.67609992676134,-47.63,-3.3577148847143));
#28738=CARTESIAN_POINT('Ctrl Pts',(-7.96780251527896,-47.63,-2.66489817109788));
#28739=CARTESIAN_POINT('',(4.50738083181344,-47.63,8.84193633985987));
#28740=CARTESIAN_POINT('Ctrl Pts',(-7.96780251527901,-47.63,-2.66489817109774));
#28741=CARTESIAN_POINT('Ctrl Pts',(-8.23599312974433,-47.63,-2.027924255025));
#28742=CARTESIAN_POINT('Ctrl Pts',(-8.42634396183627,-47.63,-1.36096366704783));
#28743=CARTESIAN_POINT('Ctrl Pts',(-8.64297828766043,-47.63,0.00360816572509623));
#28744=CARTESIAN_POINT('Ctrl Pts',(-8.66859900866028,-47.63,0.696135165601388));
#28745=CARTESIAN_POINT('Ctrl Pts',(-8.52525050570627,-47.63,2.41043360782728));
#28746=CARTESIAN_POINT('Ctrl Pts',(-8.25568996932099,-47.6300000000836,
3.41277917262432));
#28747=CARTESIAN_POINT('Ctrl Pts',(-7.37169226325108,-47.6300000000836,
5.28253364315782));
#28748=CARTESIAN_POINT('Ctrl Pts',(-6.69159903012225,-47.6300000000001,
6.31291964415818));
#28749=CARTESIAN_POINT('Ctrl Pts',(-4.74829296569675,-47.6300000000001,
8.0685409876383));
#28750=CARTESIAN_POINT('Ctrl Pts',(-3.68909457138915,-47.63,8.69991320242805));
#28751=CARTESIAN_POINT('Ctrl Pts',(-1.08588604418679,-47.63,9.62226726459695));
#28752=CARTESIAN_POINT('Ctrl Pts',(0.195202339559025,-47.63,9.67166205579392));
#28753=CARTESIAN_POINT('Ctrl Pts',(2.25253429025304,-47.63,9.57488020226805));
#28754=CARTESIAN_POINT('Ctrl Pts',(3.41720895858092,-47.63,9.30785410203652));
#28755=CARTESIAN_POINT('Ctrl Pts',(4.50738083181199,-47.63,8.84193633986041));
#28756=CARTESIAN_POINT('Ctrl Pts',(4.50738083181341,-47.63,8.84193633985991));
#28757=CARTESIAN_POINT('Ctrl Pts',(5.50129019941108,-47.63,8.24752673459283));
#28758=CARTESIAN_POINT('Ctrl Pts',(6.3827306396232,-47.63,7.48282682306558));
#28759=CARTESIAN_POINT('Ctrl Pts',(7.7290655812775,-47.63,5.82007728703929));
#28760=CARTESIAN_POINT('Ctrl Pts',(8.42964347032193,-47.6300000000064,4.72920057212086));
#28761=CARTESIAN_POINT('Ctrl Pts',(9.20437486461963,-47.6300000000064,2.13877895901777));
#28762=CARTESIAN_POINT('Ctrl Pts',(9.31838831238719,-47.63,0.915490022080004));
#28763=CARTESIAN_POINT('Ctrl Pts',(9.06300659638666,-47.63,-1.5079931069641));
#28764=CARTESIAN_POINT('Ctrl Pts',(8.69486484793724,-47.63,-2.68367031517789));
#28765=CARTESIAN_POINT('Ctrl Pts',(7.55278087878427,-47.63,-4.7656464219269));
#28766=CARTESIAN_POINT('Ctrl Pts',(6.81838193887884,-47.630000000013,-5.6526889049818));
#28767=CARTESIAN_POINT('Ctrl Pts',(5.41795245135679,-47.630000000013,-6.76839622139177));
#28768=CARTESIAN_POINT('Ctrl Pts',(4.87996243897364,-47.6300000023591,-7.10670058837738));
#28769=CARTESIAN_POINT('Ctrl Pts',(3.74918166874711,-47.6300000023591,-7.6527881999309));
#28770=CARTESIAN_POINT('Ctrl Pts',(3.16100732091453,-47.63,-7.86114610599088));
#28771=CARTESIAN_POINT('Ctrl Pts',(2.55537495509679,-47.63,-8.00360031633713));
#28772=CARTESIAN_POINT('Ctrl Pts',(-1.78726082715848E-11,-214.73675111262,
-9.92453123331945));
#28773=CARTESIAN_POINT('Ctrl Pts',(-5.7299307791557,-214.56175111262,-9.92453123330913));
#28774=CARTESIAN_POINT('Ctrl Pts',(-8.59489616871569,-214.38675111262,-4.96226561664425));
#28775=CARTESIAN_POINT('Ctrl Pts',(-11.4598615582757,-214.21175111262,2.06368086793017E-11));
#28776=CARTESIAN_POINT('Ctrl Pts',(-8.59489616869782,-214.03675111262,4.9622656166752));
#28777=CARTESIAN_POINT('Ctrl Pts',(-5.72993077911996,-213.86175111262,9.92453123332977));
#28778=CARTESIAN_POINT('Ctrl Pts',(1.7871392867044E-11,-213.68675111262,
9.92453123331945));
#28779=CARTESIAN_POINT('Ctrl Pts',(5.7299307791557,-213.51175111262,9.92453123330913));
#28780=CARTESIAN_POINT('Ctrl Pts',(8.59489616871569,-213.33675111262,4.96226561664425));
#28781=CARTESIAN_POINT('Ctrl Pts',(11.4598615582757,-213.16175111262,-2.06354052510241E-11));
#28782=CARTESIAN_POINT('Ctrl Pts',(8.59489616869782,-212.98675111262,-4.9622656166752));
#28783=CARTESIAN_POINT('Ctrl Pts',(5.72993077911996,-212.81175111262,-9.92453123332976));
#28784=CARTESIAN_POINT('Ctrl Pts',(-1.78726082715848E-11,-212.63675111262,
-9.92453123331945));
#28785=CARTESIAN_POINT('Ctrl Pts',(-5.7299307791557,-212.46175111262,-9.92453123330913));
#28786=CARTESIAN_POINT('Ctrl Pts',(-8.59489616871569,-212.28675111262,-4.96226561664425));
#28787=CARTESIAN_POINT('Ctrl Pts',(-11.4598615582757,-212.11175111262,2.06368086793017E-11));
#28788=CARTESIAN_POINT('Ctrl Pts',(-8.59489616869782,-211.93675111262,4.9622656166752));
#28789=CARTESIAN_POINT('Ctrl Pts',(-5.72993077911996,-211.76175111262,9.92453123332977));
#28790=CARTESIAN_POINT('Ctrl Pts',(1.7871392867044E-11,-211.58675111262,
9.92453123331945));
#28791=CARTESIAN_POINT('Ctrl Pts',(5.7299307791557,-211.41175111262,9.92453123330913));
#28792=CARTESIAN_POINT('Ctrl Pts',(8.59489616871569,-211.23675111262,4.96226561664425));
#28793=CARTESIAN_POINT('Ctrl Pts',(11.4598615582757,-211.06175111262,-2.06354052510241E-11));
#28794=CARTESIAN_POINT('Ctrl Pts',(8.59489616869782,-210.88675111262,-4.9622656166752));
#28795=CARTESIAN_POINT('Ctrl Pts',(5.72993077911996,-210.71175111262,-9.92453123332976));
#28796=CARTESIAN_POINT('Ctrl Pts',(-1.78726082715848E-11,-210.53675111262,
-9.92453123331945));
#28797=CARTESIAN_POINT('Ctrl Pts',(-5.7299307791557,-210.36175111262,-9.92453123330913));
#28798=CARTESIAN_POINT('Ctrl Pts',(-8.59489616871569,-210.18675111262,-4.96226561664425));
#28799=CARTESIAN_POINT('Ctrl Pts',(-11.4598615582757,-210.01175111262,2.06368086793017E-11));
#28800=CARTESIAN_POINT('Ctrl Pts',(-8.59489616869782,-209.83675111262,4.9622656166752));
#28801=CARTESIAN_POINT('Ctrl Pts',(-5.72993077911996,-209.66175111262,9.92453123332977));
#28802=CARTESIAN_POINT('Ctrl Pts',(1.7871392867044E-11,-209.48675111262,
9.92453123331945));
#28803=CARTESIAN_POINT('Ctrl Pts',(5.7299307791557,-209.31175111262,9.92453123330913));
#28804=CARTESIAN_POINT('Ctrl Pts',(8.59489616871569,-209.13675111262,4.96226561664425));
#28805=CARTESIAN_POINT('Ctrl Pts',(11.4598615582757,-208.96175111262,-2.06354052510241E-11));
#28806=CARTESIAN_POINT('Ctrl Pts',(8.59489616869782,-208.78675111262,-4.9622656166752));
#28807=CARTESIAN_POINT('Ctrl Pts',(5.72993077911996,-208.61175111262,-9.92453123332976));
#28808=CARTESIAN_POINT('Ctrl Pts',(-1.78726082715848E-11,-208.43675111262,
-9.92453123331945));
#28809=CARTESIAN_POINT('Ctrl Pts',(-5.7299307791557,-208.26175111262,-9.92453123330913));
#28810=CARTESIAN_POINT('Ctrl Pts',(-8.59489616871569,-208.08675111262,-4.96226561664425));
#28811=CARTESIAN_POINT('Ctrl Pts',(-11.4598615582757,-207.91175111262,2.06368086793017E-11));
#28812=CARTESIAN_POINT('Ctrl Pts',(-8.59489616869782,-207.73675111262,4.9622656166752));
#28813=CARTESIAN_POINT('Ctrl Pts',(-5.72993077911996,-207.56175111262,9.92453123332977));
#28814=CARTESIAN_POINT('Ctrl Pts',(1.7871392867044E-11,-207.38675111262,
9.92453123331945));
#28815=CARTESIAN_POINT('Ctrl Pts',(5.7299307791557,-207.21175111262,9.92453123330913));
#28816=CARTESIAN_POINT('Ctrl Pts',(8.59489616871569,-207.03675111262,4.96226561664425));
#28817=CARTESIAN_POINT('Ctrl Pts',(11.4598615582757,-206.86175111262,-2.06354052510241E-11));
#28818=CARTESIAN_POINT('Ctrl Pts',(8.59489616869782,-206.68675111262,-4.9622656166752));
#28819=CARTESIAN_POINT('Ctrl Pts',(5.72993077911996,-206.51175111262,-9.92453123332976));
#28820=CARTESIAN_POINT('Ctrl Pts',(-1.78726082715848E-11,-206.33675111262,
-9.92453123331945));
#28821=CARTESIAN_POINT('Ctrl Pts',(-5.7299307791557,-206.16175111262,-9.92453123330913));
#28822=CARTESIAN_POINT('Ctrl Pts',(-8.59489616871569,-205.98675111262,-4.96226561664425));
#28823=CARTESIAN_POINT('Ctrl Pts',(-11.4598615582757,-205.81175111262,2.06368086793017E-11));
#28824=CARTESIAN_POINT('Ctrl Pts',(-8.59489616869782,-205.63675111262,4.9622656166752));
#28825=CARTESIAN_POINT('Ctrl Pts',(-5.72993077911996,-205.46175111262,9.92453123332977));
#28826=CARTESIAN_POINT('Ctrl Pts',(1.7871392867044E-11,-205.28675111262,
9.92453123331945));
#28827=CARTESIAN_POINT('Ctrl Pts',(5.7299307791557,-205.11175111262,9.92453123330913));
#28828=CARTESIAN_POINT('Ctrl Pts',(8.59489616871569,-204.93675111262,4.96226561664425));
#28829=CARTESIAN_POINT('Ctrl Pts',(11.4598615582757,-204.76175111262,-2.06354052510241E-11));
#28830=CARTESIAN_POINT('Ctrl Pts',(8.59489616869782,-204.58675111262,-4.9622656166752));
#28831=CARTESIAN_POINT('Ctrl Pts',(5.72993077911996,-204.41175111262,-9.92453123332976));
#28832=CARTESIAN_POINT('Ctrl Pts',(-1.78726082715848E-11,-204.23675111262,
-9.92453123331945));
#28833=CARTESIAN_POINT('Ctrl Pts',(-5.7299307791557,-204.06175111262,-9.92453123330913));
#28834=CARTESIAN_POINT('Ctrl Pts',(-8.59489616871569,-203.88675111262,-4.96226561664425));
#28835=CARTESIAN_POINT('Ctrl Pts',(-11.4598615582757,-203.71175111262,2.06368086793017E-11));
#28836=CARTESIAN_POINT('Ctrl Pts',(-8.59489616869782,-203.53675111262,4.9622656166752));
#28837=CARTESIAN_POINT('Ctrl Pts',(-5.72993077911996,-203.36175111262,9.92453123332977));
#28838=CARTESIAN_POINT('Ctrl Pts',(1.7871392867044E-11,-203.18675111262,
9.92453123331945));
#28839=CARTESIAN_POINT('Ctrl Pts',(5.7299307791557,-203.01175111262,9.92453123330913));
#28840=CARTESIAN_POINT('Ctrl Pts',(8.59489616871569,-202.83675111262,4.96226561664425));
#28841=CARTESIAN_POINT('Ctrl Pts',(11.4598615582757,-202.66175111262,-2.06354052510241E-11));
#28842=CARTESIAN_POINT('Ctrl Pts',(8.59489616869782,-202.48675111262,-4.9622656166752));
#28843=CARTESIAN_POINT('Ctrl Pts',(5.72993077911996,-202.31175111262,-9.92453123332976));
#28844=CARTESIAN_POINT('Ctrl Pts',(-1.78726082715848E-11,-202.13675111262,
-9.92453123331945));
#28845=CARTESIAN_POINT('Ctrl Pts',(-5.7299307791557,-201.96175111262,-9.92453123330913));
#28846=CARTESIAN_POINT('Ctrl Pts',(-8.59489616871569,-201.78675111262,-4.96226561664425));
#28847=CARTESIAN_POINT('Ctrl Pts',(-11.4598615582757,-201.61175111262,2.06368086793017E-11));
#28848=CARTESIAN_POINT('Ctrl Pts',(-8.59489616869782,-201.43675111262,4.9622656166752));
#28849=CARTESIAN_POINT('Ctrl Pts',(-5.72993077911996,-201.26175111262,9.92453123332977));
#28850=CARTESIAN_POINT('Ctrl Pts',(1.7871392867044E-11,-201.08675111262,
9.92453123331945));
#28851=CARTESIAN_POINT('Ctrl Pts',(5.7299307791557,-200.91175111262,9.92453123330913));
#28852=CARTESIAN_POINT('Ctrl Pts',(8.59489616871569,-200.73675111262,4.96226561664425));
#28853=CARTESIAN_POINT('Ctrl Pts',(11.4598615582757,-200.56175111262,-2.06354052510241E-11));
#28854=CARTESIAN_POINT('Ctrl Pts',(8.59489616869782,-200.38675111262,-4.9622656166752));
#28855=CARTESIAN_POINT('Ctrl Pts',(5.72993077911996,-200.21175111262,-9.92453123332976));
#28856=CARTESIAN_POINT('Ctrl Pts',(-1.78726082715848E-11,-200.03675111262,
-9.92453123331945));
#28857=CARTESIAN_POINT('Ctrl Pts',(-5.7299307791557,-199.86175111262,-9.92453123330913));
#28858=CARTESIAN_POINT('Ctrl Pts',(-8.59489616871569,-199.68675111262,-4.96226561664425));
#28859=CARTESIAN_POINT('Ctrl Pts',(-11.4598615582757,-199.51175111262,2.06368086793017E-11));
#28860=CARTESIAN_POINT('Ctrl Pts',(-8.59489616869782,-199.33675111262,4.9622656166752));
#28861=CARTESIAN_POINT('Ctrl Pts',(-5.72993077911996,-199.16175111262,9.92453123332977));
#28862=CARTESIAN_POINT('Ctrl Pts',(1.7871392867044E-11,-198.98675111262,
9.92453123331945));
#28863=CARTESIAN_POINT('Ctrl Pts',(5.7299307791557,-198.81175111262,9.92453123330913));
#28864=CARTESIAN_POINT('Ctrl Pts',(8.59489616871569,-198.63675111262,4.96226561664425));
#28865=CARTESIAN_POINT('Ctrl Pts',(11.4598615582757,-198.46175111262,-2.06354052510241E-11));
#28866=CARTESIAN_POINT('Ctrl Pts',(8.59489616869782,-198.28675111262,-4.9622656166752));
#28867=CARTESIAN_POINT('Ctrl Pts',(5.72993077911996,-198.11175111262,-9.92453123332976));
#28868=CARTESIAN_POINT('Ctrl Pts',(-1.78726082715848E-11,-197.93675111262,
-9.92453123331945));
#28869=CARTESIAN_POINT('Ctrl Pts',(-5.7299307791557,-197.76175111262,-9.92453123330913));
#28870=CARTESIAN_POINT('Ctrl Pts',(-8.59489616871569,-197.58675111262,-4.96226561664425));
#28871=CARTESIAN_POINT('Ctrl Pts',(-11.4598615582757,-197.41175111262,2.06368086793017E-11));
#28872=CARTESIAN_POINT('Ctrl Pts',(-8.59489616869782,-197.23675111262,4.9622656166752));
#28873=CARTESIAN_POINT('Ctrl Pts',(-5.72993077911996,-197.06175111262,9.92453123332977));
#28874=CARTESIAN_POINT('Ctrl Pts',(1.7871392867044E-11,-196.88675111262,
9.92453123331945));
#28875=CARTESIAN_POINT('Ctrl Pts',(5.7299307791557,-196.71175111262,9.92453123330913));
#28876=CARTESIAN_POINT('Ctrl Pts',(8.59489616871569,-196.53675111262,4.96226561664425));
#28877=CARTESIAN_POINT('Ctrl Pts',(11.4598615582757,-196.36175111262,-2.06354052510241E-11));
#28878=CARTESIAN_POINT('Ctrl Pts',(8.59489616869782,-196.18675111262,-4.9622656166752));
#28879=CARTESIAN_POINT('Ctrl Pts',(5.72993077911996,-196.01175111262,-9.92453123332976));
#28880=CARTESIAN_POINT('Ctrl Pts',(-1.78726082715848E-11,-195.83675111262,
-9.92453123331945));
#28881=CARTESIAN_POINT('Ctrl Pts',(-5.7299307791557,-195.66175111262,-9.92453123330913));
#28882=CARTESIAN_POINT('Ctrl Pts',(-8.59489616871569,-195.48675111262,-4.96226561664425));
#28883=CARTESIAN_POINT('Ctrl Pts',(-11.4598615582757,-195.31175111262,2.06368086793017E-11));
#28884=CARTESIAN_POINT('Ctrl Pts',(-8.59489616869782,-195.13675111262,4.9622656166752));
#28885=CARTESIAN_POINT('Ctrl Pts',(-5.72993077911996,-194.96175111262,9.92453123332977));
#28886=CARTESIAN_POINT('Ctrl Pts',(1.7871392867044E-11,-194.78675111262,
9.92453123331945));
#28887=CARTESIAN_POINT('Ctrl Pts',(5.7299307791557,-194.61175111262,9.92453123330913));
#28888=CARTESIAN_POINT('Ctrl Pts',(8.59489616871569,-194.43675111262,4.96226561664425));
#28889=CARTESIAN_POINT('Ctrl Pts',(11.4598615582757,-194.26175111262,-2.06354052510241E-11));
#28890=CARTESIAN_POINT('Ctrl Pts',(8.59489616869782,-194.08675111262,-4.9622656166752));
#28891=CARTESIAN_POINT('Ctrl Pts',(5.72993077911996,-193.91175111262,-9.92453123332976));
#28892=CARTESIAN_POINT('Ctrl Pts',(-1.78726082715848E-11,-193.73675111262,
-9.92453123331945));
#28893=CARTESIAN_POINT('Ctrl Pts',(-5.7299307791557,-193.56175111262,-9.92453123330913));
#28894=CARTESIAN_POINT('Ctrl Pts',(-8.59489616871569,-193.38675111262,-4.96226561664425));
#28895=CARTESIAN_POINT('Ctrl Pts',(-11.4598615582757,-193.21175111262,2.06368086793017E-11));
#28896=CARTESIAN_POINT('Ctrl Pts',(-8.59489616869782,-193.03675111262,4.9622656166752));
#28897=CARTESIAN_POINT('Ctrl Pts',(-5.72993077911996,-192.86175111262,9.92453123332977));
#28898=CARTESIAN_POINT('Ctrl Pts',(1.7871392867044E-11,-192.68675111262,
9.92453123331945));
#28899=CARTESIAN_POINT('Ctrl Pts',(5.7299307791557,-192.51175111262,9.92453123330913));
#28900=CARTESIAN_POINT('Ctrl Pts',(8.59489616871569,-192.33675111262,4.96226561664425));
#28901=CARTESIAN_POINT('Ctrl Pts',(11.4598615582757,-192.16175111262,-2.06354052510241E-11));
#28902=CARTESIAN_POINT('Ctrl Pts',(8.59489616869782,-191.98675111262,-4.9622656166752));
#28903=CARTESIAN_POINT('Ctrl Pts',(5.72993077911996,-191.81175111262,-9.92453123332976));
#28904=CARTESIAN_POINT('Ctrl Pts',(-1.78726082715848E-11,-191.63675111262,
-9.92453123331945));
#28905=CARTESIAN_POINT('Ctrl Pts',(-5.7299307791557,-191.46175111262,-9.92453123330913));
#28906=CARTESIAN_POINT('Ctrl Pts',(-8.59489616871569,-191.28675111262,-4.96226561664425));
#28907=CARTESIAN_POINT('Ctrl Pts',(-11.4598615582757,-191.11175111262,2.06368086793017E-11));
#28908=CARTESIAN_POINT('Ctrl Pts',(-8.59489616869782,-190.93675111262,4.9622656166752));
#28909=CARTESIAN_POINT('Ctrl Pts',(-5.72993077911996,-190.76175111262,9.92453123332977));
#28910=CARTESIAN_POINT('Ctrl Pts',(1.7871392867044E-11,-190.58675111262,
9.92453123331945));
#28911=CARTESIAN_POINT('Ctrl Pts',(5.7299307791557,-190.41175111262,9.92453123330913));
#28912=CARTESIAN_POINT('Ctrl Pts',(8.59489616871569,-190.23675111262,4.96226561664425));
#28913=CARTESIAN_POINT('Ctrl Pts',(11.4598615582757,-190.06175111262,-2.06354052510241E-11));
#28914=CARTESIAN_POINT('Ctrl Pts',(8.59489616869782,-189.88675111262,-4.9622656166752));
#28915=CARTESIAN_POINT('Ctrl Pts',(5.72993077911996,-189.71175111262,-9.92453123332976));
#28916=CARTESIAN_POINT('Ctrl Pts',(-1.78726082715848E-11,-189.53675111262,
-9.92453123331945));
#28917=CARTESIAN_POINT('Ctrl Pts',(-5.7299307791557,-189.36175111262,-9.92453123330913));
#28918=CARTESIAN_POINT('Ctrl Pts',(-8.59489616871569,-189.18675111262,-4.96226561664425));
#28919=CARTESIAN_POINT('Ctrl Pts',(-11.4598615582757,-189.01175111262,2.06368086793017E-11));
#28920=CARTESIAN_POINT('Ctrl Pts',(-8.59489616869782,-188.83675111262,4.9622656166752));
#28921=CARTESIAN_POINT('Ctrl Pts',(-5.72993077911996,-188.66175111262,9.92453123332977));
#28922=CARTESIAN_POINT('Ctrl Pts',(1.7871392867044E-11,-188.48675111262,
9.92453123331945));
#28923=CARTESIAN_POINT('Ctrl Pts',(5.7299307791557,-188.31175111262,9.92453123330913));
#28924=CARTESIAN_POINT('Ctrl Pts',(8.59489616871569,-188.13675111262,4.96226561664425));
#28925=CARTESIAN_POINT('Ctrl Pts',(11.4598615582757,-187.96175111262,-2.06354052510241E-11));
#28926=CARTESIAN_POINT('Ctrl Pts',(8.59489616869782,-187.78675111262,-4.9622656166752));
#28927=CARTESIAN_POINT('Ctrl Pts',(5.72993077911996,-187.61175111262,-9.92453123332976));
#28928=CARTESIAN_POINT('Ctrl Pts',(-1.78726082715848E-11,-187.43675111262,
-9.92453123331945));
#28929=CARTESIAN_POINT('Ctrl Pts',(-5.7299307791557,-187.26175111262,-9.92453123330913));
#28930=CARTESIAN_POINT('Ctrl Pts',(-8.59489616871569,-187.08675111262,-4.96226561664425));
#28931=CARTESIAN_POINT('Ctrl Pts',(-11.4598615582757,-186.91175111262,2.06368086793017E-11));
#28932=CARTESIAN_POINT('Ctrl Pts',(-8.59489616869782,-186.73675111262,4.9622656166752));
#28933=CARTESIAN_POINT('Ctrl Pts',(-5.72993077911996,-186.56175111262,9.92453123332977));
#28934=CARTESIAN_POINT('Ctrl Pts',(1.7871392867044E-11,-186.38675111262,
9.92453123331945));
#28935=CARTESIAN_POINT('Ctrl Pts',(5.7299307791557,-186.21175111262,9.92453123330913));
#28936=CARTESIAN_POINT('Ctrl Pts',(8.59489616871569,-186.03675111262,4.96226561664425));
#28937=CARTESIAN_POINT('Ctrl Pts',(11.4598615582757,-185.86175111262,-2.06354052510241E-11));
#28938=CARTESIAN_POINT('Ctrl Pts',(8.59489616869782,-185.68675111262,-4.9622656166752));
#28939=CARTESIAN_POINT('Ctrl Pts',(5.72993077911996,-185.51175111262,-9.92453123332976));
#28940=CARTESIAN_POINT('Ctrl Pts',(-1.78726082715848E-11,-185.33675111262,
-9.92453123331945));
#28941=CARTESIAN_POINT('Ctrl Pts',(-5.7299307791557,-185.16175111262,-9.92453123330913));
#28942=CARTESIAN_POINT('Ctrl Pts',(-8.59489616871569,-184.98675111262,-4.96226561664425));
#28943=CARTESIAN_POINT('Ctrl Pts',(-11.4598615582757,-184.81175111262,2.06368086793017E-11));
#28944=CARTESIAN_POINT('Ctrl Pts',(-8.59489616869782,-184.63675111262,4.9622656166752));
#28945=CARTESIAN_POINT('Ctrl Pts',(-5.72993077911996,-184.46175111262,9.92453123332977));
#28946=CARTESIAN_POINT('Ctrl Pts',(1.7871392867044E-11,-184.28675111262,
9.92453123331945));
#28947=CARTESIAN_POINT('Ctrl Pts',(5.7299307791557,-184.11175111262,9.92453123330913));
#28948=CARTESIAN_POINT('Ctrl Pts',(8.59489616871569,-183.93675111262,4.96226561664425));
#28949=CARTESIAN_POINT('Ctrl Pts',(11.4598615582757,-183.76175111262,-2.06354052510241E-11));
#28950=CARTESIAN_POINT('Ctrl Pts',(8.59489616869782,-183.58675111262,-4.9622656166752));
#28951=CARTESIAN_POINT('Ctrl Pts',(5.72993077911996,-183.41175111262,-9.92453123332976));
#28952=CARTESIAN_POINT('Ctrl Pts',(-1.78726082715848E-11,-183.23675111262,
-9.92453123331945));
#28953=CARTESIAN_POINT('Ctrl Pts',(-5.7299307791557,-183.06175111262,-9.92453123330913));
#28954=CARTESIAN_POINT('Ctrl Pts',(-8.59489616871569,-182.88675111262,-4.96226561664425));
#28955=CARTESIAN_POINT('Ctrl Pts',(-11.4598615582757,-182.71175111262,2.06368086793017E-11));
#28956=CARTESIAN_POINT('Ctrl Pts',(-8.59489616869782,-182.53675111262,4.9622656166752));
#28957=CARTESIAN_POINT('Ctrl Pts',(-5.72993077911996,-182.36175111262,9.92453123332977));
#28958=CARTESIAN_POINT('Ctrl Pts',(1.7871392867044E-11,-182.18675111262,
9.92453123331945));
#28959=CARTESIAN_POINT('Ctrl Pts',(5.7299307791557,-182.01175111262,9.92453123330913));
#28960=CARTESIAN_POINT('Ctrl Pts',(8.59489616871569,-181.83675111262,4.96226561664425));
#28961=CARTESIAN_POINT('Ctrl Pts',(11.4598615582757,-181.66175111262,-2.06354052510241E-11));
#28962=CARTESIAN_POINT('Ctrl Pts',(8.59489616869782,-181.48675111262,-4.9622656166752));
#28963=CARTESIAN_POINT('Ctrl Pts',(5.72993077911996,-181.31175111262,-9.92453123332976));
#28964=CARTESIAN_POINT('Ctrl Pts',(-1.78726082715848E-11,-181.13675111262,
-9.92453123331945));
#28965=CARTESIAN_POINT('Ctrl Pts',(-5.7299307791557,-180.96175111262,-9.92453123330913));
#28966=CARTESIAN_POINT('Ctrl Pts',(-8.59489616871569,-180.78675111262,-4.96226561664425));
#28967=CARTESIAN_POINT('Ctrl Pts',(-11.4598615582757,-180.61175111262,2.06368086793017E-11));
#28968=CARTESIAN_POINT('Ctrl Pts',(-8.59489616869782,-180.43675111262,4.9622656166752));
#28969=CARTESIAN_POINT('Ctrl Pts',(-5.72993077911996,-180.26175111262,9.92453123332977));
#28970=CARTESIAN_POINT('Ctrl Pts',(1.7871392867044E-11,-180.08675111262,
9.92453123331945));
#28971=CARTESIAN_POINT('Ctrl Pts',(5.7299307791557,-179.91175111262,9.92453123330913));
#28972=CARTESIAN_POINT('Ctrl Pts',(8.59489616871569,-179.73675111262,4.96226561664425));
#28973=CARTESIAN_POINT('Ctrl Pts',(11.4598615582757,-179.56175111262,-2.06354052510241E-11));
#28974=CARTESIAN_POINT('Ctrl Pts',(8.59489616869782,-179.38675111262,-4.9622656166752));
#28975=CARTESIAN_POINT('Ctrl Pts',(5.72993077911996,-179.21175111262,-9.92453123332976));
#28976=CARTESIAN_POINT('Ctrl Pts',(-1.78726082715848E-11,-179.03675111262,
-9.92453123331945));
#28977=CARTESIAN_POINT('Ctrl Pts',(-5.7299307791557,-178.86175111262,-9.92453123330913));
#28978=CARTESIAN_POINT('Ctrl Pts',(-8.59489616871569,-178.68675111262,-4.96226561664425));
#28979=CARTESIAN_POINT('Ctrl Pts',(-11.4598615582757,-178.51175111262,2.06368086793017E-11));
#28980=CARTESIAN_POINT('Ctrl Pts',(-8.59489616869782,-178.33675111262,4.9622656166752));
#28981=CARTESIAN_POINT('Ctrl Pts',(-5.72993077911996,-178.16175111262,9.92453123332977));
#28982=CARTESIAN_POINT('Ctrl Pts',(1.7871392867044E-11,-177.98675111262,
9.92453123331945));
#28983=CARTESIAN_POINT('Ctrl Pts',(5.7299307791557,-177.81175111262,9.92453123330913));
#28984=CARTESIAN_POINT('Ctrl Pts',(8.59489616871569,-177.63675111262,4.96226561664425));
#28985=CARTESIAN_POINT('Ctrl Pts',(11.4598615582757,-177.46175111262,-2.06354052510241E-11));
#28986=CARTESIAN_POINT('Ctrl Pts',(8.59489616869782,-177.28675111262,-4.9622656166752));
#28987=CARTESIAN_POINT('Ctrl Pts',(5.72993077911996,-177.11175111262,-9.92453123332976));
#28988=CARTESIAN_POINT('Ctrl Pts',(-1.78726082715848E-11,-176.93675111262,
-9.92453123331945));
#28989=CARTESIAN_POINT('Ctrl Pts',(-5.7299307791557,-176.76175111262,-9.92453123330913));
#28990=CARTESIAN_POINT('Ctrl Pts',(-8.59489616871569,-176.58675111262,-4.96226561664425));
#28991=CARTESIAN_POINT('Ctrl Pts',(-11.4598615582757,-176.41175111262,2.06368086793017E-11));
#28992=CARTESIAN_POINT('Ctrl Pts',(-8.59489616869782,-176.23675111262,4.9622656166752));
#28993=CARTESIAN_POINT('Ctrl Pts',(-5.72993077911996,-176.06175111262,9.92453123332977));
#28994=CARTESIAN_POINT('Ctrl Pts',(1.7871392867044E-11,-175.88675111262,
9.92453123331945));
#28995=CARTESIAN_POINT('Ctrl Pts',(5.7299307791557,-175.71175111262,9.92453123330913));
#28996=CARTESIAN_POINT('Ctrl Pts',(8.59489616871569,-175.53675111262,4.96226561664425));
#28997=CARTESIAN_POINT('Ctrl Pts',(11.4598615582757,-175.36175111262,-2.06354052510241E-11));
#28998=CARTESIAN_POINT('Ctrl Pts',(8.59489616869782,-175.18675111262,-4.9622656166752));
#28999=CARTESIAN_POINT('Ctrl Pts',(5.72993077911996,-175.01175111262,-9.92453123332976));
#29000=CARTESIAN_POINT('Ctrl Pts',(-1.78726082715848E-11,-174.83675111262,
-9.92453123331945));
#29001=CARTESIAN_POINT('Ctrl Pts',(-5.7299307791557,-174.66175111262,-9.92453123330913));
#29002=CARTESIAN_POINT('Ctrl Pts',(-8.59489616871569,-174.48675111262,-4.96226561664425));
#29003=CARTESIAN_POINT('Ctrl Pts',(-11.4598615582757,-174.31175111262,2.06368086793017E-11));
#29004=CARTESIAN_POINT('Ctrl Pts',(-8.59489616869782,-174.13675111262,4.9622656166752));
#29005=CARTESIAN_POINT('Ctrl Pts',(-5.72993077911996,-173.96175111262,9.92453123332977));
#29006=CARTESIAN_POINT('Ctrl Pts',(1.7871392867044E-11,-173.78675111262,
9.92453123331945));
#29007=CARTESIAN_POINT('Ctrl Pts',(5.7299307791557,-173.61175111262,9.92453123330913));
#29008=CARTESIAN_POINT('Ctrl Pts',(8.59489616871569,-173.43675111262,4.96226561664425));
#29009=CARTESIAN_POINT('Ctrl Pts',(11.4598615582757,-173.26175111262,-2.06354052510241E-11));
#29010=CARTESIAN_POINT('Ctrl Pts',(8.59489616869782,-173.08675111262,-4.9622656166752));
#29011=CARTESIAN_POINT('Ctrl Pts',(5.72993077911996,-172.91175111262,-9.92453123332976));
#29012=CARTESIAN_POINT('Ctrl Pts',(-1.78726082715848E-11,-172.73675111262,
-9.92453123331945));
#29013=CARTESIAN_POINT('Ctrl Pts',(-5.7299307791557,-172.56175111262,-9.92453123330913));
#29014=CARTESIAN_POINT('Ctrl Pts',(-8.59489616871569,-172.38675111262,-4.96226561664425));
#29015=CARTESIAN_POINT('Ctrl Pts',(-11.4598615582757,-172.21175111262,2.06368086793017E-11));
#29016=CARTESIAN_POINT('Ctrl Pts',(-8.59489616869782,-172.03675111262,4.9622656166752));
#29017=CARTESIAN_POINT('Ctrl Pts',(-5.72993077911996,-171.86175111262,9.92453123332977));
#29018=CARTESIAN_POINT('Ctrl Pts',(1.7871392867044E-11,-171.68675111262,
9.92453123331945));
#29019=CARTESIAN_POINT('Ctrl Pts',(5.7299307791557,-171.51175111262,9.92453123330913));
#29020=CARTESIAN_POINT('Ctrl Pts',(8.59489616871569,-171.33675111262,4.96226561664425));
#29021=CARTESIAN_POINT('Ctrl Pts',(11.4598615582757,-171.16175111262,-2.06354052510241E-11));
#29022=CARTESIAN_POINT('Ctrl Pts',(8.59489616869782,-170.98675111262,-4.9622656166752));
#29023=CARTESIAN_POINT('Ctrl Pts',(5.72993077911996,-170.81175111262,-9.92453123332976));
#29024=CARTESIAN_POINT('Ctrl Pts',(-1.78726082715848E-11,-170.63675111262,
-9.92453123331945));
#29025=CARTESIAN_POINT('Ctrl Pts',(-5.7299307791557,-170.46175111262,-9.92453123330913));
#29026=CARTESIAN_POINT('Ctrl Pts',(-8.59489616871569,-170.28675111262,-4.96226561664425));
#29027=CARTESIAN_POINT('Ctrl Pts',(-11.4598615582757,-170.11175111262,2.06368086793017E-11));
#29028=CARTESIAN_POINT('Ctrl Pts',(-8.59489616869782,-169.93675111262,4.9622656166752));
#29029=CARTESIAN_POINT('Ctrl Pts',(-5.72993077911996,-169.76175111262,9.92453123332977));
#29030=CARTESIAN_POINT('Ctrl Pts',(1.7871392867044E-11,-169.58675111262,
9.92453123331945));
#29031=CARTESIAN_POINT('Ctrl Pts',(5.7299307791557,-169.41175111262,9.92453123330913));
#29032=CARTESIAN_POINT('Ctrl Pts',(8.59489616871569,-169.23675111262,4.96226561664425));
#29033=CARTESIAN_POINT('Ctrl Pts',(11.4598615582757,-169.06175111262,-2.06354052510241E-11));
#29034=CARTESIAN_POINT('Ctrl Pts',(8.59489616869782,-168.88675111262,-4.9622656166752));
#29035=CARTESIAN_POINT('Ctrl Pts',(5.72993077911996,-168.71175111262,-9.92453123332976));
#29036=CARTESIAN_POINT('Ctrl Pts',(-1.78726082715848E-11,-168.53675111262,
-9.92453123331945));
#29037=CARTESIAN_POINT('Ctrl Pts',(-5.7299307791557,-168.36175111262,-9.92453123330913));
#29038=CARTESIAN_POINT('Ctrl Pts',(-8.59489616871569,-168.18675111262,-4.96226561664425));
#29039=CARTESIAN_POINT('Ctrl Pts',(-11.4598615582757,-168.01175111262,2.06368086793017E-11));
#29040=CARTESIAN_POINT('Ctrl Pts',(-8.59489616869782,-167.83675111262,4.9622656166752));
#29041=CARTESIAN_POINT('Ctrl Pts',(-5.72993077911996,-167.66175111262,9.92453123332977));
#29042=CARTESIAN_POINT('Ctrl Pts',(1.7871392867044E-11,-167.48675111262,
9.92453123331945));
#29043=CARTESIAN_POINT('Ctrl Pts',(5.7299307791557,-167.31175111262,9.92453123330913));
#29044=CARTESIAN_POINT('Ctrl Pts',(8.59489616871569,-167.13675111262,4.96226561664425));
#29045=CARTESIAN_POINT('Ctrl Pts',(11.4598615582757,-166.96175111262,-2.06354052510241E-11));
#29046=CARTESIAN_POINT('Ctrl Pts',(8.59489616869782,-166.78675111262,-4.9622656166752));
#29047=CARTESIAN_POINT('Ctrl Pts',(5.72993077911996,-166.61175111262,-9.92453123332976));
#29048=CARTESIAN_POINT('Ctrl Pts',(-1.78726082715848E-11,-166.43675111262,
-9.92453123331945));
#29049=CARTESIAN_POINT('Ctrl Pts',(-5.7299307791557,-166.26175111262,-9.92453123330913));
#29050=CARTESIAN_POINT('Ctrl Pts',(-8.59489616871569,-166.08675111262,-4.96226561664425));
#29051=CARTESIAN_POINT('Ctrl Pts',(-11.4598615582757,-165.91175111262,2.06368086793017E-11));
#29052=CARTESIAN_POINT('Ctrl Pts',(-8.59489616869782,-165.73675111262,4.9622656166752));
#29053=CARTESIAN_POINT('Ctrl Pts',(-5.72993077911996,-165.56175111262,9.92453123332977));
#29054=CARTESIAN_POINT('Ctrl Pts',(1.7871392867044E-11,-165.38675111262,
9.92453123331945));
#29055=CARTESIAN_POINT('Ctrl Pts',(5.7299307791557,-165.21175111262,9.92453123330913));
#29056=CARTESIAN_POINT('Ctrl Pts',(8.59489616871569,-165.03675111262,4.96226561664425));
#29057=CARTESIAN_POINT('Ctrl Pts',(11.4598615582757,-164.86175111262,-2.06354052510241E-11));
#29058=CARTESIAN_POINT('Ctrl Pts',(8.59489616869782,-164.68675111262,-4.9622656166752));
#29059=CARTESIAN_POINT('Ctrl Pts',(5.72993077911996,-164.51175111262,-9.92453123332976));
#29060=CARTESIAN_POINT('Ctrl Pts',(-1.78726082715848E-11,-164.33675111262,
-9.92453123331945));
#29061=CARTESIAN_POINT('Ctrl Pts',(-5.7299307791557,-164.16175111262,-9.92453123330913));
#29062=CARTESIAN_POINT('Ctrl Pts',(-8.59489616871569,-163.98675111262,-4.96226561664425));
#29063=CARTESIAN_POINT('Ctrl Pts',(-11.4598615582757,-163.81175111262,2.06368086793017E-11));
#29064=CARTESIAN_POINT('Ctrl Pts',(-8.59489616869782,-163.63675111262,4.9622656166752));
#29065=CARTESIAN_POINT('Ctrl Pts',(-5.72993077911996,-163.46175111262,9.92453123332977));
#29066=CARTESIAN_POINT('Ctrl Pts',(1.7871392867044E-11,-163.28675111262,
9.92453123331945));
#29067=CARTESIAN_POINT('Ctrl Pts',(5.7299307791557,-163.11175111262,9.92453123330913));
#29068=CARTESIAN_POINT('Ctrl Pts',(8.59489616871569,-162.93675111262,4.96226561664425));
#29069=CARTESIAN_POINT('Ctrl Pts',(11.4598615582757,-162.76175111262,-2.06354052510241E-11));
#29070=CARTESIAN_POINT('Ctrl Pts',(8.59489616869782,-162.58675111262,-4.9622656166752));
#29071=CARTESIAN_POINT('Ctrl Pts',(5.72993077911996,-162.41175111262,-9.92453123332976));
#29072=CARTESIAN_POINT('Ctrl Pts',(-1.78726082715848E-11,-162.23675111262,
-9.92453123331945));
#29073=CARTESIAN_POINT('Ctrl Pts',(-5.7299307791557,-162.06175111262,-9.92453123330913));
#29074=CARTESIAN_POINT('Ctrl Pts',(-8.59489616871569,-161.88675111262,-4.96226561664425));
#29075=CARTESIAN_POINT('Ctrl Pts',(-11.4598615582757,-161.71175111262,2.06368086793017E-11));
#29076=CARTESIAN_POINT('Ctrl Pts',(-8.59489616869782,-161.53675111262,4.9622656166752));
#29077=CARTESIAN_POINT('Ctrl Pts',(-5.72993077911996,-161.36175111262,9.92453123332977));
#29078=CARTESIAN_POINT('Ctrl Pts',(1.7871392867044E-11,-161.18675111262,
9.92453123331945));
#29079=CARTESIAN_POINT('Ctrl Pts',(5.7299307791557,-161.01175111262,9.92453123330913));
#29080=CARTESIAN_POINT('Ctrl Pts',(8.59489616871569,-160.83675111262,4.96226561664425));
#29081=CARTESIAN_POINT('Ctrl Pts',(11.4598615582757,-160.66175111262,-2.06354052510241E-11));
#29082=CARTESIAN_POINT('Ctrl Pts',(8.59489616869782,-160.48675111262,-4.9622656166752));
#29083=CARTESIAN_POINT('Ctrl Pts',(5.72993077911996,-160.31175111262,-9.92453123332976));
#29084=CARTESIAN_POINT('Ctrl Pts',(-1.78726082715848E-11,-160.13675111262,
-9.92453123331945));
#29085=CARTESIAN_POINT('Ctrl Pts',(-5.7299307791557,-159.96175111262,-9.92453123330913));
#29086=CARTESIAN_POINT('Ctrl Pts',(-8.59489616871569,-159.78675111262,-4.96226561664425));
#29087=CARTESIAN_POINT('Ctrl Pts',(-11.4598615582757,-159.61175111262,2.06368086793017E-11));
#29088=CARTESIAN_POINT('Ctrl Pts',(-8.59489616869782,-159.43675111262,4.9622656166752));
#29089=CARTESIAN_POINT('Ctrl Pts',(-5.72993077911996,-159.26175111262,9.92453123332977));
#29090=CARTESIAN_POINT('Ctrl Pts',(1.7871392867044E-11,-159.08675111262,
9.92453123331945));
#29091=CARTESIAN_POINT('Ctrl Pts',(5.7299307791557,-158.91175111262,9.92453123330913));
#29092=CARTESIAN_POINT('Ctrl Pts',(8.59489616871569,-158.73675111262,4.96226561664425));
#29093=CARTESIAN_POINT('Ctrl Pts',(11.4598615582757,-158.56175111262,-2.06354052510241E-11));
#29094=CARTESIAN_POINT('Ctrl Pts',(8.59489616869782,-158.38675111262,-4.9622656166752));
#29095=CARTESIAN_POINT('Ctrl Pts',(5.72993077911996,-158.21175111262,-9.92453123332976));
#29096=CARTESIAN_POINT('Ctrl Pts',(-1.78726082715848E-11,-158.03675111262,
-9.92453123331945));
#29097=CARTESIAN_POINT('Ctrl Pts',(-5.7299307791557,-157.86175111262,-9.92453123330913));
#29098=CARTESIAN_POINT('Ctrl Pts',(-8.59489616871569,-157.68675111262,-4.96226561664425));
#29099=CARTESIAN_POINT('Ctrl Pts',(-11.4598615582757,-157.51175111262,2.06368086793017E-11));
#29100=CARTESIAN_POINT('Ctrl Pts',(-8.59489616869782,-157.33675111262,4.9622656166752));
#29101=CARTESIAN_POINT('Ctrl Pts',(-5.72993077911996,-157.16175111262,9.92453123332977));
#29102=CARTESIAN_POINT('Ctrl Pts',(1.7871392867044E-11,-156.98675111262,
9.92453123331945));
#29103=CARTESIAN_POINT('Ctrl Pts',(5.7299307791557,-156.81175111262,9.92453123330913));
#29104=CARTESIAN_POINT('Ctrl Pts',(8.59489616871569,-156.63675111262,4.96226561664425));
#29105=CARTESIAN_POINT('Ctrl Pts',(11.4598615582757,-156.46175111262,-2.06354052510241E-11));
#29106=CARTESIAN_POINT('Ctrl Pts',(8.59489616869782,-156.28675111262,-4.9622656166752));
#29107=CARTESIAN_POINT('Ctrl Pts',(5.72993077911996,-156.11175111262,-9.92453123332976));
#29108=CARTESIAN_POINT('Ctrl Pts',(-1.78726082715848E-11,-155.93675111262,
-9.92453123331945));
#29109=CARTESIAN_POINT('Ctrl Pts',(-5.7299307791557,-155.76175111262,-9.92453123330913));
#29110=CARTESIAN_POINT('Ctrl Pts',(-8.59489616871569,-155.58675111262,-4.96226561664425));
#29111=CARTESIAN_POINT('Ctrl Pts',(-11.4598615582757,-155.41175111262,2.06368086793017E-11));
#29112=CARTESIAN_POINT('Ctrl Pts',(-8.59489616869782,-155.23675111262,4.9622656166752));
#29113=CARTESIAN_POINT('Ctrl Pts',(-5.72993077911996,-155.06175111262,9.92453123332977));
#29114=CARTESIAN_POINT('Ctrl Pts',(1.7871392867044E-11,-154.88675111262,
9.92453123331945));
#29115=CARTESIAN_POINT('Ctrl Pts',(5.7299307791557,-154.71175111262,9.92453123330913));
#29116=CARTESIAN_POINT('Ctrl Pts',(8.59489616871569,-154.53675111262,4.96226561664425));
#29117=CARTESIAN_POINT('Ctrl Pts',(11.4598615582757,-154.36175111262,-2.06354052510241E-11));
#29118=CARTESIAN_POINT('Ctrl Pts',(8.59489616869782,-154.18675111262,-4.9622656166752));
#29119=CARTESIAN_POINT('Ctrl Pts',(5.72993077911996,-154.01175111262,-9.92453123332976));
#29120=CARTESIAN_POINT('Ctrl Pts',(-1.78726082715848E-11,-153.83675111262,
-9.92453123331945));
#29121=CARTESIAN_POINT('Ctrl Pts',(-5.7299307791557,-153.66175111262,-9.92453123330913));
#29122=CARTESIAN_POINT('Ctrl Pts',(-8.59489616871569,-153.48675111262,-4.96226561664425));
#29123=CARTESIAN_POINT('Ctrl Pts',(-11.4598615582757,-153.31175111262,2.06368086793017E-11));
#29124=CARTESIAN_POINT('Ctrl Pts',(-8.59489616869782,-153.13675111262,4.9622656166752));
#29125=CARTESIAN_POINT('Ctrl Pts',(-5.72993077911996,-152.96175111262,9.92453123332977));
#29126=CARTESIAN_POINT('Ctrl Pts',(1.7871392867044E-11,-152.78675111262,
9.92453123331945));
#29127=CARTESIAN_POINT('Ctrl Pts',(5.7299307791557,-152.61175111262,9.92453123330913));
#29128=CARTESIAN_POINT('Ctrl Pts',(8.59489616871569,-152.43675111262,4.96226561664425));
#29129=CARTESIAN_POINT('Ctrl Pts',(11.4598615582757,-152.26175111262,-2.06354052510241E-11));
#29130=CARTESIAN_POINT('Ctrl Pts',(8.59489616869782,-152.08675111262,-4.9622656166752));
#29131=CARTESIAN_POINT('Ctrl Pts',(5.72993077911996,-151.91175111262,-9.92453123332976));
#29132=CARTESIAN_POINT('Ctrl Pts',(-1.78726082715848E-11,-151.73675111262,
-9.92453123331945));
#29133=CARTESIAN_POINT('Ctrl Pts',(-5.7299307791557,-151.56175111262,-9.92453123330913));
#29134=CARTESIAN_POINT('Ctrl Pts',(-8.59489616871569,-151.38675111262,-4.96226561664425));
#29135=CARTESIAN_POINT('Ctrl Pts',(-11.4598615582757,-151.21175111262,2.06368086793017E-11));
#29136=CARTESIAN_POINT('Ctrl Pts',(-8.59489616869782,-151.03675111262,4.9622656166752));
#29137=CARTESIAN_POINT('Ctrl Pts',(-5.72993077911996,-150.86175111262,9.92453123332977));
#29138=CARTESIAN_POINT('Ctrl Pts',(1.7871392867044E-11,-150.68675111262,
9.92453123331945));
#29139=CARTESIAN_POINT('Ctrl Pts',(5.7299307791557,-150.51175111262,9.92453123330913));
#29140=CARTESIAN_POINT('Ctrl Pts',(8.59489616871569,-150.33675111262,4.96226561664425));
#29141=CARTESIAN_POINT('Ctrl Pts',(11.4598615582757,-150.16175111262,-2.06354052510241E-11));
#29142=CARTESIAN_POINT('Ctrl Pts',(8.59489616869782,-149.98675111262,-4.9622656166752));
#29143=CARTESIAN_POINT('Ctrl Pts',(5.72993077911996,-149.81175111262,-9.92453123332976));
#29144=CARTESIAN_POINT('Ctrl Pts',(-1.78726082715848E-11,-149.63675111262,
-9.92453123331945));
#29145=CARTESIAN_POINT('Ctrl Pts',(-5.7299307791557,-149.46175111262,-9.92453123330913));
#29146=CARTESIAN_POINT('Ctrl Pts',(-8.59489616871569,-149.28675111262,-4.96226561664425));
#29147=CARTESIAN_POINT('Ctrl Pts',(-11.4598615582757,-149.11175111262,2.06368086793017E-11));
#29148=CARTESIAN_POINT('Ctrl Pts',(-8.59489616869782,-148.93675111262,4.9622656166752));
#29149=CARTESIAN_POINT('Ctrl Pts',(-5.72993077911996,-148.76175111262,9.92453123332977));
#29150=CARTESIAN_POINT('Ctrl Pts',(1.7871392867044E-11,-148.58675111262,
9.92453123331945));
#29151=CARTESIAN_POINT('Ctrl Pts',(5.7299307791557,-148.41175111262,9.92453123330913));
#29152=CARTESIAN_POINT('Ctrl Pts',(8.59489616871569,-148.23675111262,4.96226561664425));
#29153=CARTESIAN_POINT('Ctrl Pts',(11.4598615582757,-148.06175111262,-2.06354052510241E-11));
#29154=CARTESIAN_POINT('Ctrl Pts',(8.59489616869782,-147.88675111262,-4.9622656166752));
#29155=CARTESIAN_POINT('Ctrl Pts',(5.72993077911996,-147.71175111262,-9.92453123332976));
#29156=CARTESIAN_POINT('Ctrl Pts',(-1.78726082715848E-11,-147.53675111262,
-9.92453123331945));
#29157=CARTESIAN_POINT('Ctrl Pts',(-5.7299307791557,-147.36175111262,-9.92453123330913));
#29158=CARTESIAN_POINT('Ctrl Pts',(-8.59489616871569,-147.18675111262,-4.96226561664425));
#29159=CARTESIAN_POINT('Ctrl Pts',(-11.4598615582757,-147.01175111262,2.06368086793017E-11));
#29160=CARTESIAN_POINT('Ctrl Pts',(-8.59489616869782,-146.83675111262,4.9622656166752));
#29161=CARTESIAN_POINT('Ctrl Pts',(-5.72993077911996,-146.66175111262,9.92453123332977));
#29162=CARTESIAN_POINT('Ctrl Pts',(1.7871392867044E-11,-146.48675111262,
9.92453123331945));
#29163=CARTESIAN_POINT('Ctrl Pts',(5.7299307791557,-146.31175111262,9.92453123330913));
#29164=CARTESIAN_POINT('Ctrl Pts',(8.59489616871569,-146.13675111262,4.96226561664425));
#29165=CARTESIAN_POINT('Ctrl Pts',(11.4598615582757,-145.96175111262,-2.06354052510241E-11));
#29166=CARTESIAN_POINT('Ctrl Pts',(8.59489616869782,-145.78675111262,-4.9622656166752));
#29167=CARTESIAN_POINT('Ctrl Pts',(5.72993077911996,-145.61175111262,-9.92453123332976));
#29168=CARTESIAN_POINT('Ctrl Pts',(-1.78726082715848E-11,-145.43675111262,
-9.92453123331945));
#29169=CARTESIAN_POINT('Ctrl Pts',(-5.7299307791557,-145.26175111262,-9.92453123330913));
#29170=CARTESIAN_POINT('Ctrl Pts',(-8.59489616871569,-145.08675111262,-4.96226561664425));
#29171=CARTESIAN_POINT('Ctrl Pts',(-11.4598615582757,-144.91175111262,2.06368086793017E-11));
#29172=CARTESIAN_POINT('Ctrl Pts',(-8.59489616869782,-144.73675111262,4.9622656166752));
#29173=CARTESIAN_POINT('Ctrl Pts',(-5.72993077911996,-144.56175111262,9.92453123332977));
#29174=CARTESIAN_POINT('Ctrl Pts',(1.7871392867044E-11,-144.38675111262,
9.92453123331945));
#29175=CARTESIAN_POINT('Ctrl Pts',(5.7299307791557,-144.21175111262,9.92453123330913));
#29176=CARTESIAN_POINT('Ctrl Pts',(8.59489616871569,-144.03675111262,4.96226561664425));
#29177=CARTESIAN_POINT('Ctrl Pts',(11.4598615582757,-143.86175111262,-2.06354052510241E-11));
#29178=CARTESIAN_POINT('Ctrl Pts',(8.59489616869782,-143.68675111262,-4.9622656166752));
#29179=CARTESIAN_POINT('Ctrl Pts',(5.72993077911996,-143.51175111262,-9.92453123332976));
#29180=CARTESIAN_POINT('Ctrl Pts',(-1.78726082715848E-11,-143.33675111262,
-9.92453123331945));
#29181=CARTESIAN_POINT('Ctrl Pts',(-5.7299307791557,-143.16175111262,-9.92453123330913));
#29182=CARTESIAN_POINT('Ctrl Pts',(-8.59489616871569,-142.98675111262,-4.96226561664425));
#29183=CARTESIAN_POINT('Ctrl Pts',(-11.4598615582757,-142.81175111262,2.06368086793017E-11));
#29184=CARTESIAN_POINT('Ctrl Pts',(-8.59489616869782,-142.63675111262,4.9622656166752));
#29185=CARTESIAN_POINT('Ctrl Pts',(-5.72993077911996,-142.46175111262,9.92453123332977));
#29186=CARTESIAN_POINT('Ctrl Pts',(1.7871392867044E-11,-142.28675111262,
9.92453123331945));
#29187=CARTESIAN_POINT('Ctrl Pts',(5.7299307791557,-142.11175111262,9.92453123330913));
#29188=CARTESIAN_POINT('Ctrl Pts',(8.59489616871569,-141.93675111262,4.96226561664425));
#29189=CARTESIAN_POINT('Ctrl Pts',(11.4598615582757,-141.76175111262,-2.06354052510241E-11));
#29190=CARTESIAN_POINT('Ctrl Pts',(8.59489616869782,-141.58675111262,-4.9622656166752));
#29191=CARTESIAN_POINT('Ctrl Pts',(5.72993077911996,-141.41175111262,-9.92453123332976));
#29192=CARTESIAN_POINT('Ctrl Pts',(-1.78726082715848E-11,-141.23675111262,
-9.92453123331945));
#29193=CARTESIAN_POINT('Ctrl Pts',(-5.7299307791557,-141.06175111262,-9.92453123330913));
#29194=CARTESIAN_POINT('Ctrl Pts',(-8.59489616871569,-140.88675111262,-4.96226561664425));
#29195=CARTESIAN_POINT('Ctrl Pts',(-11.4598615582757,-140.71175111262,2.06368086793017E-11));
#29196=CARTESIAN_POINT('Ctrl Pts',(-8.59489616869782,-140.53675111262,4.9622656166752));
#29197=CARTESIAN_POINT('Ctrl Pts',(-5.72993077911996,-140.36175111262,9.92453123332977));
#29198=CARTESIAN_POINT('Ctrl Pts',(1.7871392867044E-11,-140.18675111262,
9.92453123331945));
#29199=CARTESIAN_POINT('Ctrl Pts',(5.7299307791557,-140.01175111262,9.92453123330913));
#29200=CARTESIAN_POINT('Ctrl Pts',(8.59489616871569,-139.83675111262,4.96226561664425));
#29201=CARTESIAN_POINT('Ctrl Pts',(11.4598615582757,-139.66175111262,-2.06354052510241E-11));
#29202=CARTESIAN_POINT('Ctrl Pts',(8.59489616869782,-139.48675111262,-4.9622656166752));
#29203=CARTESIAN_POINT('Ctrl Pts',(5.72993077911996,-139.31175111262,-9.92453123332976));
#29204=CARTESIAN_POINT('Ctrl Pts',(-1.78726082715848E-11,-139.13675111262,
-9.92453123331945));
#29205=CARTESIAN_POINT('Ctrl Pts',(-5.7299307791557,-138.96175111262,-9.92453123330913));
#29206=CARTESIAN_POINT('Ctrl Pts',(-8.59489616871569,-138.78675111262,-4.96226561664425));
#29207=CARTESIAN_POINT('Ctrl Pts',(-11.4598615582757,-138.61175111262,2.06368086793017E-11));
#29208=CARTESIAN_POINT('Ctrl Pts',(-8.59489616869782,-138.43675111262,4.9622656166752));
#29209=CARTESIAN_POINT('Ctrl Pts',(-5.72993077911996,-138.26175111262,9.92453123332977));
#29210=CARTESIAN_POINT('Ctrl Pts',(1.7871392867044E-11,-138.08675111262,
9.92453123331945));
#29211=CARTESIAN_POINT('Ctrl Pts',(5.7299307791557,-137.91175111262,9.92453123330913));
#29212=CARTESIAN_POINT('Ctrl Pts',(8.59489616871569,-137.73675111262,4.96226561664425));
#29213=CARTESIAN_POINT('Ctrl Pts',(11.4598615582757,-137.56175111262,-2.06354052510241E-11));
#29214=CARTESIAN_POINT('Ctrl Pts',(8.59489616869782,-137.38675111262,-4.9622656166752));
#29215=CARTESIAN_POINT('Ctrl Pts',(5.72993077911996,-137.21175111262,-9.92453123332976));
#29216=CARTESIAN_POINT('Ctrl Pts',(-1.78726082715848E-11,-137.03675111262,
-9.92453123331945));
#29217=CARTESIAN_POINT('Ctrl Pts',(-5.7299307791557,-136.86175111262,-9.92453123330913));
#29218=CARTESIAN_POINT('Ctrl Pts',(-8.59489616871569,-136.68675111262,-4.96226561664425));
#29219=CARTESIAN_POINT('Ctrl Pts',(-11.4598615582757,-136.51175111262,2.06368086793017E-11));
#29220=CARTESIAN_POINT('Ctrl Pts',(-8.59489616869782,-136.33675111262,4.9622656166752));
#29221=CARTESIAN_POINT('Ctrl Pts',(-5.72993077911996,-136.16175111262,9.92453123332977));
#29222=CARTESIAN_POINT('Ctrl Pts',(1.7871392867044E-11,-135.98675111262,
9.92453123331945));
#29223=CARTESIAN_POINT('Ctrl Pts',(5.7299307791557,-135.81175111262,9.92453123330913));
#29224=CARTESIAN_POINT('Ctrl Pts',(8.59489616871569,-135.63675111262,4.96226561664425));
#29225=CARTESIAN_POINT('Ctrl Pts',(11.4598615582757,-135.46175111262,-2.06354052510241E-11));
#29226=CARTESIAN_POINT('Ctrl Pts',(8.59489616869782,-135.28675111262,-4.9622656166752));
#29227=CARTESIAN_POINT('Ctrl Pts',(5.72993077911996,-135.11175111262,-9.92453123332976));
#29228=CARTESIAN_POINT('Ctrl Pts',(-1.78726082715848E-11,-134.93675111262,
-9.92453123331945));
#29229=CARTESIAN_POINT('Ctrl Pts',(-5.7299307791557,-134.76175111262,-9.92453123330913));
#29230=CARTESIAN_POINT('Ctrl Pts',(-8.59489616871569,-134.58675111262,-4.96226561664425));
#29231=CARTESIAN_POINT('Ctrl Pts',(-11.4598615582757,-134.41175111262,2.06368086793017E-11));
#29232=CARTESIAN_POINT('Ctrl Pts',(-8.59489616869782,-134.23675111262,4.9622656166752));
#29233=CARTESIAN_POINT('Ctrl Pts',(-5.72993077911996,-134.06175111262,9.92453123332977));
#29234=CARTESIAN_POINT('Ctrl Pts',(1.7871392867044E-11,-133.88675111262,
9.92453123331945));
#29235=CARTESIAN_POINT('Ctrl Pts',(5.7299307791557,-133.71175111262,9.92453123330913));
#29236=CARTESIAN_POINT('Ctrl Pts',(8.59489616871569,-133.53675111262,4.96226561664425));
#29237=CARTESIAN_POINT('Ctrl Pts',(11.4598615582757,-133.36175111262,-2.06354052510241E-11));
#29238=CARTESIAN_POINT('Ctrl Pts',(8.59489616869782,-133.18675111262,-4.9622656166752));
#29239=CARTESIAN_POINT('Ctrl Pts',(5.72993077911996,-133.01175111262,-9.92453123332976));
#29240=CARTESIAN_POINT('Ctrl Pts',(-1.78726082715848E-11,-132.83675111262,
-9.92453123331945));
#29241=CARTESIAN_POINT('Ctrl Pts',(-5.7299307791557,-132.66175111262,-9.92453123330913));
#29242=CARTESIAN_POINT('Ctrl Pts',(-8.59489616871569,-132.48675111262,-4.96226561664425));
#29243=CARTESIAN_POINT('Ctrl Pts',(-11.4598615582757,-132.31175111262,2.06368086793017E-11));
#29244=CARTESIAN_POINT('Ctrl Pts',(-8.59489616869782,-132.13675111262,4.9622656166752));
#29245=CARTESIAN_POINT('Ctrl Pts',(-5.72993077911996,-131.96175111262,9.92453123332977));
#29246=CARTESIAN_POINT('Ctrl Pts',(1.7871392867044E-11,-131.78675111262,
9.92453123331945));
#29247=CARTESIAN_POINT('Ctrl Pts',(5.7299307791557,-131.61175111262,9.92453123330913));
#29248=CARTESIAN_POINT('Ctrl Pts',(8.59489616871569,-131.43675111262,4.96226561664425));
#29249=CARTESIAN_POINT('Ctrl Pts',(11.4598615582757,-131.26175111262,-2.06354052510241E-11));
#29250=CARTESIAN_POINT('Ctrl Pts',(8.59489616869782,-131.08675111262,-4.9622656166752));
#29251=CARTESIAN_POINT('Ctrl Pts',(5.72993077911996,-130.91175111262,-9.92453123332976));
#29252=CARTESIAN_POINT('Ctrl Pts',(-1.78726082715848E-11,-130.73675111262,
-9.92453123331945));
#29253=CARTESIAN_POINT('Ctrl Pts',(-5.7299307791557,-130.56175111262,-9.92453123330913));
#29254=CARTESIAN_POINT('Ctrl Pts',(-8.59489616871569,-130.38675111262,-4.96226561664425));
#29255=CARTESIAN_POINT('Ctrl Pts',(-11.4598615582757,-130.21175111262,2.06368086793017E-11));
#29256=CARTESIAN_POINT('Ctrl Pts',(-8.59489616869782,-130.03675111262,4.9622656166752));
#29257=CARTESIAN_POINT('Ctrl Pts',(-5.72993077911996,-129.86175111262,9.92453123332977));
#29258=CARTESIAN_POINT('Ctrl Pts',(1.7871392867044E-11,-129.68675111262,
9.92453123331945));
#29259=CARTESIAN_POINT('Ctrl Pts',(5.7299307791557,-129.51175111262,9.92453123330913));
#29260=CARTESIAN_POINT('Ctrl Pts',(8.59489616871569,-129.33675111262,4.96226561664425));
#29261=CARTESIAN_POINT('Ctrl Pts',(11.4598615582757,-129.16175111262,-2.06354052510241E-11));
#29262=CARTESIAN_POINT('Ctrl Pts',(8.59489616869782,-128.98675111262,-4.9622656166752));
#29263=CARTESIAN_POINT('Ctrl Pts',(5.72993077911996,-128.81175111262,-9.92453123332976));
#29264=CARTESIAN_POINT('Ctrl Pts',(-1.78726082715848E-11,-128.63675111262,
-9.92453123331945));
#29265=CARTESIAN_POINT('Ctrl Pts',(-5.7299307791557,-128.46175111262,-9.92453123330913));
#29266=CARTESIAN_POINT('Ctrl Pts',(-8.59489616871569,-128.28675111262,-4.96226561664425));
#29267=CARTESIAN_POINT('Ctrl Pts',(-11.4598615582757,-128.11175111262,2.06368086793017E-11));
#29268=CARTESIAN_POINT('Ctrl Pts',(-8.59489616869782,-127.93675111262,4.9622656166752));
#29269=CARTESIAN_POINT('Ctrl Pts',(-5.72993077911996,-127.76175111262,9.92453123332977));
#29270=CARTESIAN_POINT('Ctrl Pts',(1.7871392867044E-11,-127.58675111262,
9.92453123331945));
#29271=CARTESIAN_POINT('Ctrl Pts',(5.7299307791557,-127.41175111262,9.92453123330913));
#29272=CARTESIAN_POINT('Ctrl Pts',(8.59489616871569,-127.23675111262,4.96226561664425));
#29273=CARTESIAN_POINT('Ctrl Pts',(11.4598615582757,-127.06175111262,-2.06354052510241E-11));
#29274=CARTESIAN_POINT('Ctrl Pts',(8.59489616869782,-126.88675111262,-4.9622656166752));
#29275=CARTESIAN_POINT('Ctrl Pts',(5.72993077911996,-126.71175111262,-9.92453123332976));
#29276=CARTESIAN_POINT('Ctrl Pts',(-1.78726082715848E-11,-126.53675111262,
-9.92453123331945));
#29277=CARTESIAN_POINT('Ctrl Pts',(-5.7299307791557,-126.36175111262,-9.92453123330913));
#29278=CARTESIAN_POINT('Ctrl Pts',(-8.59489616871569,-126.18675111262,-4.96226561664425));
#29279=CARTESIAN_POINT('Ctrl Pts',(-11.4598615582757,-126.01175111262,2.06368086793017E-11));
#29280=CARTESIAN_POINT('Ctrl Pts',(-8.59489616869782,-125.83675111262,4.9622656166752));
#29281=CARTESIAN_POINT('Ctrl Pts',(-5.72993077911996,-125.66175111262,9.92453123332977));
#29282=CARTESIAN_POINT('Ctrl Pts',(1.7871392867044E-11,-125.48675111262,
9.92453123331945));
#29283=CARTESIAN_POINT('Ctrl Pts',(5.7299307791557,-125.31175111262,9.92453123330913));
#29284=CARTESIAN_POINT('Ctrl Pts',(8.59489616871569,-125.13675111262,4.96226561664425));
#29285=CARTESIAN_POINT('Ctrl Pts',(11.4598615582757,-124.96175111262,-2.06354052510241E-11));
#29286=CARTESIAN_POINT('Ctrl Pts',(8.59489616869782,-124.78675111262,-4.9622656166752));
#29287=CARTESIAN_POINT('Ctrl Pts',(5.72993077911996,-124.61175111262,-9.92453123332976));
#29288=CARTESIAN_POINT('Ctrl Pts',(-1.78726082715848E-11,-124.43675111262,
-9.92453123331945));
#29289=CARTESIAN_POINT('Ctrl Pts',(-5.7299307791557,-124.26175111262,-9.92453123330913));
#29290=CARTESIAN_POINT('Ctrl Pts',(-8.59489616871569,-124.08675111262,-4.96226561664425));
#29291=CARTESIAN_POINT('Ctrl Pts',(-11.4598615582757,-123.91175111262,2.06368086793017E-11));
#29292=CARTESIAN_POINT('Ctrl Pts',(-8.59489616869782,-123.73675111262,4.9622656166752));
#29293=CARTESIAN_POINT('Ctrl Pts',(-5.72993077911996,-123.56175111262,9.92453123332977));
#29294=CARTESIAN_POINT('Ctrl Pts',(1.7871392867044E-11,-123.38675111262,
9.92453123331945));
#29295=CARTESIAN_POINT('Ctrl Pts',(5.7299307791557,-123.21175111262,9.92453123330913));
#29296=CARTESIAN_POINT('Ctrl Pts',(8.59489616871569,-123.03675111262,4.96226561664425));
#29297=CARTESIAN_POINT('Ctrl Pts',(11.4598615582757,-122.86175111262,-2.06354052510241E-11));
#29298=CARTESIAN_POINT('Ctrl Pts',(8.59489616869782,-122.68675111262,-4.9622656166752));
#29299=CARTESIAN_POINT('Ctrl Pts',(5.72993077911996,-122.51175111262,-9.92453123332976));
#29300=CARTESIAN_POINT('Ctrl Pts',(-1.78726082715848E-11,-122.33675111262,
-9.92453123331945));
#29301=CARTESIAN_POINT('Ctrl Pts',(-5.7299307791557,-122.16175111262,-9.92453123330913));
#29302=CARTESIAN_POINT('Ctrl Pts',(-8.59489616871569,-121.98675111262,-4.96226561664425));
#29303=CARTESIAN_POINT('Ctrl Pts',(-11.4598615582757,-121.81175111262,2.06368086793017E-11));
#29304=CARTESIAN_POINT('Ctrl Pts',(-8.59489616869782,-121.63675111262,4.9622656166752));
#29305=CARTESIAN_POINT('Ctrl Pts',(-5.72993077911996,-121.46175111262,9.92453123332977));
#29306=CARTESIAN_POINT('Ctrl Pts',(1.7871392867044E-11,-121.28675111262,
9.92453123331945));
#29307=CARTESIAN_POINT('Ctrl Pts',(5.7299307791557,-121.11175111262,9.92453123330913));
#29308=CARTESIAN_POINT('Ctrl Pts',(8.59489616871569,-120.93675111262,4.96226561664425));
#29309=CARTESIAN_POINT('Ctrl Pts',(11.4598615582757,-120.76175111262,-2.06354052510241E-11));
#29310=CARTESIAN_POINT('Ctrl Pts',(8.59489616869782,-120.58675111262,-4.9622656166752));
#29311=CARTESIAN_POINT('Ctrl Pts',(5.72993077911996,-120.41175111262,-9.92453123332976));
#29312=CARTESIAN_POINT('Ctrl Pts',(-1.78726082715848E-11,-120.23675111262,
-9.92453123331945));
#29313=CARTESIAN_POINT('Ctrl Pts',(-5.7299307791557,-120.06175111262,-9.92453123330913));
#29314=CARTESIAN_POINT('Ctrl Pts',(-8.59489616871569,-119.88675111262,-4.96226561664425));
#29315=CARTESIAN_POINT('Ctrl Pts',(-11.4598615582757,-119.71175111262,2.06368086793017E-11));
#29316=CARTESIAN_POINT('Ctrl Pts',(-8.59489616869782,-119.53675111262,4.9622656166752));
#29317=CARTESIAN_POINT('Ctrl Pts',(-5.72993077911996,-119.36175111262,9.92453123332977));
#29318=CARTESIAN_POINT('Ctrl Pts',(1.7871392867044E-11,-119.18675111262,
9.92453123331945));
#29319=CARTESIAN_POINT('Ctrl Pts',(5.7299307791557,-119.01175111262,9.92453123330913));
#29320=CARTESIAN_POINT('Ctrl Pts',(8.59489616871569,-118.83675111262,4.96226561664425));
#29321=CARTESIAN_POINT('Ctrl Pts',(11.4598615582757,-118.66175111262,-2.06354052510241E-11));
#29322=CARTESIAN_POINT('Ctrl Pts',(8.59489616869782,-118.48675111262,-4.9622656166752));
#29323=CARTESIAN_POINT('Ctrl Pts',(5.72993077911996,-118.31175111262,-9.92453123332976));
#29324=CARTESIAN_POINT('Ctrl Pts',(-1.78726082715848E-11,-118.13675111262,
-9.92453123331945));
#29325=CARTESIAN_POINT('Ctrl Pts',(-5.7299307791557,-117.96175111262,-9.92453123330913));
#29326=CARTESIAN_POINT('Ctrl Pts',(-8.59489616871569,-117.78675111262,-4.96226561664425));
#29327=CARTESIAN_POINT('Ctrl Pts',(-11.4598615582757,-117.61175111262,2.06368086793017E-11));
#29328=CARTESIAN_POINT('Ctrl Pts',(-8.59489616869782,-117.43675111262,4.9622656166752));
#29329=CARTESIAN_POINT('Ctrl Pts',(-5.72993077911996,-117.26175111262,9.92453123332977));
#29330=CARTESIAN_POINT('Ctrl Pts',(1.7871392867044E-11,-117.08675111262,
9.92453123331945));
#29331=CARTESIAN_POINT('Ctrl Pts',(5.7299307791557,-116.91175111262,9.92453123330913));
#29332=CARTESIAN_POINT('Ctrl Pts',(8.59489616871569,-116.73675111262,4.96226561664425));
#29333=CARTESIAN_POINT('Ctrl Pts',(11.4598615582757,-116.56175111262,-2.06354052510241E-11));
#29334=CARTESIAN_POINT('Ctrl Pts',(8.59489616869782,-116.38675111262,-4.9622656166752));
#29335=CARTESIAN_POINT('Ctrl Pts',(5.72993077911996,-116.21175111262,-9.92453123332976));
#29336=CARTESIAN_POINT('Ctrl Pts',(-1.78726082715848E-11,-116.03675111262,
-9.92453123331945));
#29337=CARTESIAN_POINT('Ctrl Pts',(-5.7299307791557,-115.86175111262,-9.92453123330913));
#29338=CARTESIAN_POINT('Ctrl Pts',(-8.59489616871569,-115.68675111262,-4.96226561664425));
#29339=CARTESIAN_POINT('Ctrl Pts',(-11.4598615582757,-115.51175111262,2.06368086793017E-11));
#29340=CARTESIAN_POINT('Ctrl Pts',(-8.59489616869782,-115.33675111262,4.9622656166752));
#29341=CARTESIAN_POINT('Ctrl Pts',(-5.72993077911996,-115.16175111262,9.92453123332977));
#29342=CARTESIAN_POINT('Ctrl Pts',(1.7871392867044E-11,-114.98675111262,
9.92453123331945));
#29343=CARTESIAN_POINT('Ctrl Pts',(5.7299307791557,-114.81175111262,9.92453123330913));
#29344=CARTESIAN_POINT('Ctrl Pts',(8.59489616871569,-114.63675111262,4.96226561664425));
#29345=CARTESIAN_POINT('Ctrl Pts',(11.4598615582757,-114.46175111262,-2.06354052510241E-11));
#29346=CARTESIAN_POINT('Ctrl Pts',(8.59489616869782,-114.28675111262,-4.9622656166752));
#29347=CARTESIAN_POINT('Ctrl Pts',(5.72993077911996,-114.11175111262,-9.92453123332976));
#29348=CARTESIAN_POINT('Ctrl Pts',(-1.78726082715848E-11,-113.93675111262,
-9.92453123331945));
#29349=CARTESIAN_POINT('Ctrl Pts',(-5.7299307791557,-113.76175111262,-9.92453123330913));
#29350=CARTESIAN_POINT('Ctrl Pts',(-8.59489616871569,-113.58675111262,-4.96226561664425));
#29351=CARTESIAN_POINT('Ctrl Pts',(-11.4598615582757,-113.41175111262,2.06368086793017E-11));
#29352=CARTESIAN_POINT('Ctrl Pts',(-8.59489616869782,-113.23675111262,4.9622656166752));
#29353=CARTESIAN_POINT('Ctrl Pts',(-5.72993077911996,-113.06175111262,9.92453123332977));
#29354=CARTESIAN_POINT('Ctrl Pts',(1.7871392867044E-11,-112.88675111262,
9.92453123331945));
#29355=CARTESIAN_POINT('Ctrl Pts',(5.7299307791557,-112.71175111262,9.92453123330913));
#29356=CARTESIAN_POINT('Ctrl Pts',(8.59489616871569,-112.53675111262,4.96226561664425));
#29357=CARTESIAN_POINT('Ctrl Pts',(11.4598615582757,-112.36175111262,-2.06354052510241E-11));
#29358=CARTESIAN_POINT('Ctrl Pts',(8.59489616869782,-112.18675111262,-4.9622656166752));
#29359=CARTESIAN_POINT('Ctrl Pts',(5.72993077911996,-112.01175111262,-9.92453123332976));
#29360=CARTESIAN_POINT('Ctrl Pts',(-1.78726082715848E-11,-111.83675111262,
-9.92453123331945));
#29361=CARTESIAN_POINT('Ctrl Pts',(-5.7299307791557,-111.66175111262,-9.92453123330913));
#29362=CARTESIAN_POINT('Ctrl Pts',(-8.59489616871569,-111.48675111262,-4.96226561664425));
#29363=CARTESIAN_POINT('Ctrl Pts',(-11.4598615582757,-111.31175111262,2.06368086793017E-11));
#29364=CARTESIAN_POINT('Ctrl Pts',(-8.59489616869782,-111.13675111262,4.9622656166752));
#29365=CARTESIAN_POINT('Ctrl Pts',(-5.72993077911996,-110.96175111262,9.92453123332977));
#29366=CARTESIAN_POINT('Ctrl Pts',(1.7871392867044E-11,-110.78675111262,
9.92453123331945));
#29367=CARTESIAN_POINT('Ctrl Pts',(5.7299307791557,-110.61175111262,9.92453123330913));
#29368=CARTESIAN_POINT('Ctrl Pts',(8.59489616871569,-110.43675111262,4.96226561664425));
#29369=CARTESIAN_POINT('Ctrl Pts',(11.4598615582757,-110.26175111262,-2.06354052510241E-11));
#29370=CARTESIAN_POINT('Ctrl Pts',(8.59489616869782,-110.08675111262,-4.9622656166752));
#29371=CARTESIAN_POINT('Ctrl Pts',(5.72993077911996,-109.91175111262,-9.92453123332976));
#29372=CARTESIAN_POINT('Ctrl Pts',(-1.78726082715848E-11,-109.73675111262,
-9.92453123331945));
#29373=CARTESIAN_POINT('Ctrl Pts',(-5.7299307791557,-109.56175111262,-9.92453123330913));
#29374=CARTESIAN_POINT('Ctrl Pts',(-8.59489616871569,-109.38675111262,-4.96226561664425));
#29375=CARTESIAN_POINT('Ctrl Pts',(-11.4598615582757,-109.21175111262,2.06368086793017E-11));
#29376=CARTESIAN_POINT('Ctrl Pts',(-8.59489616869782,-109.03675111262,4.9622656166752));
#29377=CARTESIAN_POINT('Ctrl Pts',(-5.72993077911996,-108.86175111262,9.92453123332977));
#29378=CARTESIAN_POINT('Ctrl Pts',(1.7871392867044E-11,-108.68675111262,
9.92453123331945));
#29379=CARTESIAN_POINT('Ctrl Pts',(5.7299307791557,-108.51175111262,9.92453123330913));
#29380=CARTESIAN_POINT('Ctrl Pts',(8.59489616871569,-108.33675111262,4.96226561664425));
#29381=CARTESIAN_POINT('Ctrl Pts',(11.4598615582757,-108.16175111262,-2.06354052510241E-11));
#29382=CARTESIAN_POINT('Ctrl Pts',(8.59489616869782,-107.98675111262,-4.9622656166752));
#29383=CARTESIAN_POINT('Ctrl Pts',(5.72993077911996,-107.81175111262,-9.92453123332976));
#29384=CARTESIAN_POINT('Ctrl Pts',(-1.78726082715848E-11,-107.63675111262,
-9.92453123331945));
#29385=CARTESIAN_POINT('Ctrl Pts',(-5.7299307791557,-107.46175111262,-9.92453123330913));
#29386=CARTESIAN_POINT('Ctrl Pts',(-8.59489616871569,-107.28675111262,-4.96226561664425));
#29387=CARTESIAN_POINT('Ctrl Pts',(-11.4598615582757,-107.11175111262,2.06368086793017E-11));
#29388=CARTESIAN_POINT('Ctrl Pts',(-8.59489616869782,-106.93675111262,4.9622656166752));
#29389=CARTESIAN_POINT('Ctrl Pts',(-5.72993077911996,-106.76175111262,9.92453123332977));
#29390=CARTESIAN_POINT('Ctrl Pts',(1.7871392867044E-11,-106.58675111262,
9.92453123331945));
#29391=CARTESIAN_POINT('Ctrl Pts',(5.7299307791557,-106.41175111262,9.92453123330913));
#29392=CARTESIAN_POINT('Ctrl Pts',(8.59489616871569,-106.23675111262,4.96226561664425));
#29393=CARTESIAN_POINT('Ctrl Pts',(11.4598615582757,-106.06175111262,-2.06354052510241E-11));
#29394=CARTESIAN_POINT('Ctrl Pts',(8.59489616869782,-105.88675111262,-4.9622656166752));
#29395=CARTESIAN_POINT('Ctrl Pts',(5.72993077911996,-105.71175111262,-9.92453123332976));
#29396=CARTESIAN_POINT('Ctrl Pts',(-1.78726082715848E-11,-105.53675111262,
-9.92453123331945));
#29397=CARTESIAN_POINT('Ctrl Pts',(-5.7299307791557,-105.36175111262,-9.92453123330913));
#29398=CARTESIAN_POINT('Ctrl Pts',(-8.59489616871569,-105.18675111262,-4.96226561664425));
#29399=CARTESIAN_POINT('Ctrl Pts',(-11.4598615582757,-105.01175111262,2.06368086793017E-11));
#29400=CARTESIAN_POINT('Ctrl Pts',(-8.59489616869782,-104.83675111262,4.9622656166752));
#29401=CARTESIAN_POINT('Ctrl Pts',(-5.72993077911996,-104.66175111262,9.92453123332977));
#29402=CARTESIAN_POINT('Ctrl Pts',(1.7871392867044E-11,-104.48675111262,
9.92453123331945));
#29403=CARTESIAN_POINT('Ctrl Pts',(5.7299307791557,-104.31175111262,9.92453123330913));
#29404=CARTESIAN_POINT('Ctrl Pts',(8.59489616871569,-104.13675111262,4.96226561664425));
#29405=CARTESIAN_POINT('Ctrl Pts',(11.4598615582757,-103.96175111262,-2.06354052510241E-11));
#29406=CARTESIAN_POINT('Ctrl Pts',(8.59489616869782,-103.78675111262,-4.9622656166752));
#29407=CARTESIAN_POINT('Ctrl Pts',(5.72993077911996,-103.61175111262,-9.92453123332976));
#29408=CARTESIAN_POINT('Ctrl Pts',(-1.78726082715848E-11,-103.43675111262,
-9.92453123331945));
#29409=CARTESIAN_POINT('Ctrl Pts',(-5.7299307791557,-103.26175111262,-9.92453123330913));
#29410=CARTESIAN_POINT('Ctrl Pts',(-8.59489616871569,-103.08675111262,-4.96226561664425));
#29411=CARTESIAN_POINT('Ctrl Pts',(-11.4598615582757,-102.91175111262,2.06368086793017E-11));
#29412=CARTESIAN_POINT('Ctrl Pts',(-8.59489616869782,-102.73675111262,4.9622656166752));
#29413=CARTESIAN_POINT('Ctrl Pts',(-5.72993077911996,-102.56175111262,9.92453123332977));
#29414=CARTESIAN_POINT('Ctrl Pts',(1.7871392867044E-11,-102.38675111262,
9.92453123331945));
#29415=CARTESIAN_POINT('Ctrl Pts',(5.7299307791557,-102.21175111262,9.92453123330913));
#29416=CARTESIAN_POINT('Ctrl Pts',(8.59489616871569,-102.03675111262,4.96226561664425));
#29417=CARTESIAN_POINT('Ctrl Pts',(11.4598615582757,-101.86175111262,-2.06354052510241E-11));
#29418=CARTESIAN_POINT('Ctrl Pts',(8.59489616869782,-101.68675111262,-4.9622656166752));
#29419=CARTESIAN_POINT('Ctrl Pts',(5.72993077911996,-101.51175111262,-9.92453123332976));
#29420=CARTESIAN_POINT('Ctrl Pts',(-1.78726082715848E-11,-101.33675111262,
-9.92453123331945));
#29421=CARTESIAN_POINT('Ctrl Pts',(-5.7299307791557,-101.16175111262,-9.92453123330913));
#29422=CARTESIAN_POINT('Ctrl Pts',(-8.59489616871569,-100.98675111262,-4.96226561664425));
#29423=CARTESIAN_POINT('Ctrl Pts',(-11.4598615582757,-100.81175111262,2.06368086793017E-11));
#29424=CARTESIAN_POINT('Ctrl Pts',(-8.59489616869782,-100.63675111262,4.9622656166752));
#29425=CARTESIAN_POINT('Ctrl Pts',(-5.72993077911996,-100.46175111262,9.92453123332977));
#29426=CARTESIAN_POINT('Ctrl Pts',(1.7871392867044E-11,-100.28675111262,
9.92453123331945));
#29427=CARTESIAN_POINT('Ctrl Pts',(5.7299307791557,-100.11175111262,9.92453123330913));
#29428=CARTESIAN_POINT('Ctrl Pts',(8.59489616871569,-99.9367511126202,4.96226561664425));
#29429=CARTESIAN_POINT('Ctrl Pts',(11.4598615582757,-99.7617511126202,-2.06354052510241E-11));
#29430=CARTESIAN_POINT('Ctrl Pts',(8.59489616869782,-99.5867511126202,-4.9622656166752));
#29431=CARTESIAN_POINT('Ctrl Pts',(5.72993077911996,-99.4117511126202,-9.92453123332976));
#29432=CARTESIAN_POINT('Ctrl Pts',(-1.78726082715848E-11,-99.2367511126202,
-9.92453123331945));
#29433=CARTESIAN_POINT('Ctrl Pts',(-5.7299307791557,-99.0617511126202,-9.92453123330913));
#29434=CARTESIAN_POINT('Ctrl Pts',(-8.59489616871569,-98.8867511126202,
-4.96226561664425));
#29435=CARTESIAN_POINT('Ctrl Pts',(-11.4598615582757,-98.7117511126202,
2.06368086793017E-11));
#29436=CARTESIAN_POINT('Ctrl Pts',(-8.59489616869782,-98.5367511126202,
4.9622656166752));
#29437=CARTESIAN_POINT('Ctrl Pts',(-5.72993077911996,-98.3617511126202,
9.92453123332977));
#29438=CARTESIAN_POINT('Ctrl Pts',(1.7871392867044E-11,-98.1867511126202,
9.92453123331945));
#29439=CARTESIAN_POINT('Ctrl Pts',(5.7299307791557,-98.0117511126202,9.92453123330913));
#29440=CARTESIAN_POINT('Ctrl Pts',(8.59489616871569,-97.8367511126202,4.96226561664425));
#29441=CARTESIAN_POINT('Ctrl Pts',(11.4598615582757,-97.6617511126202,-2.06354052510241E-11));
#29442=CARTESIAN_POINT('Ctrl Pts',(8.59489616869782,-97.4867511126202,-4.9622656166752));
#29443=CARTESIAN_POINT('Ctrl Pts',(5.72993077911996,-97.3117511126202,-9.92453123332976));
#29444=CARTESIAN_POINT('Ctrl Pts',(-1.78726082715848E-11,-97.1367511126202,
-9.92453123331945));
#29445=CARTESIAN_POINT('Ctrl Pts',(-5.7299307791557,-96.9617511126202,-9.92453123330913));
#29446=CARTESIAN_POINT('Ctrl Pts',(-8.59489616871569,-96.7867511126202,
-4.96226561664425));
#29447=CARTESIAN_POINT('Ctrl Pts',(-11.4598615582757,-96.6117511126202,
2.06368086793017E-11));
#29448=CARTESIAN_POINT('Ctrl Pts',(-8.59489616869782,-96.4367511126202,
4.9622656166752));
#29449=CARTESIAN_POINT('Ctrl Pts',(-5.72993077911996,-96.2617511126202,
9.92453123332977));
#29450=CARTESIAN_POINT('Ctrl Pts',(1.7871392867044E-11,-96.0867511126202,
9.92453123331945));
#29451=CARTESIAN_POINT('Ctrl Pts',(5.7299307791557,-95.9117511126202,9.92453123330913));
#29452=CARTESIAN_POINT('Ctrl Pts',(8.59489616871569,-95.7367511126202,4.96226561664425));
#29453=CARTESIAN_POINT('Ctrl Pts',(11.4598615582757,-95.5617511126202,-2.06354052510241E-11));
#29454=CARTESIAN_POINT('Ctrl Pts',(8.59489616869782,-95.3867511126202,-4.9622656166752));
#29455=CARTESIAN_POINT('Ctrl Pts',(5.72993077911996,-95.2117511126202,-9.92453123332976));
#29456=CARTESIAN_POINT('Ctrl Pts',(-1.78726082715848E-11,-95.0367511126202,
-9.92453123331945));
#29457=CARTESIAN_POINT('Ctrl Pts',(-5.7299307791557,-94.8617511126203,-9.92453123330913));
#29458=CARTESIAN_POINT('Ctrl Pts',(-8.59489616871569,-94.6867511126202,
-4.96226561664425));
#29459=CARTESIAN_POINT('Ctrl Pts',(-11.4598615582757,-94.5117511126202,
2.06368086793017E-11));
#29460=CARTESIAN_POINT('Ctrl Pts',(-8.59489616869782,-94.3367511126202,
4.9622656166752));
#29461=CARTESIAN_POINT('Ctrl Pts',(-5.72993077911996,-94.1617511126202,
9.92453123332977));
#29462=CARTESIAN_POINT('Ctrl Pts',(1.7871392867044E-11,-93.9867511126202,
9.92453123331945));
#29463=CARTESIAN_POINT('Ctrl Pts',(5.7299307791557,-93.8117511126202,9.92453123330913));
#29464=CARTESIAN_POINT('Ctrl Pts',(8.59489616871569,-93.6367511126202,4.96226561664425));
#29465=CARTESIAN_POINT('Ctrl Pts',(11.4598615582757,-93.4617511126202,-2.06354052510241E-11));
#29466=CARTESIAN_POINT('Ctrl Pts',(8.59489616869782,-93.2867511126202,-4.9622656166752));
#29467=CARTESIAN_POINT('Ctrl Pts',(5.72993077911996,-93.1117511126202,-9.92453123332976));
#29468=CARTESIAN_POINT('Ctrl Pts',(-1.78726082715848E-11,-92.9367511126202,
-9.92453123331945));
#29469=CARTESIAN_POINT('Ctrl Pts',(-5.7299307791557,-92.7617511126202,-9.92453123330913));
#29470=CARTESIAN_POINT('Ctrl Pts',(-8.59489616871569,-92.5867511126202,
-4.96226561664425));
#29471=CARTESIAN_POINT('Ctrl Pts',(-11.4598615582757,-92.4117511126202,
2.06368086793017E-11));
#29472=CARTESIAN_POINT('Ctrl Pts',(-8.59489616869782,-92.2367511126202,
4.9622656166752));
#29473=CARTESIAN_POINT('Ctrl Pts',(-5.72993077911996,-92.0617511126202,
9.92453123332977));
#29474=CARTESIAN_POINT('Ctrl Pts',(1.7871392867044E-11,-91.8867511126202,
9.92453123331945));
#29475=CARTESIAN_POINT('Ctrl Pts',(5.7299307791557,-91.7117511126202,9.92453123330913));
#29476=CARTESIAN_POINT('Ctrl Pts',(8.59489616871569,-91.5367511126202,4.96226561664425));
#29477=CARTESIAN_POINT('Ctrl Pts',(11.4598615582757,-91.3617511126203,-2.06354052510241E-11));
#29478=CARTESIAN_POINT('Ctrl Pts',(8.59489616869782,-91.1867511126202,-4.9622656166752));
#29479=CARTESIAN_POINT('Ctrl Pts',(5.72993077911996,-91.0117511126202,-9.92453123332976));
#29480=CARTESIAN_POINT('Ctrl Pts',(-1.78726082715848E-11,-90.8367511126202,
-9.92453123331945));
#29481=CARTESIAN_POINT('Ctrl Pts',(-5.7299307791557,-90.6617511126203,-9.92453123330913));
#29482=CARTESIAN_POINT('Ctrl Pts',(-8.59489616871569,-90.4867511126203,
-4.96226561664425));
#29483=CARTESIAN_POINT('Ctrl Pts',(-11.4598615582757,-90.3117511126202,
2.06368086793017E-11));
#29484=CARTESIAN_POINT('Ctrl Pts',(-8.59489616869782,-90.1367511126202,
4.9622656166752));
#29485=CARTESIAN_POINT('Ctrl Pts',(-5.72993077911996,-89.9617511126202,
9.92453123332977));
#29486=CARTESIAN_POINT('Ctrl Pts',(1.7871392867044E-11,-89.7867511126202,
9.92453123331945));
#29487=CARTESIAN_POINT('Ctrl Pts',(5.7299307791557,-89.6117511126202,9.92453123330913));
#29488=CARTESIAN_POINT('Ctrl Pts',(8.59489616871569,-89.4367511126202,4.96226561664425));
#29489=CARTESIAN_POINT('Ctrl Pts',(11.4598615582757,-89.2617511126202,-2.06354052510241E-11));
#29490=CARTESIAN_POINT('Ctrl Pts',(8.59489616869782,-89.0867511126202,-4.9622656166752));
#29491=CARTESIAN_POINT('Ctrl Pts',(5.72993077911996,-88.9117511126202,-9.92453123332976));
#29492=CARTESIAN_POINT('Ctrl Pts',(-1.78726082715848E-11,-88.7367511126203,
-9.92453123331945));
#29493=CARTESIAN_POINT('Ctrl Pts',(-5.7299307791557,-88.5617511126202,-9.92453123330913));
#29494=CARTESIAN_POINT('Ctrl Pts',(-8.59489616871569,-88.3867511126202,
-4.96226561664425));
#29495=CARTESIAN_POINT('Ctrl Pts',(-11.4598615582757,-88.2117511126203,
2.06368086793017E-11));
#29496=CARTESIAN_POINT('Ctrl Pts',(-8.59489616869782,-88.0367511126202,
4.9622656166752));
#29497=CARTESIAN_POINT('Ctrl Pts',(-5.72993077911996,-87.8617511126202,
9.92453123332977));
#29498=CARTESIAN_POINT('Ctrl Pts',(1.7871392867044E-11,-87.6867511126203,
9.92453123331945));
#29499=CARTESIAN_POINT('Ctrl Pts',(5.7299307791557,-87.5117511126203,9.92453123330913));
#29500=CARTESIAN_POINT('Ctrl Pts',(8.59489616871569,-87.3367511126202,4.96226561664425));
#29501=CARTESIAN_POINT('Ctrl Pts',(11.4598615582757,-87.1617511126203,-2.06354052510241E-11));
#29502=CARTESIAN_POINT('Ctrl Pts',(8.59489616869782,-86.9867511126203,-4.9622656166752));
#29503=CARTESIAN_POINT('Ctrl Pts',(5.72993077911996,-86.8117511126202,-9.92453123332976));
#29504=CARTESIAN_POINT('Ctrl Pts',(-1.78726082715848E-11,-86.6367511126202,
-9.92453123331945));
#29505=CARTESIAN_POINT('Ctrl Pts',(-5.7299307791557,-86.4617511126202,-9.92453123330913));
#29506=CARTESIAN_POINT('Ctrl Pts',(-8.59489616871569,-86.2867511126203,
-4.96226561664425));
#29507=CARTESIAN_POINT('Ctrl Pts',(-11.4598615582757,-86.1117511126202,
2.06368086793017E-11));
#29508=CARTESIAN_POINT('Ctrl Pts',(-8.59489616869782,-85.9367511126203,
4.9622656166752));
#29509=CARTESIAN_POINT('Ctrl Pts',(-5.72993077911996,-85.7617511126202,
9.92453123332977));
#29510=CARTESIAN_POINT('Ctrl Pts',(1.7871392867044E-11,-85.5867511126202,
9.92453123331945));
#29511=CARTESIAN_POINT('Ctrl Pts',(5.7299307791557,-85.4117511126203,9.92453123330913));
#29512=CARTESIAN_POINT('Ctrl Pts',(8.59489616871569,-85.2367511126202,4.96226561664425));
#29513=CARTESIAN_POINT('Ctrl Pts',(11.4598615582757,-85.0617511126202,-2.06354052510241E-11));
#29514=CARTESIAN_POINT('Ctrl Pts',(8.59489616869782,-84.8867511126203,-4.9622656166752));
#29515=CARTESIAN_POINT('Ctrl Pts',(5.72993077911996,-84.7117511126202,-9.92453123332976));
#29516=CARTESIAN_POINT('Ctrl Pts',(-1.78726082715848E-11,-84.5367511126202,
-9.92453123331945));
#29517=CARTESIAN_POINT('Ctrl Pts',(-5.7299307791557,-84.3617511126203,-9.92453123330913));
#29518=CARTESIAN_POINT('Ctrl Pts',(-8.59489616871569,-84.1867511126203,
-4.96226561664425));
#29519=CARTESIAN_POINT('Ctrl Pts',(-11.4598615582757,-84.0117511126203,
2.06368086793017E-11));
#29520=CARTESIAN_POINT('Ctrl Pts',(-8.59489616869782,-83.8367511126203,
4.9622656166752));
#29521=CARTESIAN_POINT('Ctrl Pts',(-5.72993077911996,-83.6617511126203,
9.92453123332977));
#29522=CARTESIAN_POINT('Ctrl Pts',(1.7871392867044E-11,-83.4867511126202,
9.92453123331945));
#29523=CARTESIAN_POINT('Ctrl Pts',(5.7299307791557,-83.3117511126203,9.92453123330913));
#29524=CARTESIAN_POINT('Ctrl Pts',(8.59489616871569,-83.1367511126203,4.96226561664425));
#29525=CARTESIAN_POINT('Ctrl Pts',(11.4598615582757,-82.9617511126203,-2.06354052510241E-11));
#29526=CARTESIAN_POINT('Ctrl Pts',(8.59489616869782,-82.7867511126203,-4.9622656166752));
#29527=CARTESIAN_POINT('Ctrl Pts',(5.72993077911996,-82.6117511126203,-9.92453123332976));
#29528=CARTESIAN_POINT('Ctrl Pts',(-1.78726082715848E-11,-82.4367511126202,
-9.92453123331945));
#29529=CARTESIAN_POINT('Ctrl Pts',(-5.7299307791557,-82.2617511126202,-9.92453123330913));
#29530=CARTESIAN_POINT('Ctrl Pts',(-8.59489616871569,-82.0867511126203,
-4.96226561664425));
#29531=CARTESIAN_POINT('Ctrl Pts',(-11.4598615582757,-81.9117511126203,
2.06368086793017E-11));
#29532=CARTESIAN_POINT('Ctrl Pts',(-8.59489616869782,-81.7367511126203,
4.9622656166752));
#29533=CARTESIAN_POINT('Ctrl Pts',(-5.72993077911996,-81.5617511126202,
9.92453123332977));
#29534=CARTESIAN_POINT('Ctrl Pts',(1.7871392867044E-11,-81.3867511126203,
9.92453123331945));
#29535=CARTESIAN_POINT('Ctrl Pts',(5.7299307791557,-81.2117511126202,9.92453123330913));
#29536=CARTESIAN_POINT('Ctrl Pts',(8.59489616871569,-81.0367511126203,4.96226561664425));
#29537=CARTESIAN_POINT('Ctrl Pts',(11.4598615582757,-80.8617511126203,-2.06354052510241E-11));
#29538=CARTESIAN_POINT('Ctrl Pts',(8.59489616869782,-80.6867511126202,-4.9622656166752));
#29539=CARTESIAN_POINT('Ctrl Pts',(5.72993077911996,-80.5117511126203,-9.92453123332976));
#29540=CARTESIAN_POINT('Ctrl Pts',(-1.78726082715848E-11,-80.3367511126203,
-9.92453123331945));
#29541=CARTESIAN_POINT('Ctrl Pts',(-5.7299307791557,-80.1617511126202,-9.92453123330913));
#29542=CARTESIAN_POINT('Ctrl Pts',(-8.59489616871569,-79.9867511126203,
-4.96226561664425));
#29543=CARTESIAN_POINT('Ctrl Pts',(-11.4598615582757,-79.8117511126203,
2.06368086793017E-11));
#29544=CARTESIAN_POINT('Ctrl Pts',(-8.59489616869782,-79.6367511126202,
4.9622656166752));
#29545=CARTESIAN_POINT('Ctrl Pts',(-5.72993077911996,-79.4617511126203,
9.92453123332977));
#29546=CARTESIAN_POINT('Ctrl Pts',(1.7871392867044E-11,-79.2867511126203,
9.92453123331945));
#29547=CARTESIAN_POINT('Ctrl Pts',(5.7299307791557,-79.1117511126203,9.92453123330913));
#29548=CARTESIAN_POINT('Ctrl Pts',(8.59489616871569,-78.9367511126203,4.96226561664425));
#29549=CARTESIAN_POINT('Ctrl Pts',(11.4598615582757,-78.7617511126203,-2.06354052510241E-11));
#29550=CARTESIAN_POINT('Ctrl Pts',(8.59489616869782,-78.5867511126203,-4.9622656166752));
#29551=CARTESIAN_POINT('Ctrl Pts',(5.72993077911996,-78.4117511126203,-9.92453123332976));
#29552=CARTESIAN_POINT('Ctrl Pts',(-1.78726082715848E-11,-78.2367511126203,
-9.92453123331945));
#29553=CARTESIAN_POINT('Ctrl Pts',(-5.7299307791557,-78.0617511126203,-9.92453123330913));
#29554=CARTESIAN_POINT('Ctrl Pts',(-8.59489616871569,-77.8867511126202,
-4.96226561664425));
#29555=CARTESIAN_POINT('Ctrl Pts',(-11.4598615582757,-77.7117511126203,
2.06368086793017E-11));
#29556=CARTESIAN_POINT('Ctrl Pts',(-8.59489616869782,-77.5367511126203,
4.9622656166752));
#29557=CARTESIAN_POINT('Ctrl Pts',(-5.72993077911996,-77.3617511126203,
9.92453123332977));
#29558=CARTESIAN_POINT('Ctrl Pts',(1.7871392867044E-11,-77.1867511126203,
9.92453123331945));
#29559=CARTESIAN_POINT('Ctrl Pts',(5.7299307791557,-77.0117511126203,9.92453123330913));
#29560=CARTESIAN_POINT('Ctrl Pts',(8.59489616871569,-76.8367511126202,4.96226561664425));
#29561=CARTESIAN_POINT('Ctrl Pts',(11.4598615582757,-76.6617511126203,-2.06354052510241E-11));
#29562=CARTESIAN_POINT('Ctrl Pts',(8.59489616869782,-76.4867511126203,-4.9622656166752));
#29563=CARTESIAN_POINT('Ctrl Pts',(5.72993077911996,-76.3117511126203,-9.92453123332976));
#29564=CARTESIAN_POINT('Ctrl Pts',(-1.78726082715848E-11,-76.1367511126203,
-9.92453123331945));
#29565=CARTESIAN_POINT('Ctrl Pts',(-5.7299307791557,-75.9617511126203,-9.92453123330913));
#29566=CARTESIAN_POINT('Ctrl Pts',(-8.59489616871569,-75.7867511126203,
-4.96226561664425));
#29567=CARTESIAN_POINT('Ctrl Pts',(-11.4598615582757,-75.6117511126203,
2.06368086793017E-11));
#29568=CARTESIAN_POINT('Ctrl Pts',(-8.59489616869782,-75.4367511126203,
4.9622656166752));
#29569=CARTESIAN_POINT('Ctrl Pts',(-5.72993077911996,-75.2617511126203,
9.92453123332977));
#29570=CARTESIAN_POINT('Ctrl Pts',(1.7871392867044E-11,-75.0867511126203,
9.92453123331945));
#29571=CARTESIAN_POINT('Ctrl Pts',(5.7299307791557,-74.9117511126203,9.92453123330913));
#29572=CARTESIAN_POINT('Ctrl Pts',(8.59489616871569,-74.7367511126203,4.96226561664425));
#29573=CARTESIAN_POINT('Ctrl Pts',(11.4598615582757,-74.5617511126203,-2.06354052510241E-11));
#29574=CARTESIAN_POINT('Ctrl Pts',(8.59489616869782,-74.3867511126203,-4.9622656166752));
#29575=CARTESIAN_POINT('Ctrl Pts',(5.72993077911996,-74.2117511126203,-9.92453123332976));
#29576=CARTESIAN_POINT('Ctrl Pts',(-1.78726082715848E-11,-74.0367511126203,
-9.92453123331945));
#29577=CARTESIAN_POINT('Ctrl Pts',(-5.7299307791557,-73.8617511126203,-9.92453123330913));
#29578=CARTESIAN_POINT('Ctrl Pts',(-8.59489616871569,-73.6867511126203,
-4.96226561664425));
#29579=CARTESIAN_POINT('Ctrl Pts',(-11.4598615582757,-73.5117511126203,
2.06368086793017E-11));
#29580=CARTESIAN_POINT('Ctrl Pts',(-8.59489616869782,-73.3367511126203,
4.9622656166752));
#29581=CARTESIAN_POINT('Ctrl Pts',(-5.72993077911996,-73.1617511126203,
9.92453123332977));
#29582=CARTESIAN_POINT('Ctrl Pts',(1.7871392867044E-11,-72.9867511126203,
9.92453123331945));
#29583=CARTESIAN_POINT('Ctrl Pts',(5.7299307791557,-72.8117511126203,9.92453123330913));
#29584=CARTESIAN_POINT('Ctrl Pts',(8.59489616871569,-72.6367511126203,4.96226561664425));
#29585=CARTESIAN_POINT('Ctrl Pts',(11.4598615582757,-72.4617511126203,-2.06354052510241E-11));
#29586=CARTESIAN_POINT('Ctrl Pts',(8.59489616869782,-72.2867511126203,-4.9622656166752));
#29587=CARTESIAN_POINT('Ctrl Pts',(5.72993077911996,-72.1117511126203,-9.92453123332976));
#29588=CARTESIAN_POINT('Ctrl Pts',(-1.78726082715848E-11,-71.9367511126203,
-9.92453123331945));
#29589=CARTESIAN_POINT('Ctrl Pts',(-5.7299307791557,-71.7617511126203,-9.92453123330913));
#29590=CARTESIAN_POINT('Ctrl Pts',(-8.59489616871569,-71.5867511126203,
-4.96226561664425));
#29591=CARTESIAN_POINT('Ctrl Pts',(-11.4598615582757,-71.4117511126203,
2.06368086793017E-11));
#29592=CARTESIAN_POINT('Ctrl Pts',(-8.59489616869782,-71.2367511126203,
4.9622656166752));
#29593=CARTESIAN_POINT('Ctrl Pts',(-5.72993077911996,-71.0617511126203,
9.92453123332977));
#29594=CARTESIAN_POINT('Ctrl Pts',(1.7871392867044E-11,-70.8867511126203,
9.92453123331945));
#29595=CARTESIAN_POINT('Ctrl Pts',(5.7299307791557,-70.7117511126203,9.92453123330913));
#29596=CARTESIAN_POINT('Ctrl Pts',(8.59489616871569,-70.5367511126203,4.96226561664425));
#29597=CARTESIAN_POINT('Ctrl Pts',(11.4598615582757,-70.3617511126203,-2.06354052510241E-11));
#29598=CARTESIAN_POINT('Ctrl Pts',(8.59489616869782,-70.1867511126203,-4.9622656166752));
#29599=CARTESIAN_POINT('Ctrl Pts',(5.72993077911996,-70.0117511126203,-9.92453123332976));
#29600=CARTESIAN_POINT('Ctrl Pts',(-1.78726082715848E-11,-69.8367511126203,
-9.92453123331945));
#29601=CARTESIAN_POINT('Ctrl Pts',(-5.7299307791557,-69.6617511126203,-9.92453123330913));
#29602=CARTESIAN_POINT('Ctrl Pts',(-8.59489616871569,-69.4867511126203,
-4.96226561664425));
#29603=CARTESIAN_POINT('Ctrl Pts',(-11.4598615582757,-69.3117511126203,
2.06368086793017E-11));
#29604=CARTESIAN_POINT('Ctrl Pts',(-8.59489616869782,-69.1367511126203,
4.9622656166752));
#29605=CARTESIAN_POINT('Ctrl Pts',(-5.72993077911996,-68.9617511126203,
9.92453123332977));
#29606=CARTESIAN_POINT('Ctrl Pts',(1.7871392867044E-11,-68.7867511126203,
9.92453123331945));
#29607=CARTESIAN_POINT('Ctrl Pts',(5.7299307791557,-68.6117511126203,9.92453123330913));
#29608=CARTESIAN_POINT('Ctrl Pts',(8.59489616871569,-68.4367511126203,4.96226561664425));
#29609=CARTESIAN_POINT('Ctrl Pts',(11.4598615582757,-68.2617511126203,-2.06354052510241E-11));
#29610=CARTESIAN_POINT('Ctrl Pts',(8.59489616869782,-68.0867511126203,-4.9622656166752));
#29611=CARTESIAN_POINT('Ctrl Pts',(5.72993077911996,-67.9117511126203,-9.92453123332976));
#29612=CARTESIAN_POINT('Ctrl Pts',(-1.78726082715848E-11,-67.7367511126203,
-9.92453123331945));
#29613=CARTESIAN_POINT('Ctrl Pts',(-5.7299307791557,-67.5617511126203,-9.92453123330913));
#29614=CARTESIAN_POINT('Ctrl Pts',(-8.59489616871569,-67.3867511126203,
-4.96226561664425));
#29615=CARTESIAN_POINT('Ctrl Pts',(-11.4598615582757,-67.2117511126203,
2.06368086793017E-11));
#29616=CARTESIAN_POINT('Ctrl Pts',(-8.59489616869782,-67.0367511126203,
4.9622656166752));
#29617=CARTESIAN_POINT('Ctrl Pts',(-5.72993077911996,-66.8617511126203,
9.92453123332977));
#29618=CARTESIAN_POINT('Ctrl Pts',(1.7871392867044E-11,-66.6867511126203,
9.92453123331945));
#29619=CARTESIAN_POINT('Ctrl Pts',(5.7299307791557,-66.5117511126203,9.92453123330913));
#29620=CARTESIAN_POINT('Ctrl Pts',(8.59489616871569,-66.3367511126203,4.96226561664425));
#29621=CARTESIAN_POINT('Ctrl Pts',(11.4598615582757,-66.1617511126203,-2.06354052510241E-11));
#29622=CARTESIAN_POINT('Ctrl Pts',(8.59489616869782,-65.9867511126203,-4.9622656166752));
#29623=CARTESIAN_POINT('Ctrl Pts',(5.72993077911996,-65.8117511126203,-9.92453123332976));
#29624=CARTESIAN_POINT('Ctrl Pts',(-1.78726082715848E-11,-65.6367511126203,
-9.92453123331945));
#29625=CARTESIAN_POINT('Ctrl Pts',(-5.7299307791557,-65.4617511126203,-9.92453123330913));
#29626=CARTESIAN_POINT('Ctrl Pts',(-8.59489616871569,-65.2867511126203,
-4.96226561664425));
#29627=CARTESIAN_POINT('Ctrl Pts',(-11.4598615582757,-65.1117511126203,
2.06368086793017E-11));
#29628=CARTESIAN_POINT('Ctrl Pts',(-8.59489616869782,-64.9367511126203,
4.9622656166752));
#29629=CARTESIAN_POINT('Ctrl Pts',(-5.72993077911996,-64.7617511126203,
9.92453123332977));
#29630=CARTESIAN_POINT('Ctrl Pts',(1.7871392867044E-11,-64.5867511126203,
9.92453123331945));
#29631=CARTESIAN_POINT('Ctrl Pts',(5.7299307791557,-64.4117511126203,9.92453123330913));
#29632=CARTESIAN_POINT('Ctrl Pts',(8.59489616871569,-64.2367511126203,4.96226561664425));
#29633=CARTESIAN_POINT('Ctrl Pts',(11.4598615582757,-64.0617511126203,-2.06354052510241E-11));
#29634=CARTESIAN_POINT('Ctrl Pts',(8.59489616869782,-63.8867511126203,-4.9622656166752));
#29635=CARTESIAN_POINT('Ctrl Pts',(5.72993077911996,-63.7117511126203,-9.92453123332976));
#29636=CARTESIAN_POINT('Ctrl Pts',(-1.78726082715848E-11,-63.5367511126203,
-9.92453123331945));
#29637=CARTESIAN_POINT('Ctrl Pts',(-5.7299307791557,-63.3617511126203,-9.92453123330913));
#29638=CARTESIAN_POINT('Ctrl Pts',(-8.59489616871569,-63.1867511126203,
-4.96226561664425));
#29639=CARTESIAN_POINT('Ctrl Pts',(-11.4598615582757,-63.0117511126203,
2.06368086793017E-11));
#29640=CARTESIAN_POINT('Ctrl Pts',(-8.59489616869782,-62.8367511126203,
4.9622656166752));
#29641=CARTESIAN_POINT('Ctrl Pts',(-5.72993077911996,-62.6617511126203,
9.92453123332977));
#29642=CARTESIAN_POINT('Ctrl Pts',(1.7871392867044E-11,-62.4867511126203,
9.92453123331945));
#29643=CARTESIAN_POINT('Ctrl Pts',(5.7299307791557,-62.3117511126203,9.92453123330913));
#29644=CARTESIAN_POINT('Ctrl Pts',(8.59489616871569,-62.1367511126203,4.96226561664425));
#29645=CARTESIAN_POINT('Ctrl Pts',(11.4598615582757,-61.9617511126203,-2.06354052510241E-11));
#29646=CARTESIAN_POINT('Ctrl Pts',(8.59489616869782,-61.7867511126203,-4.9622656166752));
#29647=CARTESIAN_POINT('Ctrl Pts',(5.72993077911996,-61.6117511126203,-9.92453123332976));
#29648=CARTESIAN_POINT('Ctrl Pts',(-1.78726082715848E-11,-61.4367511126203,
-9.92453123331945));
#29649=CARTESIAN_POINT('Ctrl Pts',(-5.7299307791557,-61.2617511126203,-9.92453123330913));
#29650=CARTESIAN_POINT('Ctrl Pts',(-8.59489616871569,-61.0867511126203,
-4.96226561664425));
#29651=CARTESIAN_POINT('Ctrl Pts',(-11.4598615582757,-60.9117511126203,
2.06368086793017E-11));
#29652=CARTESIAN_POINT('Ctrl Pts',(-8.59489616869782,-60.7367511126203,
4.9622656166752));
#29653=CARTESIAN_POINT('Ctrl Pts',(-5.72993077911996,-60.5617511126203,
9.92453123332977));
#29654=CARTESIAN_POINT('Ctrl Pts',(1.7871392867044E-11,-60.3867511126203,
9.92453123331945));
#29655=CARTESIAN_POINT('Ctrl Pts',(5.7299307791557,-60.2117511126203,9.92453123330913));
#29656=CARTESIAN_POINT('Ctrl Pts',(8.59489616871569,-60.0367511126203,4.96226561664425));
#29657=CARTESIAN_POINT('Ctrl Pts',(11.4598615582757,-59.8617511126203,-2.06354052510241E-11));
#29658=CARTESIAN_POINT('Ctrl Pts',(8.59489616869782,-59.6867511126203,-4.9622656166752));
#29659=CARTESIAN_POINT('Ctrl Pts',(5.72993077911996,-59.5117511126203,-9.92453123332976));
#29660=CARTESIAN_POINT('Ctrl Pts',(-1.78726082715848E-11,-59.3367511126203,
-9.92453123331945));
#29661=CARTESIAN_POINT('Ctrl Pts',(-5.7299307791557,-59.1617511126203,-9.92453123330913));
#29662=CARTESIAN_POINT('Ctrl Pts',(-8.59489616871569,-58.9867511126203,
-4.96226561664425));
#29663=CARTESIAN_POINT('Ctrl Pts',(-11.4598615582757,-58.8117511126203,
2.06368086793017E-11));
#29664=CARTESIAN_POINT('Ctrl Pts',(-8.59489616869782,-58.6367511126203,
4.9622656166752));
#29665=CARTESIAN_POINT('Ctrl Pts',(-5.72993077911996,-58.4617511126203,
9.92453123332977));
#29666=CARTESIAN_POINT('Ctrl Pts',(1.7871392867044E-11,-58.2867511126203,
9.92453123331945));
#29667=CARTESIAN_POINT('Ctrl Pts',(5.7299307791557,-58.1117511126203,9.92453123330913));
#29668=CARTESIAN_POINT('Ctrl Pts',(8.59489616871569,-57.9367511126203,4.96226561664425));
#29669=CARTESIAN_POINT('Ctrl Pts',(11.4598615582757,-57.7617511126203,-2.06354052510241E-11));
#29670=CARTESIAN_POINT('Ctrl Pts',(8.59489616869782,-57.5867511126203,-4.9622656166752));
#29671=CARTESIAN_POINT('Ctrl Pts',(5.72993077911996,-57.4117511126203,-9.92453123332976));
#29672=CARTESIAN_POINT('Ctrl Pts',(-1.78726082715848E-11,-57.2367511126203,
-9.92453123331945));
#29673=CARTESIAN_POINT('Ctrl Pts',(-5.7299307791557,-57.0617511126203,-9.92453123330913));
#29674=CARTESIAN_POINT('Ctrl Pts',(-8.59489616871569,-56.8867511126203,
-4.96226561664425));
#29675=CARTESIAN_POINT('Ctrl Pts',(-11.4598615582757,-56.7117511126203,
2.06368086793017E-11));
#29676=CARTESIAN_POINT('Ctrl Pts',(-8.59489616869782,-56.5367511126203,
4.9622656166752));
#29677=CARTESIAN_POINT('Ctrl Pts',(-5.72993077911996,-56.3617511126203,
9.92453123332977));
#29678=CARTESIAN_POINT('Ctrl Pts',(1.7871392867044E-11,-56.1867511126203,
9.92453123331945));
#29679=CARTESIAN_POINT('Ctrl Pts',(5.7299307791557,-56.0117511126203,9.92453123330913));
#29680=CARTESIAN_POINT('Ctrl Pts',(8.59489616871569,-55.8367511126203,4.96226561664425));
#29681=CARTESIAN_POINT('Ctrl Pts',(11.4598615582757,-55.6617511126203,-2.06354052510241E-11));
#29682=CARTESIAN_POINT('Ctrl Pts',(8.59489616869782,-55.4867511126203,-4.9622656166752));
#29683=CARTESIAN_POINT('Ctrl Pts',(5.72993077911996,-55.3117511126203,-9.92453123332976));
#29684=CARTESIAN_POINT('Ctrl Pts',(-1.78726082715848E-11,-55.1367511126203,
-9.92453123331945));
#29685=CARTESIAN_POINT('Ctrl Pts',(-5.7299307791557,-54.9617511126203,-9.92453123330913));
#29686=CARTESIAN_POINT('Ctrl Pts',(-8.59489616871569,-54.7867511126203,
-4.96226561664425));
#29687=CARTESIAN_POINT('Ctrl Pts',(-11.4598615582757,-54.6117511126203,
2.06368086793017E-11));
#29688=CARTESIAN_POINT('Ctrl Pts',(-8.59489616869782,-54.4367511126203,
4.9622656166752));
#29689=CARTESIAN_POINT('Ctrl Pts',(-5.72993077911996,-54.2617511126203,
9.92453123332977));
#29690=CARTESIAN_POINT('Ctrl Pts',(1.7871392867044E-11,-54.0867511126203,
9.92453123331945));
#29691=CARTESIAN_POINT('Ctrl Pts',(5.7299307791557,-53.9117511126203,9.92453123330913));
#29692=CARTESIAN_POINT('Ctrl Pts',(8.59489616871569,-53.7367511126203,4.96226561664425));
#29693=CARTESIAN_POINT('Ctrl Pts',(11.4598615582757,-53.5617511126203,-2.06354052510241E-11));
#29694=CARTESIAN_POINT('Ctrl Pts',(8.59489616869782,-53.3867511126203,-4.9622656166752));
#29695=CARTESIAN_POINT('Ctrl Pts',(5.72993077911996,-53.2117511126203,-9.92453123332976));
#29696=CARTESIAN_POINT('Ctrl Pts',(-1.78726082715848E-11,-53.0367511126203,
-9.92453123331945));
#29697=CARTESIAN_POINT('Ctrl Pts',(-5.7299307791557,-52.8617511126203,-9.92453123330913));
#29698=CARTESIAN_POINT('Ctrl Pts',(-8.59489616871569,-52.6867511126203,
-4.96226561664425));
#29699=CARTESIAN_POINT('Ctrl Pts',(-11.4598615582757,-52.5117511126203,
2.06368086793017E-11));
#29700=CARTESIAN_POINT('Ctrl Pts',(-8.59489616869782,-52.3367511126203,
4.9622656166752));
#29701=CARTESIAN_POINT('Ctrl Pts',(-5.72993077911996,-52.1617511126203,
9.92453123332977));
#29702=CARTESIAN_POINT('Ctrl Pts',(1.7871392867044E-11,-51.9867511126203,
9.92453123331945));
#29703=CARTESIAN_POINT('Ctrl Pts',(5.7299307791557,-51.8117511126203,9.92453123330913));
#29704=CARTESIAN_POINT('Ctrl Pts',(8.59489616871569,-51.6367511126203,4.96226561664425));
#29705=CARTESIAN_POINT('Ctrl Pts',(11.4598615582757,-51.4617511126203,-2.06354052510241E-11));
#29706=CARTESIAN_POINT('Ctrl Pts',(8.59489616869782,-51.2867511126203,-4.9622656166752));
#29707=CARTESIAN_POINT('Ctrl Pts',(5.72993077911996,-51.1117511126203,-9.92453123332976));
#29708=CARTESIAN_POINT('Ctrl Pts',(-1.78726082715848E-11,-50.9367511126203,
-9.92453123331945));
#29709=CARTESIAN_POINT('Ctrl Pts',(-5.7299307791557,-50.7617511126203,-9.92453123330913));
#29710=CARTESIAN_POINT('Ctrl Pts',(-8.59489616871569,-50.5867511126203,
-4.96226561664425));
#29711=CARTESIAN_POINT('Ctrl Pts',(-11.4598615582757,-50.4117511126203,
2.06368086793017E-11));
#29712=CARTESIAN_POINT('Ctrl Pts',(-8.59489616869782,-50.2367511126203,
4.9622656166752));
#29713=CARTESIAN_POINT('Ctrl Pts',(-5.72993077911996,-50.0617511126203,
9.92453123332977));
#29714=CARTESIAN_POINT('Ctrl Pts',(1.7871392867044E-11,-49.8867511126203,
9.92453123331945));
#29715=CARTESIAN_POINT('Ctrl Pts',(5.7299307791557,-49.7117511126203,9.92453123330913));
#29716=CARTESIAN_POINT('Ctrl Pts',(8.59489616871569,-49.5367511126203,4.96226561664425));
#29717=CARTESIAN_POINT('Ctrl Pts',(11.4598615582757,-49.3617511126203,-2.06354052510241E-11));
#29718=CARTESIAN_POINT('Ctrl Pts',(8.59489616869782,-49.1867511126203,-4.9622656166752));
#29719=CARTESIAN_POINT('Ctrl Pts',(5.72993077911996,-49.0117511126203,-9.92453123332976));
#29720=CARTESIAN_POINT('Ctrl Pts',(-1.78726082715848E-11,-48.8367511126203,
-9.92453123331945));
#29721=CARTESIAN_POINT('Ctrl Pts',(-5.7299307791557,-48.6617511126203,-9.92453123330913));
#29722=CARTESIAN_POINT('Ctrl Pts',(-8.59489616871569,-48.4867511126203,
-4.96226561664425));
#29723=CARTESIAN_POINT('Ctrl Pts',(-11.4598615582757,-48.3117511126203,
2.06368086793017E-11));
#29724=CARTESIAN_POINT('Ctrl Pts',(-8.59489616869782,-48.1367511126203,
4.9622656166752));
#29725=CARTESIAN_POINT('Ctrl Pts',(-5.72993077911996,-47.9617511126203,
9.92453123332977));
#29726=CARTESIAN_POINT('Ctrl Pts',(1.7871392867044E-11,-47.7867511126204,
9.92453123331945));
#29727=CARTESIAN_POINT('Ctrl Pts',(5.7299307791557,-47.6117511126203,9.92453123330913));
#29728=CARTESIAN_POINT('Ctrl Pts',(8.59489616871569,-47.4367511126203,4.96226561664425));
#29729=CARTESIAN_POINT('Ctrl Pts',(11.4598615582757,-47.2617511126203,-2.06354052510241E-11));
#29730=CARTESIAN_POINT('Ctrl Pts',(8.59489616869782,-47.0867511126203,-4.9622656166752));
#29731=CARTESIAN_POINT('Ctrl Pts',(5.72993077911996,-46.9117511126203,-9.92453123332976));
#29732=CARTESIAN_POINT('Ctrl Pts',(-1.78726082715848E-11,-46.7367511126204,
-9.92453123331945));
#29733=CARTESIAN_POINT('Ctrl Pts',(-5.7299307791557,-46.5617511126203,-9.92453123330913));
#29734=CARTESIAN_POINT('Ctrl Pts',(-8.59489616871569,-46.3867511126203,
-4.96226561664425));
#29735=CARTESIAN_POINT('Ctrl Pts',(-11.4598615582757,-46.2117511126203,
2.06368086793017E-11));
#29736=CARTESIAN_POINT('Ctrl Pts',(-8.59489616869782,-46.0367511126203,
4.9622656166752));
#29737=CARTESIAN_POINT('Ctrl Pts',(-5.72993077911996,-45.8617511126203,
9.92453123332977));
#29738=CARTESIAN_POINT('Ctrl Pts',(1.7871392867044E-11,-45.6867511126203,
9.92453123331945));
#29739=CARTESIAN_POINT('Ctrl Pts',(5.7299307791557,-45.5117511126203,9.92453123330913));
#29740=CARTESIAN_POINT('Ctrl Pts',(8.59489616871569,-45.3367511126203,4.96226561664425));
#29741=CARTESIAN_POINT('Ctrl Pts',(11.4598615582757,-45.1617511126203,-2.06354052510241E-11));
#29742=CARTESIAN_POINT('Ctrl Pts',(8.59489616869782,-44.9867511126203,-4.9622656166752));
#29743=CARTESIAN_POINT('Ctrl Pts',(5.72993077911996,-44.8117511126203,-9.92453123332976));
#29744=CARTESIAN_POINT('Ctrl Pts',(-1.78726082715848E-11,-44.6367511126203,
-9.92453123331945));
#29745=CARTESIAN_POINT('Ctrl Pts',(-1.51301075899711E-11,-213.943984254242,
-8.40164026751963));
#29746=CARTESIAN_POINT('Ctrl Pts',(-4.85068927010198,-213.768984254242,
-8.40164026751089));
#29747=CARTESIAN_POINT('Ctrl Pts',(-7.27603390513785,-213.593984254242,
-4.20082013374671));
#29748=CARTESIAN_POINT('Ctrl Pts',(-9.70137854017371,-213.418984254242,
1.74701493417668E-11));
#29749=CARTESIAN_POINT('Ctrl Pts',(-7.27603390512272,-213.243984254242,
4.20082013377291));
#29750=CARTESIAN_POINT('Ctrl Pts',(-4.85068927007173,-213.068984254242,
8.40164026752836));
#29751=CARTESIAN_POINT('Ctrl Pts',(1.5129078685785E-11,-212.893984254242,
8.40164026751963));
#29752=CARTESIAN_POINT('Ctrl Pts',(4.85068927010198,-212.718984254242,8.40164026751089));
#29753=CARTESIAN_POINT('Ctrl Pts',(7.27603390513785,-212.543984254242,4.20082013374671));
#29754=CARTESIAN_POINT('Ctrl Pts',(9.70137854017371,-212.368984254242,-1.74689612655491E-11));
#29755=CARTESIAN_POINT('Ctrl Pts',(7.27603390512272,-212.193984254242,-4.20082013377291));
#29756=CARTESIAN_POINT('Ctrl Pts',(4.85068927007173,-212.018984254242,-8.40164026752836));
#29757=CARTESIAN_POINT('Ctrl Pts',(-1.51301075899711E-11,-211.843984254242,
-8.40164026751963));
#29758=CARTESIAN_POINT('Ctrl Pts',(-4.85068927010198,-211.668984254242,
-8.40164026751089));
#29759=CARTESIAN_POINT('Ctrl Pts',(-7.27603390513785,-211.493984254242,
-4.20082013374671));
#29760=CARTESIAN_POINT('Ctrl Pts',(-9.70137854017371,-211.318984254242,
1.74701493417668E-11));
#29761=CARTESIAN_POINT('Ctrl Pts',(-7.27603390512272,-211.143984254242,
4.20082013377291));
#29762=CARTESIAN_POINT('Ctrl Pts',(-4.85068927007173,-210.968984254242,
8.40164026752836));
#29763=CARTESIAN_POINT('Ctrl Pts',(1.5129078685785E-11,-210.793984254242,
8.40164026751963));
#29764=CARTESIAN_POINT('Ctrl Pts',(4.85068927010198,-210.618984254242,8.40164026751089));
#29765=CARTESIAN_POINT('Ctrl Pts',(7.27603390513785,-210.443984254242,4.20082013374671));
#29766=CARTESIAN_POINT('Ctrl Pts',(9.70137854017371,-210.268984254242,-1.74689612655491E-11));
#29767=CARTESIAN_POINT('Ctrl Pts',(7.27603390512272,-210.093984254242,-4.20082013377291));
#29768=CARTESIAN_POINT('Ctrl Pts',(4.85068927007173,-209.918984254242,-8.40164026752836));
#29769=CARTESIAN_POINT('Ctrl Pts',(-1.51301075899711E-11,-209.743984254242,
-8.40164026751963));
#29770=CARTESIAN_POINT('Ctrl Pts',(-4.85068927010198,-209.568984254242,
-8.40164026751089));
#29771=CARTESIAN_POINT('Ctrl Pts',(-7.27603390513785,-209.393984254242,
-4.20082013374671));
#29772=CARTESIAN_POINT('Ctrl Pts',(-9.70137854017371,-209.218984254242,
1.74701493417668E-11));
#29773=CARTESIAN_POINT('Ctrl Pts',(-7.27603390512272,-209.043984254242,
4.20082013377291));
#29774=CARTESIAN_POINT('Ctrl Pts',(-4.85068927007173,-208.868984254242,
8.40164026752836));
#29775=CARTESIAN_POINT('Ctrl Pts',(1.5129078685785E-11,-208.693984254242,
8.40164026751963));
#29776=CARTESIAN_POINT('Ctrl Pts',(4.85068927010198,-208.518984254242,8.40164026751089));
#29777=CARTESIAN_POINT('Ctrl Pts',(7.27603390513785,-208.343984254242,4.20082013374671));
#29778=CARTESIAN_POINT('Ctrl Pts',(9.70137854017371,-208.168984254242,-1.74689612655491E-11));
#29779=CARTESIAN_POINT('Ctrl Pts',(7.27603390512272,-207.993984254242,-4.20082013377291));
#29780=CARTESIAN_POINT('Ctrl Pts',(4.85068927007173,-207.818984254242,-8.40164026752836));
#29781=CARTESIAN_POINT('Ctrl Pts',(-1.51301075899711E-11,-207.643984254242,
-8.40164026751963));
#29782=CARTESIAN_POINT('Ctrl Pts',(-4.85068927010198,-207.468984254242,
-8.40164026751089));
#29783=CARTESIAN_POINT('Ctrl Pts',(-7.27603390513785,-207.293984254242,
-4.20082013374671));
#29784=CARTESIAN_POINT('Ctrl Pts',(-9.70137854017371,-207.118984254242,
1.74701493417668E-11));
#29785=CARTESIAN_POINT('Ctrl Pts',(-7.27603390512272,-206.943984254242,
4.20082013377291));
#29786=CARTESIAN_POINT('Ctrl Pts',(-4.85068927007173,-206.768984254242,
8.40164026752836));
#29787=CARTESIAN_POINT('Ctrl Pts',(1.5129078685785E-11,-206.593984254242,
8.40164026751963));
#29788=CARTESIAN_POINT('Ctrl Pts',(4.85068927010198,-206.418984254242,8.40164026751089));
#29789=CARTESIAN_POINT('Ctrl Pts',(7.27603390513785,-206.243984254242,4.20082013374671));
#29790=CARTESIAN_POINT('Ctrl Pts',(9.70137854017371,-206.068984254242,-1.74689612655491E-11));
#29791=CARTESIAN_POINT('Ctrl Pts',(7.27603390512272,-205.893984254242,-4.20082013377291));
#29792=CARTESIAN_POINT('Ctrl Pts',(4.85068927007173,-205.718984254242,-8.40164026752836));
#29793=CARTESIAN_POINT('Ctrl Pts',(-1.51301075899711E-11,-205.543984254242,
-8.40164026751963));
#29794=CARTESIAN_POINT('Ctrl Pts',(-4.85068927010198,-205.368984254242,
-8.40164026751089));
#29795=CARTESIAN_POINT('Ctrl Pts',(-7.27603390513785,-205.193984254242,
-4.20082013374671));
#29796=CARTESIAN_POINT('Ctrl Pts',(-9.70137854017371,-205.018984254242,
1.74701493417668E-11));
#29797=CARTESIAN_POINT('Ctrl Pts',(-7.27603390512272,-204.843984254242,
4.20082013377291));
#29798=CARTESIAN_POINT('Ctrl Pts',(-4.85068927007173,-204.668984254242,
8.40164026752836));
#29799=CARTESIAN_POINT('Ctrl Pts',(1.5129078685785E-11,-204.493984254242,
8.40164026751963));
#29800=CARTESIAN_POINT('Ctrl Pts',(4.85068927010198,-204.318984254242,8.40164026751089));
#29801=CARTESIAN_POINT('Ctrl Pts',(7.27603390513785,-204.143984254242,4.20082013374671));
#29802=CARTESIAN_POINT('Ctrl Pts',(9.70137854017371,-203.968984254242,-1.74689612655491E-11));
#29803=CARTESIAN_POINT('Ctrl Pts',(7.27603390512272,-203.793984254242,-4.20082013377291));
#29804=CARTESIAN_POINT('Ctrl Pts',(4.85068927007173,-203.618984254242,-8.40164026752836));
#29805=CARTESIAN_POINT('Ctrl Pts',(-1.51301075899711E-11,-203.443984254242,
-8.40164026751963));
#29806=CARTESIAN_POINT('Ctrl Pts',(-4.85068927010198,-203.268984254242,
-8.40164026751089));
#29807=CARTESIAN_POINT('Ctrl Pts',(-7.27603390513785,-203.093984254242,
-4.20082013374671));
#29808=CARTESIAN_POINT('Ctrl Pts',(-9.70137854017371,-202.918984254242,
1.74701493417668E-11));
#29809=CARTESIAN_POINT('Ctrl Pts',(-7.27603390512272,-202.743984254242,
4.20082013377291));
#29810=CARTESIAN_POINT('Ctrl Pts',(-4.85068927007173,-202.568984254242,
8.40164026752836));
#29811=CARTESIAN_POINT('Ctrl Pts',(1.5129078685785E-11,-202.393984254242,
8.40164026751963));
#29812=CARTESIAN_POINT('Ctrl Pts',(4.85068927010198,-202.218984254242,8.40164026751089));
#29813=CARTESIAN_POINT('Ctrl Pts',(7.27603390513785,-202.043984254242,4.20082013374671));
#29814=CARTESIAN_POINT('Ctrl Pts',(9.70137854017371,-201.868984254242,-1.74689612655491E-11));
#29815=CARTESIAN_POINT('Ctrl Pts',(7.27603390512272,-201.693984254242,-4.20082013377291));
#29816=CARTESIAN_POINT('Ctrl Pts',(4.85068927007173,-201.518984254242,-8.40164026752836));
#29817=CARTESIAN_POINT('Ctrl Pts',(-1.51301075899711E-11,-201.343984254242,
-8.40164026751963));
#29818=CARTESIAN_POINT('Ctrl Pts',(-4.85068927010198,-201.168984254242,
-8.40164026751089));
#29819=CARTESIAN_POINT('Ctrl Pts',(-7.27603390513785,-200.993984254242,
-4.20082013374671));
#29820=CARTESIAN_POINT('Ctrl Pts',(-9.70137854017371,-200.818984254242,
1.74701493417668E-11));
#29821=CARTESIAN_POINT('Ctrl Pts',(-7.27603390512272,-200.643984254242,
4.20082013377291));
#29822=CARTESIAN_POINT('Ctrl Pts',(-4.85068927007173,-200.468984254242,
8.40164026752836));
#29823=CARTESIAN_POINT('Ctrl Pts',(1.5129078685785E-11,-200.293984254242,
8.40164026751963));
#29824=CARTESIAN_POINT('Ctrl Pts',(4.85068927010198,-200.118984254242,8.40164026751089));
#29825=CARTESIAN_POINT('Ctrl Pts',(7.27603390513785,-199.943984254242,4.20082013374671));
#29826=CARTESIAN_POINT('Ctrl Pts',(9.70137854017371,-199.768984254242,-1.74689612655491E-11));
#29827=CARTESIAN_POINT('Ctrl Pts',(7.27603390512272,-199.593984254242,-4.20082013377291));
#29828=CARTESIAN_POINT('Ctrl Pts',(4.85068927007173,-199.418984254242,-8.40164026752836));
#29829=CARTESIAN_POINT('Ctrl Pts',(-1.51301075899711E-11,-199.243984254242,
-8.40164026751963));
#29830=CARTESIAN_POINT('Ctrl Pts',(-4.85068927010198,-199.068984254242,
-8.40164026751089));
#29831=CARTESIAN_POINT('Ctrl Pts',(-7.27603390513785,-198.893984254242,
-4.20082013374671));
#29832=CARTESIAN_POINT('Ctrl Pts',(-9.70137854017371,-198.718984254242,
1.74701493417668E-11));
#29833=CARTESIAN_POINT('Ctrl Pts',(-7.27603390512272,-198.543984254242,
4.20082013377291));
#29834=CARTESIAN_POINT('Ctrl Pts',(-4.85068927007173,-198.368984254242,
8.40164026752836));
#29835=CARTESIAN_POINT('Ctrl Pts',(1.5129078685785E-11,-198.193984254242,
8.40164026751963));
#29836=CARTESIAN_POINT('Ctrl Pts',(4.85068927010198,-198.018984254242,8.40164026751089));
#29837=CARTESIAN_POINT('Ctrl Pts',(7.27603390513785,-197.843984254242,4.20082013374671));
#29838=CARTESIAN_POINT('Ctrl Pts',(9.70137854017371,-197.668984254242,-1.74689612655491E-11));
#29839=CARTESIAN_POINT('Ctrl Pts',(7.27603390512272,-197.493984254242,-4.20082013377291));
#29840=CARTESIAN_POINT('Ctrl Pts',(4.85068927007173,-197.318984254242,-8.40164026752836));
#29841=CARTESIAN_POINT('Ctrl Pts',(-1.51301075899711E-11,-197.143984254242,
-8.40164026751963));
#29842=CARTESIAN_POINT('Ctrl Pts',(-4.85068927010198,-196.968984254242,
-8.40164026751089));
#29843=CARTESIAN_POINT('Ctrl Pts',(-7.27603390513785,-196.793984254242,
-4.20082013374671));
#29844=CARTESIAN_POINT('Ctrl Pts',(-9.70137854017371,-196.618984254242,
1.74701493417668E-11));
#29845=CARTESIAN_POINT('Ctrl Pts',(-7.27603390512272,-196.443984254242,
4.20082013377291));
#29846=CARTESIAN_POINT('Ctrl Pts',(-4.85068927007173,-196.268984254242,
8.40164026752836));
#29847=CARTESIAN_POINT('Ctrl Pts',(1.5129078685785E-11,-196.093984254242,
8.40164026751963));
#29848=CARTESIAN_POINT('Ctrl Pts',(4.85068927010198,-195.918984254242,8.40164026751089));
#29849=CARTESIAN_POINT('Ctrl Pts',(7.27603390513785,-195.743984254242,4.20082013374671));
#29850=CARTESIAN_POINT('Ctrl Pts',(9.70137854017371,-195.568984254242,-1.74689612655491E-11));
#29851=CARTESIAN_POINT('Ctrl Pts',(7.27603390512272,-195.393984254242,-4.20082013377291));
#29852=CARTESIAN_POINT('Ctrl Pts',(4.85068927007173,-195.218984254242,-8.40164026752836));
#29853=CARTESIAN_POINT('Ctrl Pts',(-1.51301075899711E-11,-195.043984254242,
-8.40164026751963));
#29854=CARTESIAN_POINT('Ctrl Pts',(-4.85068927010198,-194.868984254242,
-8.40164026751089));
#29855=CARTESIAN_POINT('Ctrl Pts',(-7.27603390513785,-194.693984254242,
-4.20082013374671));
#29856=CARTESIAN_POINT('Ctrl Pts',(-9.70137854017371,-194.518984254242,
1.74701493417668E-11));
#29857=CARTESIAN_POINT('Ctrl Pts',(-7.27603390512272,-194.343984254242,
4.20082013377291));
#29858=CARTESIAN_POINT('Ctrl Pts',(-4.85068927007173,-194.168984254242,
8.40164026752836));
#29859=CARTESIAN_POINT('Ctrl Pts',(1.5129078685785E-11,-193.993984254242,
8.40164026751963));
#29860=CARTESIAN_POINT('Ctrl Pts',(4.85068927010198,-193.818984254242,8.40164026751089));
#29861=CARTESIAN_POINT('Ctrl Pts',(7.27603390513785,-193.643984254242,4.20082013374671));
#29862=CARTESIAN_POINT('Ctrl Pts',(9.70137854017371,-193.468984254242,-1.74689612655491E-11));
#29863=CARTESIAN_POINT('Ctrl Pts',(7.27603390512272,-193.293984254242,-4.20082013377291));
#29864=CARTESIAN_POINT('Ctrl Pts',(4.85068927007173,-193.118984254242,-8.40164026752836));
#29865=CARTESIAN_POINT('Ctrl Pts',(-1.51301075899711E-11,-192.943984254242,
-8.40164026751963));
#29866=CARTESIAN_POINT('Ctrl Pts',(-4.85068927010198,-192.768984254242,
-8.40164026751089));
#29867=CARTESIAN_POINT('Ctrl Pts',(-7.27603390513785,-192.593984254242,
-4.20082013374671));
#29868=CARTESIAN_POINT('Ctrl Pts',(-9.70137854017371,-192.418984254242,
1.74701493417668E-11));
#29869=CARTESIAN_POINT('Ctrl Pts',(-7.27603390512272,-192.243984254242,
4.20082013377291));
#29870=CARTESIAN_POINT('Ctrl Pts',(-4.85068927007173,-192.068984254242,
8.40164026752836));
#29871=CARTESIAN_POINT('Ctrl Pts',(1.5129078685785E-11,-191.893984254242,
8.40164026751963));
#29872=CARTESIAN_POINT('Ctrl Pts',(4.85068927010198,-191.718984254242,8.40164026751089));
#29873=CARTESIAN_POINT('Ctrl Pts',(7.27603390513785,-191.543984254242,4.20082013374671));
#29874=CARTESIAN_POINT('Ctrl Pts',(9.70137854017371,-191.368984254242,-1.74689612655491E-11));
#29875=CARTESIAN_POINT('Ctrl Pts',(7.27603390512272,-191.193984254242,-4.20082013377291));
#29876=CARTESIAN_POINT('Ctrl Pts',(4.85068927007173,-191.018984254242,-8.40164026752836));
#29877=CARTESIAN_POINT('Ctrl Pts',(-1.51301075899711E-11,-190.843984254242,
-8.40164026751963));
#29878=CARTESIAN_POINT('Ctrl Pts',(-4.85068927010198,-190.668984254242,
-8.40164026751089));
#29879=CARTESIAN_POINT('Ctrl Pts',(-7.27603390513785,-190.493984254242,
-4.20082013374671));
#29880=CARTESIAN_POINT('Ctrl Pts',(-9.70137854017371,-190.318984254242,
1.74701493417668E-11));
#29881=CARTESIAN_POINT('Ctrl Pts',(-7.27603390512272,-190.143984254242,
4.20082013377291));
#29882=CARTESIAN_POINT('Ctrl Pts',(-4.85068927007173,-189.968984254242,
8.40164026752836));
#29883=CARTESIAN_POINT('Ctrl Pts',(1.5129078685785E-11,-189.793984254242,
8.40164026751963));
#29884=CARTESIAN_POINT('Ctrl Pts',(4.85068927010198,-189.618984254242,8.40164026751089));
#29885=CARTESIAN_POINT('Ctrl Pts',(7.27603390513785,-189.443984254242,4.20082013374671));
#29886=CARTESIAN_POINT('Ctrl Pts',(9.70137854017371,-189.268984254242,-1.74689612655491E-11));
#29887=CARTESIAN_POINT('Ctrl Pts',(7.27603390512272,-189.093984254242,-4.20082013377291));
#29888=CARTESIAN_POINT('Ctrl Pts',(4.85068927007173,-188.918984254242,-8.40164026752836));
#29889=CARTESIAN_POINT('Ctrl Pts',(-1.51301075899711E-11,-188.743984254242,
-8.40164026751963));
#29890=CARTESIAN_POINT('Ctrl Pts',(-4.85068927010198,-188.568984254242,
-8.40164026751089));
#29891=CARTESIAN_POINT('Ctrl Pts',(-7.27603390513785,-188.393984254242,
-4.20082013374671));
#29892=CARTESIAN_POINT('Ctrl Pts',(-9.70137854017371,-188.218984254242,
1.74701493417668E-11));
#29893=CARTESIAN_POINT('Ctrl Pts',(-7.27603390512272,-188.043984254242,
4.20082013377291));
#29894=CARTESIAN_POINT('Ctrl Pts',(-4.85068927007173,-187.868984254242,
8.40164026752836));
#29895=CARTESIAN_POINT('Ctrl Pts',(1.5129078685785E-11,-187.693984254242,
8.40164026751963));
#29896=CARTESIAN_POINT('Ctrl Pts',(4.85068927010198,-187.518984254242,8.40164026751089));
#29897=CARTESIAN_POINT('Ctrl Pts',(7.27603390513785,-187.343984254242,4.20082013374671));
#29898=CARTESIAN_POINT('Ctrl Pts',(9.70137854017371,-187.168984254242,-1.74689612655491E-11));
#29899=CARTESIAN_POINT('Ctrl Pts',(7.27603390512272,-186.993984254242,-4.20082013377291));
#29900=CARTESIAN_POINT('Ctrl Pts',(4.85068927007173,-186.818984254242,-8.40164026752836));
#29901=CARTESIAN_POINT('Ctrl Pts',(-1.51301075899711E-11,-186.643984254242,
-8.40164026751963));
#29902=CARTESIAN_POINT('Ctrl Pts',(-4.85068927010198,-186.468984254242,
-8.40164026751089));
#29903=CARTESIAN_POINT('Ctrl Pts',(-7.27603390513785,-186.293984254242,
-4.20082013374671));
#29904=CARTESIAN_POINT('Ctrl Pts',(-9.70137854017371,-186.118984254242,
1.74701493417668E-11));
#29905=CARTESIAN_POINT('Ctrl Pts',(-7.27603390512272,-185.943984254242,
4.20082013377291));
#29906=CARTESIAN_POINT('Ctrl Pts',(-4.85068927007173,-185.768984254242,
8.40164026752836));
#29907=CARTESIAN_POINT('Ctrl Pts',(1.5129078685785E-11,-185.593984254242,
8.40164026751963));
#29908=CARTESIAN_POINT('Ctrl Pts',(4.85068927010198,-185.418984254242,8.40164026751089));
#29909=CARTESIAN_POINT('Ctrl Pts',(7.27603390513785,-185.243984254242,4.20082013374671));
#29910=CARTESIAN_POINT('Ctrl Pts',(9.70137854017371,-185.068984254242,-1.74689612655491E-11));
#29911=CARTESIAN_POINT('Ctrl Pts',(7.27603390512272,-184.893984254242,-4.20082013377291));
#29912=CARTESIAN_POINT('Ctrl Pts',(4.85068927007173,-184.718984254242,-8.40164026752836));
#29913=CARTESIAN_POINT('Ctrl Pts',(-1.51301075899711E-11,-184.543984254242,
-8.40164026751963));
#29914=CARTESIAN_POINT('Ctrl Pts',(-4.85068927010198,-184.368984254242,
-8.40164026751089));
#29915=CARTESIAN_POINT('Ctrl Pts',(-7.27603390513785,-184.193984254242,
-4.20082013374671));
#29916=CARTESIAN_POINT('Ctrl Pts',(-9.70137854017371,-184.018984254242,
1.74701493417668E-11));
#29917=CARTESIAN_POINT('Ctrl Pts',(-7.27603390512272,-183.843984254242,
4.20082013377291));
#29918=CARTESIAN_POINT('Ctrl Pts',(-4.85068927007173,-183.668984254242,
8.40164026752836));
#29919=CARTESIAN_POINT('Ctrl Pts',(1.5129078685785E-11,-183.493984254242,
8.40164026751963));
#29920=CARTESIAN_POINT('Ctrl Pts',(4.85068927010198,-183.318984254242,8.40164026751089));
#29921=CARTESIAN_POINT('Ctrl Pts',(7.27603390513785,-183.143984254242,4.20082013374671));
#29922=CARTESIAN_POINT('Ctrl Pts',(9.70137854017371,-182.968984254242,-1.74689612655491E-11));
#29923=CARTESIAN_POINT('Ctrl Pts',(7.27603390512272,-182.793984254242,-4.20082013377291));
#29924=CARTESIAN_POINT('Ctrl Pts',(4.85068927007173,-182.618984254242,-8.40164026752836));
#29925=CARTESIAN_POINT('Ctrl Pts',(-1.51301075899711E-11,-182.443984254242,
-8.40164026751963));
#29926=CARTESIAN_POINT('Ctrl Pts',(-4.85068927010198,-182.268984254242,
-8.40164026751089));
#29927=CARTESIAN_POINT('Ctrl Pts',(-7.27603390513785,-182.093984254242,
-4.20082013374671));
#29928=CARTESIAN_POINT('Ctrl Pts',(-9.70137854017371,-181.918984254242,
1.74701493417668E-11));
#29929=CARTESIAN_POINT('Ctrl Pts',(-7.27603390512272,-181.743984254242,
4.20082013377291));
#29930=CARTESIAN_POINT('Ctrl Pts',(-4.85068927007173,-181.568984254242,
8.40164026752836));
#29931=CARTESIAN_POINT('Ctrl Pts',(1.5129078685785E-11,-181.393984254242,
8.40164026751963));
#29932=CARTESIAN_POINT('Ctrl Pts',(4.85068927010198,-181.218984254242,8.40164026751089));
#29933=CARTESIAN_POINT('Ctrl Pts',(7.27603390513785,-181.043984254242,4.20082013374671));
#29934=CARTESIAN_POINT('Ctrl Pts',(9.70137854017371,-180.868984254242,-1.74689612655491E-11));
#29935=CARTESIAN_POINT('Ctrl Pts',(7.27603390512272,-180.693984254242,-4.20082013377291));
#29936=CARTESIAN_POINT('Ctrl Pts',(4.85068927007173,-180.518984254242,-8.40164026752836));
#29937=CARTESIAN_POINT('Ctrl Pts',(-1.51301075899711E-11,-180.343984254242,
-8.40164026751963));
#29938=CARTESIAN_POINT('Ctrl Pts',(-4.85068927010198,-180.168984254242,
-8.40164026751089));
#29939=CARTESIAN_POINT('Ctrl Pts',(-7.27603390513785,-179.993984254242,
-4.20082013374671));
#29940=CARTESIAN_POINT('Ctrl Pts',(-9.70137854017371,-179.818984254242,
1.74701493417668E-11));
#29941=CARTESIAN_POINT('Ctrl Pts',(-7.27603390512272,-179.643984254242,
4.20082013377291));
#29942=CARTESIAN_POINT('Ctrl Pts',(-4.85068927007173,-179.468984254242,
8.40164026752836));
#29943=CARTESIAN_POINT('Ctrl Pts',(1.5129078685785E-11,-179.293984254242,
8.40164026751963));
#29944=CARTESIAN_POINT('Ctrl Pts',(4.85068927010198,-179.118984254242,8.40164026751089));
#29945=CARTESIAN_POINT('Ctrl Pts',(7.27603390513785,-178.943984254242,4.20082013374671));
#29946=CARTESIAN_POINT('Ctrl Pts',(9.70137854017371,-178.768984254242,-1.74689612655491E-11));
#29947=CARTESIAN_POINT('Ctrl Pts',(7.27603390512272,-178.593984254242,-4.20082013377291));
#29948=CARTESIAN_POINT('Ctrl Pts',(4.85068927007173,-178.418984254242,-8.40164026752836));
#29949=CARTESIAN_POINT('Ctrl Pts',(-1.51301075899711E-11,-178.243984254242,
-8.40164026751963));
#29950=CARTESIAN_POINT('Ctrl Pts',(-4.85068927010198,-178.068984254242,
-8.40164026751089));
#29951=CARTESIAN_POINT('Ctrl Pts',(-7.27603390513785,-177.893984254242,
-4.20082013374671));
#29952=CARTESIAN_POINT('Ctrl Pts',(-9.70137854017371,-177.718984254242,
1.74701493417668E-11));
#29953=CARTESIAN_POINT('Ctrl Pts',(-7.27603390512272,-177.543984254242,
4.20082013377291));
#29954=CARTESIAN_POINT('Ctrl Pts',(-4.85068927007173,-177.368984254242,
8.40164026752836));
#29955=CARTESIAN_POINT('Ctrl Pts',(1.5129078685785E-11,-177.193984254242,
8.40164026751963));
#29956=CARTESIAN_POINT('Ctrl Pts',(4.85068927010198,-177.018984254242,8.40164026751089));
#29957=CARTESIAN_POINT('Ctrl Pts',(7.27603390513785,-176.843984254242,4.20082013374671));
#29958=CARTESIAN_POINT('Ctrl Pts',(9.70137854017371,-176.668984254242,-1.74689612655491E-11));
#29959=CARTESIAN_POINT('Ctrl Pts',(7.27603390512272,-176.493984254242,-4.20082013377291));
#29960=CARTESIAN_POINT('Ctrl Pts',(4.85068927007173,-176.318984254242,-8.40164026752836));
#29961=CARTESIAN_POINT('Ctrl Pts',(-1.51301075899711E-11,-176.143984254242,
-8.40164026751963));
#29962=CARTESIAN_POINT('Ctrl Pts',(-4.85068927010198,-175.968984254242,
-8.40164026751089));
#29963=CARTESIAN_POINT('Ctrl Pts',(-7.27603390513785,-175.793984254242,
-4.20082013374671));
#29964=CARTESIAN_POINT('Ctrl Pts',(-9.70137854017371,-175.618984254242,
1.74701493417668E-11));
#29965=CARTESIAN_POINT('Ctrl Pts',(-7.27603390512272,-175.443984254242,
4.20082013377291));
#29966=CARTESIAN_POINT('Ctrl Pts',(-4.85068927007173,-175.268984254242,
8.40164026752836));
#29967=CARTESIAN_POINT('Ctrl Pts',(1.5129078685785E-11,-175.093984254242,
8.40164026751963));
#29968=CARTESIAN_POINT('Ctrl Pts',(4.85068927010198,-174.918984254242,8.40164026751089));
#29969=CARTESIAN_POINT('Ctrl Pts',(7.27603390513785,-174.743984254242,4.20082013374671));
#29970=CARTESIAN_POINT('Ctrl Pts',(9.70137854017371,-174.568984254242,-1.74689612655491E-11));
#29971=CARTESIAN_POINT('Ctrl Pts',(7.27603390512272,-174.393984254242,-4.20082013377291));
#29972=CARTESIAN_POINT('Ctrl Pts',(4.85068927007173,-174.218984254242,-8.40164026752836));
#29973=CARTESIAN_POINT('Ctrl Pts',(-1.51301075899711E-11,-174.043984254242,
-8.40164026751963));
#29974=CARTESIAN_POINT('Ctrl Pts',(-4.85068927010198,-173.868984254242,
-8.40164026751089));
#29975=CARTESIAN_POINT('Ctrl Pts',(-7.27603390513785,-173.693984254242,
-4.20082013374671));
#29976=CARTESIAN_POINT('Ctrl Pts',(-9.70137854017371,-173.518984254242,
1.74701493417668E-11));
#29977=CARTESIAN_POINT('Ctrl Pts',(-7.27603390512272,-173.343984254242,
4.20082013377291));
#29978=CARTESIAN_POINT('Ctrl Pts',(-4.85068927007173,-173.168984254242,
8.40164026752836));
#29979=CARTESIAN_POINT('Ctrl Pts',(1.5129078685785E-11,-172.993984254242,
8.40164026751963));
#29980=CARTESIAN_POINT('Ctrl Pts',(4.85068927010198,-172.818984254242,8.40164026751089));
#29981=CARTESIAN_POINT('Ctrl Pts',(7.27603390513785,-172.643984254242,4.20082013374671));
#29982=CARTESIAN_POINT('Ctrl Pts',(9.70137854017371,-172.468984254242,-1.74689612655491E-11));
#29983=CARTESIAN_POINT('Ctrl Pts',(7.27603390512272,-172.293984254242,-4.20082013377291));
#29984=CARTESIAN_POINT('Ctrl Pts',(4.85068927007173,-172.118984254242,-8.40164026752836));
#29985=CARTESIAN_POINT('Ctrl Pts',(-1.51301075899711E-11,-171.943984254242,
-8.40164026751963));
#29986=CARTESIAN_POINT('Ctrl Pts',(-4.85068927010198,-171.768984254242,
-8.40164026751089));
#29987=CARTESIAN_POINT('Ctrl Pts',(-7.27603390513785,-171.593984254242,
-4.20082013374671));
#29988=CARTESIAN_POINT('Ctrl Pts',(-9.70137854017371,-171.418984254242,
1.74701493417668E-11));
#29989=CARTESIAN_POINT('Ctrl Pts',(-7.27603390512272,-171.243984254242,
4.20082013377291));
#29990=CARTESIAN_POINT('Ctrl Pts',(-4.85068927007173,-171.068984254242,
8.40164026752836));
#29991=CARTESIAN_POINT('Ctrl Pts',(1.5129078685785E-11,-170.893984254242,
8.40164026751963));
#29992=CARTESIAN_POINT('Ctrl Pts',(4.85068927010198,-170.718984254242,8.40164026751089));
#29993=CARTESIAN_POINT('Ctrl Pts',(7.27603390513785,-170.543984254242,4.20082013374671));
#29994=CARTESIAN_POINT('Ctrl Pts',(9.70137854017371,-170.368984254242,-1.74689612655491E-11));
#29995=CARTESIAN_POINT('Ctrl Pts',(7.27603390512272,-170.193984254242,-4.20082013377291));
#29996=CARTESIAN_POINT('Ctrl Pts',(4.85068927007173,-170.018984254242,-8.40164026752836));
#29997=CARTESIAN_POINT('Ctrl Pts',(-1.51301075899711E-11,-169.843984254242,
-8.40164026751963));
#29998=CARTESIAN_POINT('Ctrl Pts',(-4.85068927010198,-169.668984254242,
-8.40164026751089));
#29999=CARTESIAN_POINT('Ctrl Pts',(-7.27603390513785,-169.493984254242,
-4.20082013374671));
#30000=CARTESIAN_POINT('Ctrl Pts',(-9.70137854017371,-169.318984254242,
1.74701493417668E-11));
#30001=CARTESIAN_POINT('Ctrl Pts',(-7.27603390512272,-169.143984254242,
4.20082013377291));
#30002=CARTESIAN_POINT('Ctrl Pts',(-4.85068927007173,-168.968984254242,
8.40164026752836));
#30003=CARTESIAN_POINT('Ctrl Pts',(1.5129078685785E-11,-168.793984254242,
8.40164026751963));
#30004=CARTESIAN_POINT('Ctrl Pts',(4.85068927010198,-168.618984254242,8.40164026751089));
#30005=CARTESIAN_POINT('Ctrl Pts',(7.27603390513785,-168.443984254242,4.20082013374671));
#30006=CARTESIAN_POINT('Ctrl Pts',(9.70137854017371,-168.268984254242,-1.74689612655491E-11));
#30007=CARTESIAN_POINT('Ctrl Pts',(7.27603390512272,-168.093984254242,-4.20082013377291));
#30008=CARTESIAN_POINT('Ctrl Pts',(4.85068927007173,-167.918984254242,-8.40164026752836));
#30009=CARTESIAN_POINT('Ctrl Pts',(-1.51301075899711E-11,-167.743984254242,
-8.40164026751963));
#30010=CARTESIAN_POINT('Ctrl Pts',(-4.85068927010198,-167.568984254242,
-8.40164026751089));
#30011=CARTESIAN_POINT('Ctrl Pts',(-7.27603390513785,-167.393984254242,
-4.20082013374671));
#30012=CARTESIAN_POINT('Ctrl Pts',(-9.70137854017371,-167.218984254242,
1.74701493417668E-11));
#30013=CARTESIAN_POINT('Ctrl Pts',(-7.27603390512272,-167.043984254242,
4.20082013377291));
#30014=CARTESIAN_POINT('Ctrl Pts',(-4.85068927007173,-166.868984254242,
8.40164026752836));
#30015=CARTESIAN_POINT('Ctrl Pts',(1.5129078685785E-11,-166.693984254242,
8.40164026751963));
#30016=CARTESIAN_POINT('Ctrl Pts',(4.85068927010198,-166.518984254242,8.40164026751089));
#30017=CARTESIAN_POINT('Ctrl Pts',(7.27603390513785,-166.343984254242,4.20082013374671));
#30018=CARTESIAN_POINT('Ctrl Pts',(9.70137854017371,-166.168984254242,-1.74689612655491E-11));
#30019=CARTESIAN_POINT('Ctrl Pts',(7.27603390512272,-165.993984254242,-4.20082013377291));
#30020=CARTESIAN_POINT('Ctrl Pts',(4.85068927007173,-165.818984254242,-8.40164026752836));
#30021=CARTESIAN_POINT('Ctrl Pts',(-1.51301075899711E-11,-165.643984254242,
-8.40164026751963));
#30022=CARTESIAN_POINT('Ctrl Pts',(-4.85068927010198,-165.468984254242,
-8.40164026751089));
#30023=CARTESIAN_POINT('Ctrl Pts',(-7.27603390513785,-165.293984254242,
-4.20082013374671));
#30024=CARTESIAN_POINT('Ctrl Pts',(-9.70137854017371,-165.118984254242,
1.74701493417668E-11));
#30025=CARTESIAN_POINT('Ctrl Pts',(-7.27603390512272,-164.943984254242,
4.20082013377291));
#30026=CARTESIAN_POINT('Ctrl Pts',(-4.85068927007173,-164.768984254242,
8.40164026752836));
#30027=CARTESIAN_POINT('Ctrl Pts',(1.5129078685785E-11,-164.593984254242,
8.40164026751963));
#30028=CARTESIAN_POINT('Ctrl Pts',(4.85068927010198,-164.418984254242,8.40164026751089));
#30029=CARTESIAN_POINT('Ctrl Pts',(7.27603390513785,-164.243984254242,4.20082013374671));
#30030=CARTESIAN_POINT('Ctrl Pts',(9.70137854017371,-164.068984254242,-1.74689612655491E-11));
#30031=CARTESIAN_POINT('Ctrl Pts',(7.27603390512272,-163.893984254242,-4.20082013377291));
#30032=CARTESIAN_POINT('Ctrl Pts',(4.85068927007173,-163.718984254242,-8.40164026752836));
#30033=CARTESIAN_POINT('Ctrl Pts',(-1.51301075899711E-11,-163.543984254242,
-8.40164026751963));
#30034=CARTESIAN_POINT('Ctrl Pts',(-4.85068927010198,-163.368984254242,
-8.40164026751089));
#30035=CARTESIAN_POINT('Ctrl Pts',(-7.27603390513785,-163.193984254242,
-4.20082013374671));
#30036=CARTESIAN_POINT('Ctrl Pts',(-9.70137854017371,-163.018984254242,
1.74701493417668E-11));
#30037=CARTESIAN_POINT('Ctrl Pts',(-7.27603390512272,-162.843984254242,
4.20082013377291));
#30038=CARTESIAN_POINT('Ctrl Pts',(-4.85068927007173,-162.668984254242,
8.40164026752836));
#30039=CARTESIAN_POINT('Ctrl Pts',(1.5129078685785E-11,-162.493984254242,
8.40164026751963));
#30040=CARTESIAN_POINT('Ctrl Pts',(4.85068927010198,-162.318984254242,8.40164026751089));
#30041=CARTESIAN_POINT('Ctrl Pts',(7.27603390513785,-162.143984254242,4.20082013374671));
#30042=CARTESIAN_POINT('Ctrl Pts',(9.70137854017371,-161.968984254242,-1.74689612655491E-11));
#30043=CARTESIAN_POINT('Ctrl Pts',(7.27603390512272,-161.793984254242,-4.20082013377291));
#30044=CARTESIAN_POINT('Ctrl Pts',(4.85068927007173,-161.618984254242,-8.40164026752836));
#30045=CARTESIAN_POINT('Ctrl Pts',(-1.51301075899711E-11,-161.443984254242,
-8.40164026751963));
#30046=CARTESIAN_POINT('Ctrl Pts',(-4.85068927010198,-161.268984254242,
-8.40164026751089));
#30047=CARTESIAN_POINT('Ctrl Pts',(-7.27603390513785,-161.093984254242,
-4.20082013374671));
#30048=CARTESIAN_POINT('Ctrl Pts',(-9.70137854017371,-160.918984254242,
1.74701493417668E-11));
#30049=CARTESIAN_POINT('Ctrl Pts',(-7.27603390512272,-160.743984254242,
4.20082013377291));
#30050=CARTESIAN_POINT('Ctrl Pts',(-4.85068927007173,-160.568984254242,
8.40164026752836));
#30051=CARTESIAN_POINT('Ctrl Pts',(1.5129078685785E-11,-160.393984254242,
8.40164026751963));
#30052=CARTESIAN_POINT('Ctrl Pts',(4.85068927010198,-160.218984254242,8.40164026751089));
#30053=CARTESIAN_POINT('Ctrl Pts',(7.27603390513785,-160.043984254242,4.20082013374671));
#30054=CARTESIAN_POINT('Ctrl Pts',(9.70137854017371,-159.868984254242,-1.74689612655491E-11));
#30055=CARTESIAN_POINT('Ctrl Pts',(7.27603390512272,-159.693984254242,-4.20082013377291));
#30056=CARTESIAN_POINT('Ctrl Pts',(4.85068927007173,-159.518984254242,-8.40164026752836));
#30057=CARTESIAN_POINT('Ctrl Pts',(-1.51301075899711E-11,-159.343984254242,
-8.40164026751963));
#30058=CARTESIAN_POINT('Ctrl Pts',(-4.85068927010198,-159.168984254242,
-8.40164026751089));
#30059=CARTESIAN_POINT('Ctrl Pts',(-7.27603390513785,-158.993984254242,
-4.20082013374671));
#30060=CARTESIAN_POINT('Ctrl Pts',(-9.70137854017371,-158.818984254242,
1.74701493417668E-11));
#30061=CARTESIAN_POINT('Ctrl Pts',(-7.27603390512272,-158.643984254242,
4.20082013377291));
#30062=CARTESIAN_POINT('Ctrl Pts',(-4.85068927007173,-158.468984254242,
8.40164026752836));
#30063=CARTESIAN_POINT('Ctrl Pts',(1.5129078685785E-11,-158.293984254242,
8.40164026751963));
#30064=CARTESIAN_POINT('Ctrl Pts',(4.85068927010198,-158.118984254242,8.40164026751089));
#30065=CARTESIAN_POINT('Ctrl Pts',(7.27603390513785,-157.943984254242,4.20082013374671));
#30066=CARTESIAN_POINT('Ctrl Pts',(9.70137854017371,-157.768984254242,-1.74689612655491E-11));
#30067=CARTESIAN_POINT('Ctrl Pts',(7.27603390512272,-157.593984254242,-4.20082013377291));
#30068=CARTESIAN_POINT('Ctrl Pts',(4.85068927007173,-157.418984254242,-8.40164026752836));
#30069=CARTESIAN_POINT('Ctrl Pts',(-1.51301075899711E-11,-157.243984254242,
-8.40164026751963));
#30070=CARTESIAN_POINT('Ctrl Pts',(-4.85068927010198,-157.068984254242,
-8.40164026751089));
#30071=CARTESIAN_POINT('Ctrl Pts',(-7.27603390513785,-156.893984254242,
-4.20082013374671));
#30072=CARTESIAN_POINT('Ctrl Pts',(-9.70137854017371,-156.718984254242,
1.74701493417668E-11));
#30073=CARTESIAN_POINT('Ctrl Pts',(-7.27603390512272,-156.543984254242,
4.20082013377291));
#30074=CARTESIAN_POINT('Ctrl Pts',(-4.85068927007173,-156.368984254242,
8.40164026752836));
#30075=CARTESIAN_POINT('Ctrl Pts',(1.5129078685785E-11,-156.193984254242,
8.40164026751963));
#30076=CARTESIAN_POINT('Ctrl Pts',(4.85068927010198,-156.018984254242,8.40164026751089));
#30077=CARTESIAN_POINT('Ctrl Pts',(7.27603390513785,-155.843984254242,4.20082013374671));
#30078=CARTESIAN_POINT('Ctrl Pts',(9.70137854017371,-155.668984254242,-1.74689612655491E-11));
#30079=CARTESIAN_POINT('Ctrl Pts',(7.27603390512272,-155.493984254242,-4.20082013377291));
#30080=CARTESIAN_POINT('Ctrl Pts',(4.85068927007173,-155.318984254242,-8.40164026752836));
#30081=CARTESIAN_POINT('Ctrl Pts',(-1.51301075899711E-11,-155.143984254242,
-8.40164026751963));
#30082=CARTESIAN_POINT('Ctrl Pts',(-4.85068927010198,-154.968984254242,
-8.40164026751089));
#30083=CARTESIAN_POINT('Ctrl Pts',(-7.27603390513785,-154.793984254242,
-4.20082013374671));
#30084=CARTESIAN_POINT('Ctrl Pts',(-9.70137854017371,-154.618984254242,
1.74701493417668E-11));
#30085=CARTESIAN_POINT('Ctrl Pts',(-7.27603390512272,-154.443984254242,
4.20082013377291));
#30086=CARTESIAN_POINT('Ctrl Pts',(-4.85068927007173,-154.268984254242,
8.40164026752836));
#30087=CARTESIAN_POINT('Ctrl Pts',(1.5129078685785E-11,-154.093984254242,
8.40164026751963));
#30088=CARTESIAN_POINT('Ctrl Pts',(4.85068927010198,-153.918984254242,8.40164026751089));
#30089=CARTESIAN_POINT('Ctrl Pts',(7.27603390513785,-153.743984254242,4.20082013374671));
#30090=CARTESIAN_POINT('Ctrl Pts',(9.70137854017371,-153.568984254242,-1.74689612655491E-11));
#30091=CARTESIAN_POINT('Ctrl Pts',(7.27603390512272,-153.393984254242,-4.20082013377291));
#30092=CARTESIAN_POINT('Ctrl Pts',(4.85068927007173,-153.218984254242,-8.40164026752836));
#30093=CARTESIAN_POINT('Ctrl Pts',(-1.51301075899711E-11,-153.043984254242,
-8.40164026751963));
#30094=CARTESIAN_POINT('Ctrl Pts',(-4.85068927010198,-152.868984254242,
-8.40164026751089));
#30095=CARTESIAN_POINT('Ctrl Pts',(-7.27603390513785,-152.693984254242,
-4.20082013374671));
#30096=CARTESIAN_POINT('Ctrl Pts',(-9.70137854017371,-152.518984254242,
1.74701493417668E-11));
#30097=CARTESIAN_POINT('Ctrl Pts',(-7.27603390512272,-152.343984254242,
4.20082013377291));
#30098=CARTESIAN_POINT('Ctrl Pts',(-4.85068927007173,-152.168984254242,
8.40164026752836));
#30099=CARTESIAN_POINT('Ctrl Pts',(1.5129078685785E-11,-151.993984254242,
8.40164026751963));
#30100=CARTESIAN_POINT('Ctrl Pts',(4.85068927010198,-151.818984254242,8.40164026751089));
#30101=CARTESIAN_POINT('Ctrl Pts',(7.27603390513785,-151.643984254242,4.20082013374671));
#30102=CARTESIAN_POINT('Ctrl Pts',(9.70137854017371,-151.468984254242,-1.74689612655491E-11));
#30103=CARTESIAN_POINT('Ctrl Pts',(7.27603390512272,-151.293984254242,-4.20082013377291));
#30104=CARTESIAN_POINT('Ctrl Pts',(4.85068927007173,-151.118984254242,-8.40164026752836));
#30105=CARTESIAN_POINT('Ctrl Pts',(-1.51301075899711E-11,-150.943984254242,
-8.40164026751963));
#30106=CARTESIAN_POINT('Ctrl Pts',(-4.85068927010198,-150.768984254242,
-8.40164026751089));
#30107=CARTESIAN_POINT('Ctrl Pts',(-7.27603390513785,-150.593984254242,
-4.20082013374671));
#30108=CARTESIAN_POINT('Ctrl Pts',(-9.70137854017371,-150.418984254242,
1.74701493417668E-11));
#30109=CARTESIAN_POINT('Ctrl Pts',(-7.27603390512272,-150.243984254242,
4.20082013377291));
#30110=CARTESIAN_POINT('Ctrl Pts',(-4.85068927007173,-150.068984254242,
8.40164026752836));
#30111=CARTESIAN_POINT('Ctrl Pts',(1.5129078685785E-11,-149.893984254242,
8.40164026751963));
#30112=CARTESIAN_POINT('Ctrl Pts',(4.85068927010198,-149.718984254242,8.40164026751089));
#30113=CARTESIAN_POINT('Ctrl Pts',(7.27603390513785,-149.543984254242,4.20082013374671));
#30114=CARTESIAN_POINT('Ctrl Pts',(9.70137854017371,-149.368984254242,-1.74689612655491E-11));
#30115=CARTESIAN_POINT('Ctrl Pts',(7.27603390512272,-149.193984254242,-4.20082013377291));
#30116=CARTESIAN_POINT('Ctrl Pts',(4.85068927007173,-149.018984254242,-8.40164026752836));
#30117=CARTESIAN_POINT('Ctrl Pts',(-1.51301075899711E-11,-148.843984254242,
-8.40164026751963));
#30118=CARTESIAN_POINT('Ctrl Pts',(-4.85068927010198,-148.668984254242,
-8.40164026751089));
#30119=CARTESIAN_POINT('Ctrl Pts',(-7.27603390513785,-148.493984254242,
-4.20082013374671));
#30120=CARTESIAN_POINT('Ctrl Pts',(-9.70137854017371,-148.318984254242,
1.74701493417668E-11));
#30121=CARTESIAN_POINT('Ctrl Pts',(-7.27603390512272,-148.143984254242,
4.20082013377291));
#30122=CARTESIAN_POINT('Ctrl Pts',(-4.85068927007173,-147.968984254242,
8.40164026752836));
#30123=CARTESIAN_POINT('Ctrl Pts',(1.5129078685785E-11,-147.793984254242,
8.40164026751963));
#30124=CARTESIAN_POINT('Ctrl Pts',(4.85068927010198,-147.618984254242,8.40164026751089));
#30125=CARTESIAN_POINT('Ctrl Pts',(7.27603390513785,-147.443984254242,4.20082013374671));
#30126=CARTESIAN_POINT('Ctrl Pts',(9.70137854017371,-147.268984254242,-1.74689612655491E-11));
#30127=CARTESIAN_POINT('Ctrl Pts',(7.27603390512272,-147.093984254242,-4.20082013377291));
#30128=CARTESIAN_POINT('Ctrl Pts',(4.85068927007173,-146.918984254242,-8.40164026752836));
#30129=CARTESIAN_POINT('Ctrl Pts',(-1.51301075899711E-11,-146.743984254242,
-8.40164026751963));
#30130=CARTESIAN_POINT('Ctrl Pts',(-4.85068927010198,-146.568984254242,
-8.40164026751089));
#30131=CARTESIAN_POINT('Ctrl Pts',(-7.27603390513785,-146.393984254242,
-4.20082013374671));
#30132=CARTESIAN_POINT('Ctrl Pts',(-9.70137854017371,-146.218984254242,
1.74701493417668E-11));
#30133=CARTESIAN_POINT('Ctrl Pts',(-7.27603390512272,-146.043984254242,
4.20082013377291));
#30134=CARTESIAN_POINT('Ctrl Pts',(-4.85068927007173,-145.868984254242,
8.40164026752836));
#30135=CARTESIAN_POINT('Ctrl Pts',(1.5129078685785E-11,-145.693984254242,
8.40164026751963));
#30136=CARTESIAN_POINT('Ctrl Pts',(4.85068927010198,-145.518984254242,8.40164026751089));
#30137=CARTESIAN_POINT('Ctrl Pts',(7.27603390513785,-145.343984254242,4.20082013374671));
#30138=CARTESIAN_POINT('Ctrl Pts',(9.70137854017371,-145.168984254242,-1.74689612655491E-11));
#30139=CARTESIAN_POINT('Ctrl Pts',(7.27603390512272,-144.993984254242,-4.20082013377291));
#30140=CARTESIAN_POINT('Ctrl Pts',(4.85068927007173,-144.818984254242,-8.40164026752836));
#30141=CARTESIAN_POINT('Ctrl Pts',(-1.51301075899711E-11,-144.643984254242,
-8.40164026751963));
#30142=CARTESIAN_POINT('Ctrl Pts',(-4.85068927010198,-144.468984254242,
-8.40164026751089));
#30143=CARTESIAN_POINT('Ctrl Pts',(-7.27603390513785,-144.293984254242,
-4.20082013374671));
#30144=CARTESIAN_POINT('Ctrl Pts',(-9.70137854017371,-144.118984254242,
1.74701493417668E-11));
#30145=CARTESIAN_POINT('Ctrl Pts',(-7.27603390512272,-143.943984254242,
4.20082013377291));
#30146=CARTESIAN_POINT('Ctrl Pts',(-4.85068927007173,-143.768984254242,
8.40164026752836));
#30147=CARTESIAN_POINT('Ctrl Pts',(1.5129078685785E-11,-143.593984254242,
8.40164026751963));
#30148=CARTESIAN_POINT('Ctrl Pts',(4.85068927010198,-143.418984254242,8.40164026751089));
#30149=CARTESIAN_POINT('Ctrl Pts',(7.27603390513785,-143.243984254242,4.20082013374671));
#30150=CARTESIAN_POINT('Ctrl Pts',(9.70137854017371,-143.068984254242,-1.74689612655491E-11));
#30151=CARTESIAN_POINT('Ctrl Pts',(7.27603390512272,-142.893984254242,-4.20082013377291));
#30152=CARTESIAN_POINT('Ctrl Pts',(4.85068927007173,-142.718984254242,-8.40164026752836));
#30153=CARTESIAN_POINT('Ctrl Pts',(-1.51301075899711E-11,-142.543984254242,
-8.40164026751963));
#30154=CARTESIAN_POINT('Ctrl Pts',(-4.85068927010198,-142.368984254242,
-8.40164026751089));
#30155=CARTESIAN_POINT('Ctrl Pts',(-7.27603390513785,-142.193984254242,
-4.20082013374671));
#30156=CARTESIAN_POINT('Ctrl Pts',(-9.70137854017371,-142.018984254242,
1.74701493417668E-11));
#30157=CARTESIAN_POINT('Ctrl Pts',(-7.27603390512272,-141.843984254242,
4.20082013377291));
#30158=CARTESIAN_POINT('Ctrl Pts',(-4.85068927007173,-141.668984254242,
8.40164026752836));
#30159=CARTESIAN_POINT('Ctrl Pts',(1.5129078685785E-11,-141.493984254242,
8.40164026751963));
#30160=CARTESIAN_POINT('Ctrl Pts',(4.85068927010198,-141.318984254242,8.40164026751089));
#30161=CARTESIAN_POINT('Ctrl Pts',(7.27603390513785,-141.143984254242,4.20082013374671));
#30162=CARTESIAN_POINT('Ctrl Pts',(9.70137854017371,-140.968984254242,-1.74689612655491E-11));
#30163=CARTESIAN_POINT('Ctrl Pts',(7.27603390512272,-140.793984254242,-4.20082013377291));
#30164=CARTESIAN_POINT('Ctrl Pts',(4.85068927007173,-140.618984254242,-8.40164026752836));
#30165=CARTESIAN_POINT('Ctrl Pts',(-1.51301075899711E-11,-140.443984254242,
-8.40164026751963));
#30166=CARTESIAN_POINT('Ctrl Pts',(-4.85068927010198,-140.268984254242,
-8.40164026751089));
#30167=CARTESIAN_POINT('Ctrl Pts',(-7.27603390513785,-140.093984254242,
-4.20082013374671));
#30168=CARTESIAN_POINT('Ctrl Pts',(-9.70137854017371,-139.918984254242,
1.74701493417668E-11));
#30169=CARTESIAN_POINT('Ctrl Pts',(-7.27603390512272,-139.743984254242,
4.20082013377291));
#30170=CARTESIAN_POINT('Ctrl Pts',(-4.85068927007173,-139.568984254242,
8.40164026752836));
#30171=CARTESIAN_POINT('Ctrl Pts',(1.5129078685785E-11,-139.393984254242,
8.40164026751963));
#30172=CARTESIAN_POINT('Ctrl Pts',(4.85068927010198,-139.218984254242,8.40164026751089));
#30173=CARTESIAN_POINT('Ctrl Pts',(7.27603390513785,-139.043984254242,4.20082013374671));
#30174=CARTESIAN_POINT('Ctrl Pts',(9.70137854017371,-138.868984254242,-1.74689612655491E-11));
#30175=CARTESIAN_POINT('Ctrl Pts',(7.27603390512272,-138.693984254242,-4.20082013377291));
#30176=CARTESIAN_POINT('Ctrl Pts',(4.85068927007173,-138.518984254242,-8.40164026752836));
#30177=CARTESIAN_POINT('Ctrl Pts',(-1.51301075899711E-11,-138.343984254242,
-8.40164026751963));
#30178=CARTESIAN_POINT('Ctrl Pts',(-4.85068927010198,-138.168984254242,
-8.40164026751089));
#30179=CARTESIAN_POINT('Ctrl Pts',(-7.27603390513785,-137.993984254242,
-4.20082013374671));
#30180=CARTESIAN_POINT('Ctrl Pts',(-9.70137854017371,-137.818984254242,
1.74701493417668E-11));
#30181=CARTESIAN_POINT('Ctrl Pts',(-7.27603390512272,-137.643984254242,
4.20082013377291));
#30182=CARTESIAN_POINT('Ctrl Pts',(-4.85068927007173,-137.468984254242,
8.40164026752836));
#30183=CARTESIAN_POINT('Ctrl Pts',(1.5129078685785E-11,-137.293984254242,
8.40164026751963));
#30184=CARTESIAN_POINT('Ctrl Pts',(4.85068927010198,-137.118984254242,8.40164026751089));
#30185=CARTESIAN_POINT('Ctrl Pts',(7.27603390513785,-136.943984254242,4.20082013374671));
#30186=CARTESIAN_POINT('Ctrl Pts',(9.70137854017371,-136.768984254242,-1.74689612655491E-11));
#30187=CARTESIAN_POINT('Ctrl Pts',(7.27603390512272,-136.593984254242,-4.20082013377291));
#30188=CARTESIAN_POINT('Ctrl Pts',(4.85068927007173,-136.418984254242,-8.40164026752836));
#30189=CARTESIAN_POINT('Ctrl Pts',(-1.51301075899711E-11,-136.243984254242,
-8.40164026751963));
#30190=CARTESIAN_POINT('Ctrl Pts',(-4.85068927010198,-136.068984254242,
-8.40164026751089));
#30191=CARTESIAN_POINT('Ctrl Pts',(-7.27603390513785,-135.893984254242,
-4.20082013374671));
#30192=CARTESIAN_POINT('Ctrl Pts',(-9.70137854017371,-135.718984254242,
1.74701493417668E-11));
#30193=CARTESIAN_POINT('Ctrl Pts',(-7.27603390512272,-135.543984254242,
4.20082013377291));
#30194=CARTESIAN_POINT('Ctrl Pts',(-4.85068927007173,-135.368984254242,
8.40164026752836));
#30195=CARTESIAN_POINT('Ctrl Pts',(1.5129078685785E-11,-135.193984254242,
8.40164026751963));
#30196=CARTESIAN_POINT('Ctrl Pts',(4.85068927010198,-135.018984254242,8.40164026751089));
#30197=CARTESIAN_POINT('Ctrl Pts',(7.27603390513785,-134.843984254242,4.20082013374671));
#30198=CARTESIAN_POINT('Ctrl Pts',(9.70137854017371,-134.668984254242,-1.74689612655491E-11));
#30199=CARTESIAN_POINT('Ctrl Pts',(7.27603390512272,-134.493984254242,-4.20082013377291));
#30200=CARTESIAN_POINT('Ctrl Pts',(4.85068927007173,-134.318984254242,-8.40164026752836));
#30201=CARTESIAN_POINT('Ctrl Pts',(-1.51301075899711E-11,-134.143984254242,
-8.40164026751963));
#30202=CARTESIAN_POINT('Ctrl Pts',(-4.85068927010198,-133.968984254242,
-8.40164026751089));
#30203=CARTESIAN_POINT('Ctrl Pts',(-7.27603390513785,-133.793984254242,
-4.20082013374671));
#30204=CARTESIAN_POINT('Ctrl Pts',(-9.70137854017371,-133.618984254242,
1.74701493417668E-11));
#30205=CARTESIAN_POINT('Ctrl Pts',(-7.27603390512272,-133.443984254242,
4.20082013377291));
#30206=CARTESIAN_POINT('Ctrl Pts',(-4.85068927007173,-133.268984254242,
8.40164026752836));
#30207=CARTESIAN_POINT('Ctrl Pts',(1.5129078685785E-11,-133.093984254242,
8.40164026751963));
#30208=CARTESIAN_POINT('Ctrl Pts',(4.85068927010198,-132.918984254242,8.40164026751089));
#30209=CARTESIAN_POINT('Ctrl Pts',(7.27603390513785,-132.743984254242,4.20082013374671));
#30210=CARTESIAN_POINT('Ctrl Pts',(9.70137854017371,-132.568984254242,-1.74689612655491E-11));
#30211=CARTESIAN_POINT('Ctrl Pts',(7.27603390512272,-132.393984254242,-4.20082013377291));
#30212=CARTESIAN_POINT('Ctrl Pts',(4.85068927007173,-132.218984254242,-8.40164026752836));
#30213=CARTESIAN_POINT('Ctrl Pts',(-1.51301075899711E-11,-132.043984254242,
-8.40164026751963));
#30214=CARTESIAN_POINT('Ctrl Pts',(-4.85068927010198,-131.868984254242,
-8.40164026751089));
#30215=CARTESIAN_POINT('Ctrl Pts',(-7.27603390513785,-131.693984254242,
-4.20082013374671));
#30216=CARTESIAN_POINT('Ctrl Pts',(-9.70137854017371,-131.518984254242,
1.74701493417668E-11));
#30217=CARTESIAN_POINT('Ctrl Pts',(-7.27603390512272,-131.343984254242,
4.20082013377291));
#30218=CARTESIAN_POINT('Ctrl Pts',(-4.85068927007173,-131.168984254242,
8.40164026752836));
#30219=CARTESIAN_POINT('Ctrl Pts',(1.5129078685785E-11,-130.993984254242,
8.40164026751963));
#30220=CARTESIAN_POINT('Ctrl Pts',(4.85068927010198,-130.818984254242,8.40164026751089));
#30221=CARTESIAN_POINT('Ctrl Pts',(7.27603390513785,-130.643984254242,4.20082013374671));
#30222=CARTESIAN_POINT('Ctrl Pts',(9.70137854017371,-130.468984254242,-1.74689612655491E-11));
#30223=CARTESIAN_POINT('Ctrl Pts',(7.27603390512272,-130.293984254242,-4.20082013377291));
#30224=CARTESIAN_POINT('Ctrl Pts',(4.85068927007173,-130.118984254242,-8.40164026752836));
#30225=CARTESIAN_POINT('Ctrl Pts',(-1.51301075899711E-11,-129.943984254242,
-8.40164026751963));
#30226=CARTESIAN_POINT('Ctrl Pts',(-4.85068927010198,-129.768984254242,
-8.40164026751089));
#30227=CARTESIAN_POINT('Ctrl Pts',(-7.27603390513785,-129.593984254242,
-4.20082013374671));
#30228=CARTESIAN_POINT('Ctrl Pts',(-9.70137854017371,-129.418984254242,
1.74701493417668E-11));
#30229=CARTESIAN_POINT('Ctrl Pts',(-7.27603390512272,-129.243984254242,
4.20082013377291));
#30230=CARTESIAN_POINT('Ctrl Pts',(-4.85068927007173,-129.068984254242,
8.40164026752836));
#30231=CARTESIAN_POINT('Ctrl Pts',(1.5129078685785E-11,-128.893984254242,
8.40164026751963));
#30232=CARTESIAN_POINT('Ctrl Pts',(4.85068927010198,-128.718984254242,8.40164026751089));
#30233=CARTESIAN_POINT('Ctrl Pts',(7.27603390513785,-128.543984254242,4.20082013374671));
#30234=CARTESIAN_POINT('Ctrl Pts',(9.70137854017371,-128.368984254242,-1.74689612655491E-11));
#30235=CARTESIAN_POINT('Ctrl Pts',(7.27603390512272,-128.193984254242,-4.20082013377291));
#30236=CARTESIAN_POINT('Ctrl Pts',(4.85068927007173,-128.018984254242,-8.40164026752836));
#30237=CARTESIAN_POINT('Ctrl Pts',(-1.51301075899711E-11,-127.843984254242,
-8.40164026751963));
#30238=CARTESIAN_POINT('Ctrl Pts',(-4.85068927010198,-127.668984254242,
-8.40164026751089));
#30239=CARTESIAN_POINT('Ctrl Pts',(-7.27603390513785,-127.493984254242,
-4.20082013374671));
#30240=CARTESIAN_POINT('Ctrl Pts',(-9.70137854017371,-127.318984254242,
1.74701493417668E-11));
#30241=CARTESIAN_POINT('Ctrl Pts',(-7.27603390512272,-127.143984254242,
4.20082013377291));
#30242=CARTESIAN_POINT('Ctrl Pts',(-4.85068927007173,-126.968984254242,
8.40164026752836));
#30243=CARTESIAN_POINT('Ctrl Pts',(1.5129078685785E-11,-126.793984254242,
8.40164026751963));
#30244=CARTESIAN_POINT('Ctrl Pts',(4.85068927010198,-126.618984254242,8.40164026751089));
#30245=CARTESIAN_POINT('Ctrl Pts',(7.27603390513785,-126.443984254242,4.20082013374671));
#30246=CARTESIAN_POINT('Ctrl Pts',(9.70137854017371,-126.268984254242,-1.74689612655491E-11));
#30247=CARTESIAN_POINT('Ctrl Pts',(7.27603390512272,-126.093984254242,-4.20082013377291));
#30248=CARTESIAN_POINT('Ctrl Pts',(4.85068927007173,-125.918984254242,-8.40164026752836));
#30249=CARTESIAN_POINT('Ctrl Pts',(-1.51301075899711E-11,-125.743984254242,
-8.40164026751963));
#30250=CARTESIAN_POINT('Ctrl Pts',(-4.85068927010198,-125.568984254242,
-8.40164026751089));
#30251=CARTESIAN_POINT('Ctrl Pts',(-7.27603390513785,-125.393984254242,
-4.20082013374671));
#30252=CARTESIAN_POINT('Ctrl Pts',(-9.70137854017371,-125.218984254242,
1.74701493417668E-11));
#30253=CARTESIAN_POINT('Ctrl Pts',(-7.27603390512272,-125.043984254242,
4.20082013377291));
#30254=CARTESIAN_POINT('Ctrl Pts',(-4.85068927007173,-124.868984254242,
8.40164026752836));
#30255=CARTESIAN_POINT('Ctrl Pts',(1.5129078685785E-11,-124.693984254242,
8.40164026751963));
#30256=CARTESIAN_POINT('Ctrl Pts',(4.85068927010198,-124.518984254242,8.40164026751089));
#30257=CARTESIAN_POINT('Ctrl Pts',(7.27603390513785,-124.343984254242,4.20082013374671));
#30258=CARTESIAN_POINT('Ctrl Pts',(9.70137854017371,-124.168984254242,-1.74689612655491E-11));
#30259=CARTESIAN_POINT('Ctrl Pts',(7.27603390512272,-123.993984254242,-4.20082013377291));
#30260=CARTESIAN_POINT('Ctrl Pts',(4.85068927007173,-123.818984254242,-8.40164026752836));
#30261=CARTESIAN_POINT('Ctrl Pts',(-1.51301075899711E-11,-123.643984254242,
-8.40164026751963));
#30262=CARTESIAN_POINT('Ctrl Pts',(-4.85068927010198,-123.468984254242,
-8.40164026751089));
#30263=CARTESIAN_POINT('Ctrl Pts',(-7.27603390513785,-123.293984254242,
-4.20082013374671));
#30264=CARTESIAN_POINT('Ctrl Pts',(-9.70137854017371,-123.118984254242,
1.74701493417668E-11));
#30265=CARTESIAN_POINT('Ctrl Pts',(-7.27603390512272,-122.943984254242,
4.20082013377291));
#30266=CARTESIAN_POINT('Ctrl Pts',(-4.85068927007173,-122.768984254242,
8.40164026752836));
#30267=CARTESIAN_POINT('Ctrl Pts',(1.5129078685785E-11,-122.593984254242,
8.40164026751963));
#30268=CARTESIAN_POINT('Ctrl Pts',(4.85068927010198,-122.418984254242,8.40164026751089));
#30269=CARTESIAN_POINT('Ctrl Pts',(7.27603390513785,-122.243984254242,4.20082013374671));
#30270=CARTESIAN_POINT('Ctrl Pts',(9.70137854017371,-122.068984254242,-1.74689612655491E-11));
#30271=CARTESIAN_POINT('Ctrl Pts',(7.27603390512272,-121.893984254242,-4.20082013377291));
#30272=CARTESIAN_POINT('Ctrl Pts',(4.85068927007173,-121.718984254242,-8.40164026752836));
#30273=CARTESIAN_POINT('Ctrl Pts',(-1.51301075899711E-11,-121.543984254242,
-8.40164026751963));
#30274=CARTESIAN_POINT('Ctrl Pts',(-4.85068927010198,-121.368984254242,
-8.40164026751089));
#30275=CARTESIAN_POINT('Ctrl Pts',(-7.27603390513785,-121.193984254242,
-4.20082013374671));
#30276=CARTESIAN_POINT('Ctrl Pts',(-9.70137854017371,-121.018984254242,
1.74701493417668E-11));
#30277=CARTESIAN_POINT('Ctrl Pts',(-7.27603390512272,-120.843984254242,
4.20082013377291));
#30278=CARTESIAN_POINT('Ctrl Pts',(-4.85068927007173,-120.668984254242,
8.40164026752836));
#30279=CARTESIAN_POINT('Ctrl Pts',(1.5129078685785E-11,-120.493984254242,
8.40164026751963));
#30280=CARTESIAN_POINT('Ctrl Pts',(4.85068927010198,-120.318984254242,8.40164026751089));
#30281=CARTESIAN_POINT('Ctrl Pts',(7.27603390513785,-120.143984254242,4.20082013374671));
#30282=CARTESIAN_POINT('Ctrl Pts',(9.70137854017371,-119.968984254242,-1.74689612655491E-11));
#30283=CARTESIAN_POINT('Ctrl Pts',(7.27603390512272,-119.793984254242,-4.20082013377291));
#30284=CARTESIAN_POINT('Ctrl Pts',(4.85068927007173,-119.618984254242,-8.40164026752836));
#30285=CARTESIAN_POINT('Ctrl Pts',(-1.51301075899711E-11,-119.443984254242,
-8.40164026751963));
#30286=CARTESIAN_POINT('Ctrl Pts',(-4.85068927010198,-119.268984254242,
-8.40164026751089));
#30287=CARTESIAN_POINT('Ctrl Pts',(-7.27603390513785,-119.093984254242,
-4.20082013374671));
#30288=CARTESIAN_POINT('Ctrl Pts',(-9.70137854017371,-118.918984254242,
1.74701493417668E-11));
#30289=CARTESIAN_POINT('Ctrl Pts',(-7.27603390512272,-118.743984254242,
4.20082013377291));
#30290=CARTESIAN_POINT('Ctrl Pts',(-4.85068927007173,-118.568984254242,
8.40164026752836));
#30291=CARTESIAN_POINT('Ctrl Pts',(1.5129078685785E-11,-118.393984254242,
8.40164026751963));
#30292=CARTESIAN_POINT('Ctrl Pts',(4.85068927010198,-118.218984254242,8.40164026751089));
#30293=CARTESIAN_POINT('Ctrl Pts',(7.27603390513785,-118.043984254242,4.20082013374671));
#30294=CARTESIAN_POINT('Ctrl Pts',(9.70137854017371,-117.868984254242,-1.74689612655491E-11));
#30295=CARTESIAN_POINT('Ctrl Pts',(7.27603390512272,-117.693984254242,-4.20082013377291));
#30296=CARTESIAN_POINT('Ctrl Pts',(4.85068927007173,-117.518984254242,-8.40164026752836));
#30297=CARTESIAN_POINT('Ctrl Pts',(-1.51301075899711E-11,-117.343984254242,
-8.40164026751963));
#30298=CARTESIAN_POINT('Ctrl Pts',(-4.85068927010198,-117.168984254242,
-8.40164026751089));
#30299=CARTESIAN_POINT('Ctrl Pts',(-7.27603390513785,-116.993984254242,
-4.20082013374671));
#30300=CARTESIAN_POINT('Ctrl Pts',(-9.70137854017371,-116.818984254242,
1.74701493417668E-11));
#30301=CARTESIAN_POINT('Ctrl Pts',(-7.27603390512272,-116.643984254242,
4.20082013377291));
#30302=CARTESIAN_POINT('Ctrl Pts',(-4.85068927007173,-116.468984254242,
8.40164026752836));
#30303=CARTESIAN_POINT('Ctrl Pts',(1.5129078685785E-11,-116.293984254242,
8.40164026751963));
#30304=CARTESIAN_POINT('Ctrl Pts',(4.85068927010198,-116.118984254242,8.40164026751089));
#30305=CARTESIAN_POINT('Ctrl Pts',(7.27603390513785,-115.943984254242,4.20082013374671));
#30306=CARTESIAN_POINT('Ctrl Pts',(9.70137854017371,-115.768984254242,-1.74689612655491E-11));
#30307=CARTESIAN_POINT('Ctrl Pts',(7.27603390512272,-115.593984254242,-4.20082013377291));
#30308=CARTESIAN_POINT('Ctrl Pts',(4.85068927007173,-115.418984254242,-8.40164026752836));
#30309=CARTESIAN_POINT('Ctrl Pts',(-1.51301075899711E-11,-115.243984254242,
-8.40164026751963));
#30310=CARTESIAN_POINT('Ctrl Pts',(-4.85068927010198,-115.068984254242,
-8.40164026751089));
#30311=CARTESIAN_POINT('Ctrl Pts',(-7.27603390513785,-114.893984254242,
-4.20082013374671));
#30312=CARTESIAN_POINT('Ctrl Pts',(-9.70137854017371,-114.718984254242,
1.74701493417668E-11));
#30313=CARTESIAN_POINT('Ctrl Pts',(-7.27603390512272,-114.543984254242,
4.20082013377291));
#30314=CARTESIAN_POINT('Ctrl Pts',(-4.85068927007173,-114.368984254242,
8.40164026752836));
#30315=CARTESIAN_POINT('Ctrl Pts',(1.5129078685785E-11,-114.193984254242,
8.40164026751963));
#30316=CARTESIAN_POINT('Ctrl Pts',(4.85068927010198,-114.018984254242,8.40164026751089));
#30317=CARTESIAN_POINT('Ctrl Pts',(7.27603390513785,-113.843984254242,4.20082013374671));
#30318=CARTESIAN_POINT('Ctrl Pts',(9.70137854017371,-113.668984254242,-1.74689612655491E-11));
#30319=CARTESIAN_POINT('Ctrl Pts',(7.27603390512272,-113.493984254242,-4.20082013377291));
#30320=CARTESIAN_POINT('Ctrl Pts',(4.85068927007173,-113.318984254242,-8.40164026752836));
#30321=CARTESIAN_POINT('Ctrl Pts',(-1.51301075899711E-11,-113.143984254242,
-8.40164026751963));
#30322=CARTESIAN_POINT('Ctrl Pts',(-4.85068927010198,-112.968984254242,
-8.40164026751089));
#30323=CARTESIAN_POINT('Ctrl Pts',(-7.27603390513785,-112.793984254242,
-4.20082013374671));
#30324=CARTESIAN_POINT('Ctrl Pts',(-9.70137854017371,-112.618984254242,
1.74701493417668E-11));
#30325=CARTESIAN_POINT('Ctrl Pts',(-7.27603390512272,-112.443984254242,
4.20082013377291));
#30326=CARTESIAN_POINT('Ctrl Pts',(-4.85068927007173,-112.268984254242,
8.40164026752836));
#30327=CARTESIAN_POINT('Ctrl Pts',(1.5129078685785E-11,-112.093984254242,
8.40164026751963));
#30328=CARTESIAN_POINT('Ctrl Pts',(4.85068927010198,-111.918984254242,8.40164026751089));
#30329=CARTESIAN_POINT('Ctrl Pts',(7.27603390513785,-111.743984254242,4.20082013374671));
#30330=CARTESIAN_POINT('Ctrl Pts',(9.70137854017371,-111.568984254242,-1.74689612655491E-11));
#30331=CARTESIAN_POINT('Ctrl Pts',(7.27603390512272,-111.393984254242,-4.20082013377291));
#30332=CARTESIAN_POINT('Ctrl Pts',(4.85068927007173,-111.218984254242,-8.40164026752836));
#30333=CARTESIAN_POINT('Ctrl Pts',(-1.51301075899711E-11,-111.043984254242,
-8.40164026751963));
#30334=CARTESIAN_POINT('Ctrl Pts',(-4.85068927010198,-110.868984254242,
-8.40164026751089));
#30335=CARTESIAN_POINT('Ctrl Pts',(-7.27603390513785,-110.693984254242,
-4.20082013374671));
#30336=CARTESIAN_POINT('Ctrl Pts',(-9.70137854017371,-110.518984254242,
1.74701493417668E-11));
#30337=CARTESIAN_POINT('Ctrl Pts',(-7.27603390512272,-110.343984254242,
4.20082013377291));
#30338=CARTESIAN_POINT('Ctrl Pts',(-4.85068927007173,-110.168984254242,
8.40164026752836));
#30339=CARTESIAN_POINT('Ctrl Pts',(1.5129078685785E-11,-109.993984254242,
8.40164026751963));
#30340=CARTESIAN_POINT('Ctrl Pts',(4.85068927010198,-109.818984254242,8.40164026751089));
#30341=CARTESIAN_POINT('Ctrl Pts',(7.27603390513785,-109.643984254242,4.20082013374671));
#30342=CARTESIAN_POINT('Ctrl Pts',(9.70137854017371,-109.468984254242,-1.74689612655491E-11));
#30343=CARTESIAN_POINT('Ctrl Pts',(7.27603390512272,-109.293984254242,-4.20082013377291));
#30344=CARTESIAN_POINT('Ctrl Pts',(4.85068927007173,-109.118984254242,-8.40164026752836));
#30345=CARTESIAN_POINT('Ctrl Pts',(-1.51301075899711E-11,-108.943984254242,
-8.40164026751963));
#30346=CARTESIAN_POINT('Ctrl Pts',(-4.85068927010198,-108.768984254242,
-8.40164026751089));
#30347=CARTESIAN_POINT('Ctrl Pts',(-7.27603390513785,-108.593984254242,
-4.20082013374671));
#30348=CARTESIAN_POINT('Ctrl Pts',(-9.70137854017371,-108.418984254242,
1.74701493417668E-11));
#30349=CARTESIAN_POINT('Ctrl Pts',(-7.27603390512272,-108.243984254242,
4.20082013377291));
#30350=CARTESIAN_POINT('Ctrl Pts',(-4.85068927007173,-108.068984254242,
8.40164026752836));
#30351=CARTESIAN_POINT('Ctrl Pts',(1.5129078685785E-11,-107.893984254242,
8.40164026751963));
#30352=CARTESIAN_POINT('Ctrl Pts',(4.85068927010198,-107.718984254242,8.40164026751089));
#30353=CARTESIAN_POINT('Ctrl Pts',(7.27603390513785,-107.543984254242,4.20082013374671));
#30354=CARTESIAN_POINT('Ctrl Pts',(9.70137854017371,-107.368984254242,-1.74689612655491E-11));
#30355=CARTESIAN_POINT('Ctrl Pts',(7.27603390512272,-107.193984254242,-4.20082013377291));
#30356=CARTESIAN_POINT('Ctrl Pts',(4.85068927007173,-107.018984254242,-8.40164026752836));
#30357=CARTESIAN_POINT('Ctrl Pts',(-1.51301075899711E-11,-106.843984254242,
-8.40164026751963));
#30358=CARTESIAN_POINT('Ctrl Pts',(-4.85068927010198,-106.668984254242,
-8.40164026751089));
#30359=CARTESIAN_POINT('Ctrl Pts',(-7.27603390513785,-106.493984254242,
-4.20082013374671));
#30360=CARTESIAN_POINT('Ctrl Pts',(-9.70137854017371,-106.318984254242,
1.74701493417668E-11));
#30361=CARTESIAN_POINT('Ctrl Pts',(-7.27603390512272,-106.143984254242,
4.20082013377291));
#30362=CARTESIAN_POINT('Ctrl Pts',(-4.85068927007173,-105.968984254242,
8.40164026752836));
#30363=CARTESIAN_POINT('Ctrl Pts',(1.5129078685785E-11,-105.793984254242,
8.40164026751963));
#30364=CARTESIAN_POINT('Ctrl Pts',(4.85068927010198,-105.618984254242,8.40164026751089));
#30365=CARTESIAN_POINT('Ctrl Pts',(7.27603390513785,-105.443984254242,4.20082013374671));
#30366=CARTESIAN_POINT('Ctrl Pts',(9.70137854017371,-105.268984254242,-1.74689612655491E-11));
#30367=CARTESIAN_POINT('Ctrl Pts',(7.27603390512272,-105.093984254242,-4.20082013377291));
#30368=CARTESIAN_POINT('Ctrl Pts',(4.85068927007173,-104.918984254242,-8.40164026752836));
#30369=CARTESIAN_POINT('Ctrl Pts',(-1.51301075899711E-11,-104.743984254242,
-8.40164026751963));
#30370=CARTESIAN_POINT('Ctrl Pts',(-4.85068927010198,-104.568984254242,
-8.40164026751089));
#30371=CARTESIAN_POINT('Ctrl Pts',(-7.27603390513785,-104.393984254242,
-4.20082013374671));
#30372=CARTESIAN_POINT('Ctrl Pts',(-9.70137854017371,-104.218984254242,
1.74701493417668E-11));
#30373=CARTESIAN_POINT('Ctrl Pts',(-7.27603390512272,-104.043984254242,
4.20082013377291));
#30374=CARTESIAN_POINT('Ctrl Pts',(-4.85068927007173,-103.868984254242,
8.40164026752836));
#30375=CARTESIAN_POINT('Ctrl Pts',(1.5129078685785E-11,-103.693984254242,
8.40164026751963));
#30376=CARTESIAN_POINT('Ctrl Pts',(4.85068927010198,-103.518984254242,8.40164026751089));
#30377=CARTESIAN_POINT('Ctrl Pts',(7.27603390513785,-103.343984254242,4.20082013374671));
#30378=CARTESIAN_POINT('Ctrl Pts',(9.70137854017371,-103.168984254242,-1.74689612655491E-11));
#30379=CARTESIAN_POINT('Ctrl Pts',(7.27603390512272,-102.993984254242,-4.20082013377291));
#30380=CARTESIAN_POINT('Ctrl Pts',(4.85068927007173,-102.818984254242,-8.40164026752836));
#30381=CARTESIAN_POINT('Ctrl Pts',(-1.51301075899711E-11,-102.643984254242,
-8.40164026751963));
#30382=CARTESIAN_POINT('Ctrl Pts',(-4.85068927010198,-102.468984254242,
-8.40164026751089));
#30383=CARTESIAN_POINT('Ctrl Pts',(-7.27603390513785,-102.293984254242,
-4.20082013374671));
#30384=CARTESIAN_POINT('Ctrl Pts',(-9.70137854017371,-102.118984254242,
1.74701493417668E-11));
#30385=CARTESIAN_POINT('Ctrl Pts',(-7.27603390512272,-101.943984254242,
4.20082013377291));
#30386=CARTESIAN_POINT('Ctrl Pts',(-4.85068927007173,-101.768984254242,
8.40164026752836));
#30387=CARTESIAN_POINT('Ctrl Pts',(1.5129078685785E-11,-101.593984254242,
8.40164026751963));
#30388=CARTESIAN_POINT('Ctrl Pts',(4.85068927010198,-101.418984254242,8.40164026751089));
#30389=CARTESIAN_POINT('Ctrl Pts',(7.27603390513785,-101.243984254242,4.20082013374671));
#30390=CARTESIAN_POINT('Ctrl Pts',(9.70137854017371,-101.068984254242,-1.74689612655491E-11));
#30391=CARTESIAN_POINT('Ctrl Pts',(7.27603390512272,-100.893984254242,-4.20082013377291));
#30392=CARTESIAN_POINT('Ctrl Pts',(4.85068927007173,-100.718984254242,-8.40164026752836));
#30393=CARTESIAN_POINT('Ctrl Pts',(-1.51301075899711E-11,-100.543984254242,
-8.40164026751963));
#30394=CARTESIAN_POINT('Ctrl Pts',(-4.85068927010198,-100.368984254242,
-8.40164026751089));
#30395=CARTESIAN_POINT('Ctrl Pts',(-7.27603390513785,-100.193984254242,
-4.20082013374671));
#30396=CARTESIAN_POINT('Ctrl Pts',(-9.70137854017371,-100.018984254242,
1.74701493417668E-11));
#30397=CARTESIAN_POINT('Ctrl Pts',(-7.27603390512272,-99.8439842542419,
4.20082013377291));
#30398=CARTESIAN_POINT('Ctrl Pts',(-4.85068927007173,-99.6689842542419,
8.40164026752836));
#30399=CARTESIAN_POINT('Ctrl Pts',(1.5129078685785E-11,-99.4939842542419,
8.40164026751963));
#30400=CARTESIAN_POINT('Ctrl Pts',(4.85068927010198,-99.3189842542419,8.40164026751089));
#30401=CARTESIAN_POINT('Ctrl Pts',(7.27603390513785,-99.1439842542419,4.20082013374671));
#30402=CARTESIAN_POINT('Ctrl Pts',(9.70137854017371,-98.9689842542419,-1.74689612655491E-11));
#30403=CARTESIAN_POINT('Ctrl Pts',(7.27603390512272,-98.7939842542419,-4.20082013377291));
#30404=CARTESIAN_POINT('Ctrl Pts',(4.85068927007173,-98.6189842542419,-8.40164026752836));
#30405=CARTESIAN_POINT('Ctrl Pts',(-1.51301075899711E-11,-98.4439842542419,
-8.40164026751963));
#30406=CARTESIAN_POINT('Ctrl Pts',(-4.85068927010198,-98.2689842542419,
-8.40164026751089));
#30407=CARTESIAN_POINT('Ctrl Pts',(-7.27603390513785,-98.0939842542419,
-4.20082013374671));
#30408=CARTESIAN_POINT('Ctrl Pts',(-9.70137854017371,-97.9189842542419,
1.74701493417668E-11));
#30409=CARTESIAN_POINT('Ctrl Pts',(-7.27603390512272,-97.7439842542419,
4.20082013377291));
#30410=CARTESIAN_POINT('Ctrl Pts',(-4.85068927007173,-97.5689842542419,
8.40164026752836));
#30411=CARTESIAN_POINT('Ctrl Pts',(1.5129078685785E-11,-97.3939842542419,
8.40164026751963));
#30412=CARTESIAN_POINT('Ctrl Pts',(4.85068927010198,-97.2189842542419,8.40164026751089));
#30413=CARTESIAN_POINT('Ctrl Pts',(7.27603390513785,-97.0439842542419,4.20082013374671));
#30414=CARTESIAN_POINT('Ctrl Pts',(9.70137854017371,-96.8689842542419,-1.74689612655491E-11));
#30415=CARTESIAN_POINT('Ctrl Pts',(7.27603390512272,-96.6939842542419,-4.20082013377291));
#30416=CARTESIAN_POINT('Ctrl Pts',(4.85068927007173,-96.5189842542419,-8.40164026752836));
#30417=CARTESIAN_POINT('Ctrl Pts',(-1.51301075899711E-11,-96.3439842542419,
-8.40164026751963));
#30418=CARTESIAN_POINT('Ctrl Pts',(-4.85068927010198,-96.1689842542419,
-8.40164026751089));
#30419=CARTESIAN_POINT('Ctrl Pts',(-7.27603390513785,-95.9939842542419,
-4.20082013374671));
#30420=CARTESIAN_POINT('Ctrl Pts',(-9.70137854017371,-95.8189842542419,
1.74701493417668E-11));
#30421=CARTESIAN_POINT('Ctrl Pts',(-7.27603390512272,-95.6439842542419,
4.20082013377291));
#30422=CARTESIAN_POINT('Ctrl Pts',(-4.85068927007173,-95.4689842542419,
8.40164026752836));
#30423=CARTESIAN_POINT('Ctrl Pts',(1.5129078685785E-11,-95.2939842542419,
8.40164026751963));
#30424=CARTESIAN_POINT('Ctrl Pts',(4.85068927010198,-95.1189842542419,8.40164026751089));
#30425=CARTESIAN_POINT('Ctrl Pts',(7.27603390513785,-94.9439842542419,4.20082013374671));
#30426=CARTESIAN_POINT('Ctrl Pts',(9.70137854017371,-94.7689842542419,-1.74689612655491E-11));
#30427=CARTESIAN_POINT('Ctrl Pts',(7.27603390512272,-94.5939842542419,-4.20082013377291));
#30428=CARTESIAN_POINT('Ctrl Pts',(4.85068927007173,-94.4189842542419,-8.40164026752836));
#30429=CARTESIAN_POINT('Ctrl Pts',(-1.51301075899711E-11,-94.2439842542419,
-8.40164026751963));
#30430=CARTESIAN_POINT('Ctrl Pts',(-4.85068927010198,-94.0689842542419,
-8.40164026751089));
#30431=CARTESIAN_POINT('Ctrl Pts',(-7.27603390513785,-93.8939842542419,
-4.20082013374671));
#30432=CARTESIAN_POINT('Ctrl Pts',(-9.70137854017371,-93.7189842542419,
1.74701493417668E-11));
#30433=CARTESIAN_POINT('Ctrl Pts',(-7.27603390512272,-93.5439842542419,
4.20082013377291));
#30434=CARTESIAN_POINT('Ctrl Pts',(-4.85068927007173,-93.3689842542419,
8.40164026752836));
#30435=CARTESIAN_POINT('Ctrl Pts',(1.5129078685785E-11,-93.1939842542419,
8.40164026751963));
#30436=CARTESIAN_POINT('Ctrl Pts',(4.85068927010198,-93.0189842542419,8.40164026751089));
#30437=CARTESIAN_POINT('Ctrl Pts',(7.27603390513785,-92.8439842542419,4.20082013374671));
#30438=CARTESIAN_POINT('Ctrl Pts',(9.70137854017371,-92.6689842542419,-1.74689612655491E-11));
#30439=CARTESIAN_POINT('Ctrl Pts',(7.27603390512272,-92.4939842542419,-4.20082013377291));
#30440=CARTESIAN_POINT('Ctrl Pts',(4.85068927007173,-92.3189842542419,-8.40164026752836));
#30441=CARTESIAN_POINT('Ctrl Pts',(-1.51301075899711E-11,-92.1439842542419,
-8.40164026751963));
#30442=CARTESIAN_POINT('Ctrl Pts',(-4.85068927010198,-91.9689842542419,
-8.40164026751089));
#30443=CARTESIAN_POINT('Ctrl Pts',(-7.27603390513785,-91.7939842542419,
-4.20082013374671));
#30444=CARTESIAN_POINT('Ctrl Pts',(-9.70137854017371,-91.6189842542419,
1.74701493417668E-11));
#30445=CARTESIAN_POINT('Ctrl Pts',(-7.27603390512272,-91.4439842542419,
4.20082013377291));
#30446=CARTESIAN_POINT('Ctrl Pts',(-4.85068927007173,-91.2689842542419,
8.40164026752836));
#30447=CARTESIAN_POINT('Ctrl Pts',(1.5129078685785E-11,-91.0939842542419,
8.40164026751963));
#30448=CARTESIAN_POINT('Ctrl Pts',(4.85068927010198,-90.9189842542419,8.40164026751089));
#30449=CARTESIAN_POINT('Ctrl Pts',(7.27603390513785,-90.7439842542419,4.20082013374671));
#30450=CARTESIAN_POINT('Ctrl Pts',(9.70137854017371,-90.5689842542419,-1.74689612655491E-11));
#30451=CARTESIAN_POINT('Ctrl Pts',(7.27603390512272,-90.3939842542419,-4.20082013377291));
#30452=CARTESIAN_POINT('Ctrl Pts',(4.85068927007173,-90.2189842542419,-8.40164026752836));
#30453=CARTESIAN_POINT('Ctrl Pts',(-1.51301075899711E-11,-90.0439842542419,
-8.40164026751963));
#30454=CARTESIAN_POINT('Ctrl Pts',(-4.85068927010198,-89.8689842542419,
-8.40164026751089));
#30455=CARTESIAN_POINT('Ctrl Pts',(-7.27603390513785,-89.6939842542419,
-4.20082013374671));
#30456=CARTESIAN_POINT('Ctrl Pts',(-9.70137854017371,-89.5189842542419,
1.74701493417668E-11));
#30457=CARTESIAN_POINT('Ctrl Pts',(-7.27603390512272,-89.3439842542419,
4.20082013377291));
#30458=CARTESIAN_POINT('Ctrl Pts',(-4.85068927007173,-89.1689842542419,
8.40164026752836));
#30459=CARTESIAN_POINT('Ctrl Pts',(1.5129078685785E-11,-88.9939842542419,
8.40164026751963));
#30460=CARTESIAN_POINT('Ctrl Pts',(4.85068927010198,-88.8189842542419,8.40164026751089));
#30461=CARTESIAN_POINT('Ctrl Pts',(7.27603390513785,-88.6439842542419,4.20082013374671));
#30462=CARTESIAN_POINT('Ctrl Pts',(9.70137854017371,-88.4689842542419,-1.74689612655491E-11));
#30463=CARTESIAN_POINT('Ctrl Pts',(7.27603390512272,-88.2939842542419,-4.20082013377291));
#30464=CARTESIAN_POINT('Ctrl Pts',(4.85068927007173,-88.1189842542419,-8.40164026752836));
#30465=CARTESIAN_POINT('Ctrl Pts',(-1.51301075899711E-11,-87.9439842542419,
-8.40164026751963));
#30466=CARTESIAN_POINT('Ctrl Pts',(-4.85068927010198,-87.7689842542419,
-8.40164026751089));
#30467=CARTESIAN_POINT('Ctrl Pts',(-7.27603390513785,-87.5939842542419,
-4.20082013374671));
#30468=CARTESIAN_POINT('Ctrl Pts',(-9.70137854017371,-87.4189842542419,
1.74701493417668E-11));
#30469=CARTESIAN_POINT('Ctrl Pts',(-7.27603390512272,-87.2439842542419,
4.20082013377291));
#30470=CARTESIAN_POINT('Ctrl Pts',(-4.85068927007173,-87.0689842542419,
8.40164026752836));
#30471=CARTESIAN_POINT('Ctrl Pts',(1.5129078685785E-11,-86.8939842542419,
8.40164026751963));
#30472=CARTESIAN_POINT('Ctrl Pts',(4.85068927010198,-86.7189842542419,8.40164026751089));
#30473=CARTESIAN_POINT('Ctrl Pts',(7.27603390513785,-86.5439842542419,4.20082013374671));
#30474=CARTESIAN_POINT('Ctrl Pts',(9.70137854017371,-86.3689842542419,-1.74689612655491E-11));
#30475=CARTESIAN_POINT('Ctrl Pts',(7.27603390512272,-86.1939842542419,-4.20082013377291));
#30476=CARTESIAN_POINT('Ctrl Pts',(4.85068927007173,-86.0189842542419,-8.40164026752836));
#30477=CARTESIAN_POINT('Ctrl Pts',(-1.51301075899711E-11,-85.8439842542419,
-8.40164026751963));
#30478=CARTESIAN_POINT('Ctrl Pts',(-4.85068927010198,-85.6689842542419,
-8.40164026751089));
#30479=CARTESIAN_POINT('Ctrl Pts',(-7.27603390513785,-85.4939842542419,
-4.20082013374671));
#30480=CARTESIAN_POINT('Ctrl Pts',(-9.70137854017371,-85.3189842542419,
1.74701493417668E-11));
#30481=CARTESIAN_POINT('Ctrl Pts',(-7.27603390512272,-85.143984254242,4.20082013377291));
#30482=CARTESIAN_POINT('Ctrl Pts',(-4.85068927007173,-84.9689842542419,
8.40164026752836));
#30483=CARTESIAN_POINT('Ctrl Pts',(1.5129078685785E-11,-84.7939842542419,
8.40164026751963));
#30484=CARTESIAN_POINT('Ctrl Pts',(4.85068927010198,-84.6189842542419,8.40164026751089));
#30485=CARTESIAN_POINT('Ctrl Pts',(7.27603390513785,-84.443984254242,4.20082013374671));
#30486=CARTESIAN_POINT('Ctrl Pts',(9.70137854017371,-84.2689842542419,-1.74689612655491E-11));
#30487=CARTESIAN_POINT('Ctrl Pts',(7.27603390512272,-84.0939842542419,-4.20082013377291));
#30488=CARTESIAN_POINT('Ctrl Pts',(4.85068927007173,-83.9189842542419,-8.40164026752836));
#30489=CARTESIAN_POINT('Ctrl Pts',(-1.51301075899711E-11,-83.7439842542419,
-8.40164026751963));
#30490=CARTESIAN_POINT('Ctrl Pts',(-4.85068927010198,-83.5689842542419,
-8.40164026751089));
#30491=CARTESIAN_POINT('Ctrl Pts',(-7.27603390513785,-83.3939842542419,
-4.20082013374671));
#30492=CARTESIAN_POINT('Ctrl Pts',(-9.70137854017371,-83.2189842542419,
1.74701493417668E-11));
#30493=CARTESIAN_POINT('Ctrl Pts',(-7.27603390512272,-83.0439842542419,
4.20082013377291));
#30494=CARTESIAN_POINT('Ctrl Pts',(-4.85068927007173,-82.868984254242,8.40164026752836));
#30495=CARTESIAN_POINT('Ctrl Pts',(1.5129078685785E-11,-82.6939842542419,
8.40164026751963));
#30496=CARTESIAN_POINT('Ctrl Pts',(4.85068927010198,-82.5189842542419,8.40164026751089));
#30497=CARTESIAN_POINT('Ctrl Pts',(7.27603390513785,-82.3439842542419,4.20082013374671));
#30498=CARTESIAN_POINT('Ctrl Pts',(9.70137854017371,-82.1689842542419,-1.74689612655491E-11));
#30499=CARTESIAN_POINT('Ctrl Pts',(7.27603390512272,-81.993984254242,-4.20082013377291));
#30500=CARTESIAN_POINT('Ctrl Pts',(4.85068927007173,-81.8189842542419,-8.40164026752836));
#30501=CARTESIAN_POINT('Ctrl Pts',(-1.51301075899711E-11,-81.6439842542419,
-8.40164026751963));
#30502=CARTESIAN_POINT('Ctrl Pts',(-4.85068927010198,-81.4689842542419,
-8.40164026751089));
#30503=CARTESIAN_POINT('Ctrl Pts',(-7.27603390513785,-81.293984254242,-4.20082013374671));
#30504=CARTESIAN_POINT('Ctrl Pts',(-9.70137854017371,-81.1189842542419,
1.74701493417668E-11));
#30505=CARTESIAN_POINT('Ctrl Pts',(-7.27603390512272,-80.9439842542419,
4.20082013377291));
#30506=CARTESIAN_POINT('Ctrl Pts',(-4.85068927007173,-80.768984254242,8.40164026752836));
#30507=CARTESIAN_POINT('Ctrl Pts',(1.5129078685785E-11,-80.5939842542419,
8.40164026751963));
#30508=CARTESIAN_POINT('Ctrl Pts',(4.85068927010198,-80.4189842542419,8.40164026751089));
#30509=CARTESIAN_POINT('Ctrl Pts',(7.27603390513785,-80.243984254242,4.20082013374671));
#30510=CARTESIAN_POINT('Ctrl Pts',(9.70137854017371,-80.068984254242,-1.74689612655491E-11));
#30511=CARTESIAN_POINT('Ctrl Pts',(7.27603390512272,-79.8939842542419,-4.20082013377291));
#30512=CARTESIAN_POINT('Ctrl Pts',(4.85068927007173,-79.7189842542419,-8.40164026752836));
#30513=CARTESIAN_POINT('Ctrl Pts',(-1.51301075899711E-11,-79.5439842542419,
-8.40164026751963));
#30514=CARTESIAN_POINT('Ctrl Pts',(-4.85068927010198,-79.368984254242,-8.40164026751089));
#30515=CARTESIAN_POINT('Ctrl Pts',(-7.27603390513785,-79.193984254242,-4.20082013374671));
#30516=CARTESIAN_POINT('Ctrl Pts',(-9.70137854017371,-79.0189842542419,
1.74701493417668E-11));
#30517=CARTESIAN_POINT('Ctrl Pts',(-7.27603390512272,-78.8439842542419,
4.20082013377291));
#30518=CARTESIAN_POINT('Ctrl Pts',(-4.85068927007173,-78.668984254242,8.40164026752836));
#30519=CARTESIAN_POINT('Ctrl Pts',(1.5129078685785E-11,-78.493984254242,
8.40164026751963));
#30520=CARTESIAN_POINT('Ctrl Pts',(4.85068927010198,-78.3189842542419,8.40164026751089));
#30521=CARTESIAN_POINT('Ctrl Pts',(7.27603390513785,-78.143984254242,4.20082013374671));
#30522=CARTESIAN_POINT('Ctrl Pts',(9.70137854017371,-77.968984254242,-1.74689612655491E-11));
#30523=CARTESIAN_POINT('Ctrl Pts',(7.27603390512272,-77.7939842542419,-4.20082013377291));
#30524=CARTESIAN_POINT('Ctrl Pts',(4.85068927007173,-77.618984254242,-8.40164026752836));
#30525=CARTESIAN_POINT('Ctrl Pts',(-1.51301075899711E-11,-77.443984254242,
-8.40164026751963));
#30526=CARTESIAN_POINT('Ctrl Pts',(-4.85068927010198,-77.268984254242,-8.40164026751089));
#30527=CARTESIAN_POINT('Ctrl Pts',(-7.27603390513785,-77.0939842542419,
-4.20082013374671));
#30528=CARTESIAN_POINT('Ctrl Pts',(-9.70137854017371,-76.918984254242,1.74701493417668E-11));
#30529=CARTESIAN_POINT('Ctrl Pts',(-7.27603390512272,-76.743984254242,4.20082013377291));
#30530=CARTESIAN_POINT('Ctrl Pts',(-4.85068927007173,-76.5689842542419,
8.40164026752836));
#30531=CARTESIAN_POINT('Ctrl Pts',(1.5129078685785E-11,-76.393984254242,
8.40164026751963));
#30532=CARTESIAN_POINT('Ctrl Pts',(4.85068927010198,-76.218984254242,8.40164026751089));
#30533=CARTESIAN_POINT('Ctrl Pts',(7.27603390513785,-76.0439842542419,4.20082013374671));
#30534=CARTESIAN_POINT('Ctrl Pts',(9.70137854017371,-75.868984254242,-1.74689612655491E-11));
#30535=CARTESIAN_POINT('Ctrl Pts',(7.27603390512272,-75.693984254242,-4.20082013377291));
#30536=CARTESIAN_POINT('Ctrl Pts',(4.85068927007173,-75.518984254242,-8.40164026752836));
#30537=CARTESIAN_POINT('Ctrl Pts',(-1.51301075899711E-11,-75.343984254242,
-8.40164026751963));
#30538=CARTESIAN_POINT('Ctrl Pts',(-4.85068927010198,-75.1689842542419,
-8.40164026751089));
#30539=CARTESIAN_POINT('Ctrl Pts',(-7.27603390513785,-74.993984254242,-4.20082013374671));
#30540=CARTESIAN_POINT('Ctrl Pts',(-9.70137854017371,-74.818984254242,1.74701493417668E-11));
#30541=CARTESIAN_POINT('Ctrl Pts',(-7.27603390512272,-74.643984254242,4.20082013377291));
#30542=CARTESIAN_POINT('Ctrl Pts',(-4.85068927007173,-74.4689842542419,
8.40164026752836));
#30543=CARTESIAN_POINT('Ctrl Pts',(1.5129078685785E-11,-74.293984254242,
8.40164026751963));
#30544=CARTESIAN_POINT('Ctrl Pts',(4.85068927010198,-74.118984254242,8.40164026751089));
#30545=CARTESIAN_POINT('Ctrl Pts',(7.27603390513785,-73.943984254242,4.20082013374671));
#30546=CARTESIAN_POINT('Ctrl Pts',(9.70137854017371,-73.768984254242,-1.74689612655491E-11));
#30547=CARTESIAN_POINT('Ctrl Pts',(7.27603390512272,-73.593984254242,-4.20082013377291));
#30548=CARTESIAN_POINT('Ctrl Pts',(4.85068927007173,-73.4189842542419,-8.40164026752836));
#30549=CARTESIAN_POINT('Ctrl Pts',(-1.51301075899711E-11,-73.243984254242,
-8.40164026751963));
#30550=CARTESIAN_POINT('Ctrl Pts',(-4.85068927010198,-73.068984254242,-8.40164026751089));
#30551=CARTESIAN_POINT('Ctrl Pts',(-7.27603390513785,-72.893984254242,-4.20082013374671));
#30552=CARTESIAN_POINT('Ctrl Pts',(-9.70137854017371,-72.718984254242,1.74701493417668E-11));
#30553=CARTESIAN_POINT('Ctrl Pts',(-7.27603390512272,-72.543984254242,4.20082013377291));
#30554=CARTESIAN_POINT('Ctrl Pts',(-4.85068927007173,-72.368984254242,8.40164026752836));
#30555=CARTESIAN_POINT('Ctrl Pts',(1.5129078685785E-11,-72.193984254242,
8.40164026751963));
#30556=CARTESIAN_POINT('Ctrl Pts',(4.85068927010198,-72.018984254242,8.40164026751089));
#30557=CARTESIAN_POINT('Ctrl Pts',(7.27603390513785,-71.843984254242,4.20082013374671));
#30558=CARTESIAN_POINT('Ctrl Pts',(9.70137854017371,-71.6689842542419,-1.74689612655491E-11));
#30559=CARTESIAN_POINT('Ctrl Pts',(7.27603390512272,-71.493984254242,-4.20082013377291));
#30560=CARTESIAN_POINT('Ctrl Pts',(4.85068927007173,-71.318984254242,-8.40164026752836));
#30561=CARTESIAN_POINT('Ctrl Pts',(-1.51301075899711E-11,-71.143984254242,
-8.40164026751963));
#30562=CARTESIAN_POINT('Ctrl Pts',(-4.85068927010198,-70.968984254242,-8.40164026751089));
#30563=CARTESIAN_POINT('Ctrl Pts',(-7.27603390513785,-70.793984254242,-4.20082013374671));
#30564=CARTESIAN_POINT('Ctrl Pts',(-9.70137854017371,-70.618984254242,1.74701493417668E-11));
#30565=CARTESIAN_POINT('Ctrl Pts',(-7.27603390512272,-70.443984254242,4.20082013377291));
#30566=CARTESIAN_POINT('Ctrl Pts',(-4.85068927007173,-70.268984254242,8.40164026752836));
#30567=CARTESIAN_POINT('Ctrl Pts',(1.5129078685785E-11,-70.093984254242,
8.40164026751963));
#30568=CARTESIAN_POINT('Ctrl Pts',(4.85068927010198,-69.918984254242,8.40164026751089));
#30569=CARTESIAN_POINT('Ctrl Pts',(7.27603390513785,-69.743984254242,4.20082013374671));
#30570=CARTESIAN_POINT('Ctrl Pts',(9.70137854017371,-69.568984254242,-1.74689612655491E-11));
#30571=CARTESIAN_POINT('Ctrl Pts',(7.27603390512272,-69.393984254242,-4.20082013377291));
#30572=CARTESIAN_POINT('Ctrl Pts',(4.85068927007173,-69.218984254242,-8.40164026752836));
#30573=CARTESIAN_POINT('Ctrl Pts',(-1.51301075899711E-11,-69.043984254242,
-8.40164026751963));
#30574=CARTESIAN_POINT('Ctrl Pts',(-4.85068927010198,-68.868984254242,-8.40164026751089));
#30575=CARTESIAN_POINT('Ctrl Pts',(-7.27603390513785,-68.693984254242,-4.20082013374671));
#30576=CARTESIAN_POINT('Ctrl Pts',(-9.70137854017371,-68.518984254242,1.74701493417668E-11));
#30577=CARTESIAN_POINT('Ctrl Pts',(-7.27603390512272,-68.343984254242,4.20082013377291));
#30578=CARTESIAN_POINT('Ctrl Pts',(-4.85068927007173,-68.168984254242,8.40164026752836));
#30579=CARTESIAN_POINT('Ctrl Pts',(1.5129078685785E-11,-67.993984254242,
8.40164026751963));
#30580=CARTESIAN_POINT('Ctrl Pts',(4.85068927010198,-67.818984254242,8.40164026751089));
#30581=CARTESIAN_POINT('Ctrl Pts',(7.27603390513785,-67.643984254242,4.20082013374671));
#30582=CARTESIAN_POINT('Ctrl Pts',(9.70137854017371,-67.468984254242,-1.74689612655491E-11));
#30583=CARTESIAN_POINT('Ctrl Pts',(7.27603390512272,-67.293984254242,-4.20082013377291));
#30584=CARTESIAN_POINT('Ctrl Pts',(4.85068927007173,-67.118984254242,-8.40164026752836));
#30585=CARTESIAN_POINT('Ctrl Pts',(-1.51301075899711E-11,-66.943984254242,
-8.40164026751963));
#30586=CARTESIAN_POINT('Ctrl Pts',(-4.85068927010198,-66.768984254242,-8.40164026751089));
#30587=CARTESIAN_POINT('Ctrl Pts',(-7.27603390513785,-66.593984254242,-4.20082013374671));
#30588=CARTESIAN_POINT('Ctrl Pts',(-9.70137854017371,-66.418984254242,1.74701493417668E-11));
#30589=CARTESIAN_POINT('Ctrl Pts',(-7.27603390512272,-66.243984254242,4.20082013377291));
#30590=CARTESIAN_POINT('Ctrl Pts',(-4.85068927007173,-66.068984254242,8.40164026752836));
#30591=CARTESIAN_POINT('Ctrl Pts',(1.5129078685785E-11,-65.893984254242,
8.40164026751963));
#30592=CARTESIAN_POINT('Ctrl Pts',(4.85068927010198,-65.718984254242,8.40164026751089));
#30593=CARTESIAN_POINT('Ctrl Pts',(7.27603390513785,-65.543984254242,4.20082013374671));
#30594=CARTESIAN_POINT('Ctrl Pts',(9.70137854017371,-65.368984254242,-1.74689612655491E-11));
#30595=CARTESIAN_POINT('Ctrl Pts',(7.27603390512272,-65.193984254242,-4.20082013377291));
#30596=CARTESIAN_POINT('Ctrl Pts',(4.85068927007173,-65.018984254242,-8.40164026752836));
#30597=CARTESIAN_POINT('Ctrl Pts',(-1.51301075899711E-11,-64.843984254242,
-8.40164026751963));
#30598=CARTESIAN_POINT('Ctrl Pts',(-4.85068927010198,-64.668984254242,-8.40164026751089));
#30599=CARTESIAN_POINT('Ctrl Pts',(-7.27603390513785,-64.493984254242,-4.20082013374671));
#30600=CARTESIAN_POINT('Ctrl Pts',(-9.70137854017371,-64.318984254242,1.74701493417668E-11));
#30601=CARTESIAN_POINT('Ctrl Pts',(-7.27603390512272,-64.143984254242,4.20082013377291));
#30602=CARTESIAN_POINT('Ctrl Pts',(-4.85068927007173,-63.968984254242,8.40164026752836));
#30603=CARTESIAN_POINT('Ctrl Pts',(1.5129078685785E-11,-63.793984254242,
8.40164026751963));
#30604=CARTESIAN_POINT('Ctrl Pts',(4.85068927010198,-63.618984254242,8.40164026751089));
#30605=CARTESIAN_POINT('Ctrl Pts',(7.27603390513785,-63.443984254242,4.20082013374671));
#30606=CARTESIAN_POINT('Ctrl Pts',(9.70137854017371,-63.268984254242,-1.74689612655491E-11));
#30607=CARTESIAN_POINT('Ctrl Pts',(7.27603390512272,-63.093984254242,-4.20082013377291));
#30608=CARTESIAN_POINT('Ctrl Pts',(4.85068927007173,-62.918984254242,-8.40164026752836));
#30609=CARTESIAN_POINT('Ctrl Pts',(-1.51301075899711E-11,-62.743984254242,
-8.40164026751963));
#30610=CARTESIAN_POINT('Ctrl Pts',(-4.85068927010198,-62.568984254242,-8.40164026751089));
#30611=CARTESIAN_POINT('Ctrl Pts',(-7.27603390513785,-62.393984254242,-4.20082013374671));
#30612=CARTESIAN_POINT('Ctrl Pts',(-9.70137854017371,-62.218984254242,1.74701493417668E-11));
#30613=CARTESIAN_POINT('Ctrl Pts',(-7.27603390512272,-62.043984254242,4.20082013377291));
#30614=CARTESIAN_POINT('Ctrl Pts',(-4.85068927007173,-61.868984254242,8.40164026752836));
#30615=CARTESIAN_POINT('Ctrl Pts',(1.5129078685785E-11,-61.693984254242,
8.40164026751963));
#30616=CARTESIAN_POINT('Ctrl Pts',(4.85068927010198,-61.518984254242,8.40164026751089));
#30617=CARTESIAN_POINT('Ctrl Pts',(7.27603390513785,-61.343984254242,4.20082013374671));
#30618=CARTESIAN_POINT('Ctrl Pts',(9.70137854017371,-61.168984254242,-1.74689612655491E-11));
#30619=CARTESIAN_POINT('Ctrl Pts',(7.27603390512272,-60.993984254242,-4.20082013377291));
#30620=CARTESIAN_POINT('Ctrl Pts',(4.85068927007173,-60.818984254242,-8.40164026752836));
#30621=CARTESIAN_POINT('Ctrl Pts',(-1.51301075899711E-11,-60.643984254242,
-8.40164026751963));
#30622=CARTESIAN_POINT('Ctrl Pts',(-4.85068927010198,-60.468984254242,-8.40164026751089));
#30623=CARTESIAN_POINT('Ctrl Pts',(-7.27603390513785,-60.293984254242,-4.20082013374671));
#30624=CARTESIAN_POINT('Ctrl Pts',(-9.70137854017371,-60.118984254242,1.74701493417668E-11));
#30625=CARTESIAN_POINT('Ctrl Pts',(-7.27603390512272,-59.943984254242,4.20082013377291));
#30626=CARTESIAN_POINT('Ctrl Pts',(-4.85068927007173,-59.768984254242,8.40164026752836));
#30627=CARTESIAN_POINT('Ctrl Pts',(1.5129078685785E-11,-59.593984254242,
8.40164026751963));
#30628=CARTESIAN_POINT('Ctrl Pts',(4.85068927010198,-59.418984254242,8.40164026751089));
#30629=CARTESIAN_POINT('Ctrl Pts',(7.27603390513785,-59.243984254242,4.20082013374671));
#30630=CARTESIAN_POINT('Ctrl Pts',(9.70137854017371,-59.068984254242,-1.74689612655491E-11));
#30631=CARTESIAN_POINT('Ctrl Pts',(7.27603390512272,-58.893984254242,-4.20082013377291));
#30632=CARTESIAN_POINT('Ctrl Pts',(4.85068927007173,-58.718984254242,-8.40164026752836));
#30633=CARTESIAN_POINT('Ctrl Pts',(-1.51301075899711E-11,-58.543984254242,
-8.40164026751963));
#30634=CARTESIAN_POINT('Ctrl Pts',(-4.85068927010198,-58.368984254242,-8.40164026751089));
#30635=CARTESIAN_POINT('Ctrl Pts',(-7.27603390513785,-58.193984254242,-4.20082013374671));
#30636=CARTESIAN_POINT('Ctrl Pts',(-9.70137854017371,-58.018984254242,1.74701493417668E-11));
#30637=CARTESIAN_POINT('Ctrl Pts',(-7.27603390512272,-57.843984254242,4.20082013377291));
#30638=CARTESIAN_POINT('Ctrl Pts',(-4.85068927007173,-57.668984254242,8.40164026752836));
#30639=CARTESIAN_POINT('Ctrl Pts',(1.5129078685785E-11,-57.493984254242,
8.40164026751963));
#30640=CARTESIAN_POINT('Ctrl Pts',(4.85068927010198,-57.318984254242,8.40164026751089));
#30641=CARTESIAN_POINT('Ctrl Pts',(7.27603390513785,-57.143984254242,4.20082013374671));
#30642=CARTESIAN_POINT('Ctrl Pts',(9.70137854017371,-56.968984254242,-1.74689612655491E-11));
#30643=CARTESIAN_POINT('Ctrl Pts',(7.27603390512272,-56.793984254242,-4.20082013377291));
#30644=CARTESIAN_POINT('Ctrl Pts',(4.85068927007173,-56.618984254242,-8.40164026752836));
#30645=CARTESIAN_POINT('Ctrl Pts',(-1.51301075899711E-11,-56.443984254242,
-8.40164026751963));
#30646=CARTESIAN_POINT('Ctrl Pts',(-4.85068927010198,-56.268984254242,-8.40164026751089));
#30647=CARTESIAN_POINT('Ctrl Pts',(-7.27603390513785,-56.093984254242,-4.20082013374671));
#30648=CARTESIAN_POINT('Ctrl Pts',(-9.70137854017371,-55.918984254242,1.74701493417668E-11));
#30649=CARTESIAN_POINT('Ctrl Pts',(-7.27603390512272,-55.743984254242,4.20082013377291));
#30650=CARTESIAN_POINT('Ctrl Pts',(-4.85068927007173,-55.568984254242,8.40164026752836));
#30651=CARTESIAN_POINT('Ctrl Pts',(1.5129078685785E-11,-55.393984254242,
8.40164026751963));
#30652=CARTESIAN_POINT('Ctrl Pts',(4.85068927010198,-55.218984254242,8.40164026751089));
#30653=CARTESIAN_POINT('Ctrl Pts',(7.27603390513785,-55.043984254242,4.20082013374671));
#30654=CARTESIAN_POINT('Ctrl Pts',(9.70137854017371,-54.868984254242,-1.74689612655491E-11));
#30655=CARTESIAN_POINT('Ctrl Pts',(7.27603390512272,-54.693984254242,-4.20082013377291));
#30656=CARTESIAN_POINT('Ctrl Pts',(4.85068927007173,-54.518984254242,-8.40164026752836));
#30657=CARTESIAN_POINT('Ctrl Pts',(-1.51301075899711E-11,-54.343984254242,
-8.40164026751963));
#30658=CARTESIAN_POINT('Ctrl Pts',(-4.85068927010198,-54.168984254242,-8.40164026751089));
#30659=CARTESIAN_POINT('Ctrl Pts',(-7.27603390513785,-53.993984254242,-4.20082013374671));
#30660=CARTESIAN_POINT('Ctrl Pts',(-9.70137854017371,-53.818984254242,1.74701493417668E-11));
#30661=CARTESIAN_POINT('Ctrl Pts',(-7.27603390512272,-53.643984254242,4.20082013377291));
#30662=CARTESIAN_POINT('Ctrl Pts',(-4.85068927007173,-53.468984254242,8.40164026752836));
#30663=CARTESIAN_POINT('Ctrl Pts',(1.5129078685785E-11,-53.293984254242,
8.40164026751963));
#30664=CARTESIAN_POINT('Ctrl Pts',(4.85068927010198,-53.118984254242,8.40164026751089));
#30665=CARTESIAN_POINT('Ctrl Pts',(7.27603390513785,-52.943984254242,4.20082013374671));
#30666=CARTESIAN_POINT('Ctrl Pts',(9.70137854017371,-52.768984254242,-1.74689612655491E-11));
#30667=CARTESIAN_POINT('Ctrl Pts',(7.27603390512272,-52.593984254242,-4.20082013377291));
#30668=CARTESIAN_POINT('Ctrl Pts',(4.85068927007173,-52.418984254242,-8.40164026752836));
#30669=CARTESIAN_POINT('Ctrl Pts',(-1.51301075899711E-11,-52.243984254242,
-8.40164026751963));
#30670=CARTESIAN_POINT('Ctrl Pts',(-4.85068927010198,-52.068984254242,-8.40164026751089));
#30671=CARTESIAN_POINT('Ctrl Pts',(-7.27603390513785,-51.893984254242,-4.20082013374671));
#30672=CARTESIAN_POINT('Ctrl Pts',(-9.70137854017371,-51.718984254242,1.74701493417668E-11));
#30673=CARTESIAN_POINT('Ctrl Pts',(-7.27603390512272,-51.543984254242,4.20082013377291));
#30674=CARTESIAN_POINT('Ctrl Pts',(-4.85068927007173,-51.368984254242,8.40164026752836));
#30675=CARTESIAN_POINT('Ctrl Pts',(1.5129078685785E-11,-51.193984254242,
8.40164026751963));
#30676=CARTESIAN_POINT('Ctrl Pts',(4.85068927010198,-51.018984254242,8.40164026751089));
#30677=CARTESIAN_POINT('Ctrl Pts',(7.27603390513785,-50.843984254242,4.20082013374671));
#30678=CARTESIAN_POINT('Ctrl Pts',(9.70137854017371,-50.668984254242,-1.74689612655491E-11));
#30679=CARTESIAN_POINT('Ctrl Pts',(7.27603390512272,-50.493984254242,-4.20082013377291));
#30680=CARTESIAN_POINT('Ctrl Pts',(4.85068927007173,-50.318984254242,-8.40164026752836));
#30681=CARTESIAN_POINT('Ctrl Pts',(-1.51301075899711E-11,-50.143984254242,
-8.40164026751963));
#30682=CARTESIAN_POINT('Ctrl Pts',(-4.85068927010198,-49.968984254242,-8.40164026751089));
#30683=CARTESIAN_POINT('Ctrl Pts',(-7.27603390513785,-49.793984254242,-4.20082013374671));
#30684=CARTESIAN_POINT('Ctrl Pts',(-9.70137854017371,-49.618984254242,1.74701493417668E-11));
#30685=CARTESIAN_POINT('Ctrl Pts',(-7.27603390512272,-49.443984254242,4.20082013377291));
#30686=CARTESIAN_POINT('Ctrl Pts',(-4.85068927007173,-49.268984254242,8.40164026752836));
#30687=CARTESIAN_POINT('Ctrl Pts',(1.5129078685785E-11,-49.093984254242,
8.40164026751963));
#30688=CARTESIAN_POINT('Ctrl Pts',(4.85068927010198,-48.918984254242,8.40164026751089));
#30689=CARTESIAN_POINT('Ctrl Pts',(7.27603390513785,-48.743984254242,4.20082013374671));
#30690=CARTESIAN_POINT('Ctrl Pts',(9.70137854017371,-48.568984254242,-1.74689612655491E-11));
#30691=CARTESIAN_POINT('Ctrl Pts',(7.27603390512272,-48.393984254242,-4.20082013377291));
#30692=CARTESIAN_POINT('Ctrl Pts',(4.85068927007173,-48.218984254242,-8.40164026752836));
#30693=CARTESIAN_POINT('Ctrl Pts',(-1.51301075899711E-11,-48.043984254242,
-8.40164026751963));
#30694=CARTESIAN_POINT('Ctrl Pts',(-4.85068927010198,-47.868984254242,-8.40164026751089));
#30695=CARTESIAN_POINT('Ctrl Pts',(-7.27603390513785,-47.693984254242,-4.20082013374671));
#30696=CARTESIAN_POINT('Ctrl Pts',(-9.70137854017371,-47.518984254242,1.74701493417668E-11));
#30697=CARTESIAN_POINT('Ctrl Pts',(-7.27603390512272,-47.343984254242,4.20082013377291));
#30698=CARTESIAN_POINT('Ctrl Pts',(-4.85068927007173,-47.168984254242,8.40164026752836));
#30699=CARTESIAN_POINT('Ctrl Pts',(1.5129078685785E-11,-46.993984254242,
8.40164026751963));
#30700=CARTESIAN_POINT('Ctrl Pts',(4.85068927010198,-46.818984254242,8.40164026751089));
#30701=CARTESIAN_POINT('Ctrl Pts',(7.27603390513785,-46.643984254242,4.20082013374671));
#30702=CARTESIAN_POINT('Ctrl Pts',(9.70137854017371,-46.468984254242,-1.74689612655491E-11));
#30703=CARTESIAN_POINT('Ctrl Pts',(7.27603390512272,-46.293984254242,-4.20082013377291));
#30704=CARTESIAN_POINT('Ctrl Pts',(4.85068927007173,-46.118984254242,-8.40164026752836));
#30705=CARTESIAN_POINT('Ctrl Pts',(-1.51301075899711E-11,-45.943984254242,
-8.40164026751963));
#30706=CARTESIAN_POINT('Ctrl Pts',(-4.85068927010198,-45.768984254242,-8.40164026751089));
#30707=CARTESIAN_POINT('Ctrl Pts',(-7.27603390513785,-45.593984254242,-4.20082013374671));
#30708=CARTESIAN_POINT('Ctrl Pts',(-9.70137854017371,-45.418984254242,1.74701493417668E-11));
#30709=CARTESIAN_POINT('Ctrl Pts',(-7.27603390512272,-45.243984254242,4.20082013377291));
#30710=CARTESIAN_POINT('Ctrl Pts',(-4.85068927007173,-45.068984254242,8.40164026752836));
#30711=CARTESIAN_POINT('Ctrl Pts',(1.5129078685785E-11,-44.893984254242,
8.40164026751963));
#30712=CARTESIAN_POINT('Ctrl Pts',(4.85068927010198,-44.718984254242,8.40164026751089));
#30713=CARTESIAN_POINT('Ctrl Pts',(7.27603390513785,-44.543984254242,4.20082013374671));
#30714=CARTESIAN_POINT('Ctrl Pts',(9.70137854017371,-44.368984254242,-1.74689612655491E-11));
#30715=CARTESIAN_POINT('Ctrl Pts',(7.27603390512272,-44.193984254242,-4.20082013377291));
#30716=CARTESIAN_POINT('Ctrl Pts',(4.85068927007173,-44.018984254242,-8.40164026752836));
#30717=CARTESIAN_POINT('Ctrl Pts',(-1.51301075899711E-11,-43.843984254242,
-8.40164026751963));
#30718=CARTESIAN_POINT('',(5.91264939824166,-212.63,5.96893091585754));
#30719=CARTESIAN_POINT('Ctrl Pts',(5.91264939824165,-212.63,5.96893091585754));
#30720=CARTESIAN_POINT('Ctrl Pts',(6.71286052373726,-212.584619857249,5.17626504380697));
#30721=CARTESIAN_POINT('Ctrl Pts',(7.27603390513785,-212.543984254242,4.20082013374672));
#30722=CARTESIAN_POINT('Ctrl Pts',(9.70137854017372,-212.368984254242,-1.74689612655491E-11));
#30723=CARTESIAN_POINT('Ctrl Pts',(7.27603390512273,-212.193984254242,-4.20082013377291));
#30724=CARTESIAN_POINT('Ctrl Pts',(4.85068927007173,-212.018984254242,-8.40164026752836));
#30725=CARTESIAN_POINT('Ctrl Pts',(-1.51280497815988E-11,-211.843984254242,
-8.40164026751963));
#30726=CARTESIAN_POINT('Ctrl Pts',(-4.85068927010198,-211.668984254242,
-8.4016402675109));
#30727=CARTESIAN_POINT('Ctrl Pts',(-7.27603390513785,-211.493984254242,
-4.20082013374672));
#30728=CARTESIAN_POINT('Ctrl Pts',(-9.70137854017372,-211.318984254242,
1.74591566342707E-11));
#30729=CARTESIAN_POINT('Ctrl Pts',(-7.27603390512273,-211.143984254242,
4.20082013377291));
#30730=CARTESIAN_POINT('Ctrl Pts',(-4.85068927007174,-210.968984254242,
8.40164026752836));
#30731=CARTESIAN_POINT('Ctrl Pts',(1.51270208774127E-11,-210.793984254242,
8.40164026751963));
#30732=CARTESIAN_POINT('Ctrl Pts',(4.85068927010198,-210.618984254242,8.4016402675109));
#30733=CARTESIAN_POINT('Ctrl Pts',(7.27603390513785,-210.443984254242,4.20082013374672));
#30734=CARTESIAN_POINT('Ctrl Pts',(9.70137854017372,-210.268984254242,-1.74665851131138E-11));
#30735=CARTESIAN_POINT('Ctrl Pts',(7.27603390512273,-210.093984254242,-4.20082013377291));
#30736=CARTESIAN_POINT('Ctrl Pts',(4.85068927007174,-209.918984254242,-8.40164026752836));
#30737=CARTESIAN_POINT('Ctrl Pts',(-1.51259919732266E-11,-209.743984254242,
-8.40164026751963));
#30738=CARTESIAN_POINT('Ctrl Pts',(-4.85068927010198,-209.568984254242,
-8.4016402675109));
#30739=CARTESIAN_POINT('Ctrl Pts',(-7.27603390513785,-209.393984254242,
-4.20082013374672));
#30740=CARTESIAN_POINT('Ctrl Pts',(-9.70137854017372,-209.218984254242,
1.74481639267747E-11));
#30741=CARTESIAN_POINT('Ctrl Pts',(-7.27603390512273,-209.043984254242,
4.20082013377291));
#30742=CARTESIAN_POINT('Ctrl Pts',(-4.85068927007174,-208.868984254242,
8.40164026752836));
#30743=CARTESIAN_POINT('Ctrl Pts',(1.51100387578891E-11,-208.693984254242,
8.40164026751963));
#30744=CARTESIAN_POINT('Ctrl Pts',(4.85068927010198,-208.518984254242,8.4016402675109));
#30745=CARTESIAN_POINT('Ctrl Pts',(7.27603390513784,-208.343984254242,4.20082013374673));
#30746=CARTESIAN_POINT('Ctrl Pts',(9.70137854017372,-208.168984254242,-1.74469758505571E-11));
#30747=CARTESIAN_POINT('Ctrl Pts',(7.27603390512273,-207.993984254242,-4.2008201337729));
#30748=CARTESIAN_POINT('Ctrl Pts',(4.85068927007176,-207.818984254242,-8.40164026752835));
#30749=CARTESIAN_POINT('Ctrl Pts',(-1.51239341648544E-11,-207.643984254242,
-8.40164026751963));
#30750=CARTESIAN_POINT('Ctrl Pts',(-4.85068927010198,-207.468984254242,
-8.4016402675109));
#30751=CARTESIAN_POINT('Ctrl Pts',(-7.27603390513784,-207.293984254242,
-4.20082013374673));
#30752=CARTESIAN_POINT('Ctrl Pts',(-9.70137854017372,-207.118984254242,
1.74457877743394E-11));
#30753=CARTESIAN_POINT('Ctrl Pts',(-7.27603390512273,-206.943984254242,
4.20082013377289));
#30754=CARTESIAN_POINT('Ctrl Pts',(-4.85068927007176,-206.768984254242,
8.40164026752835));
#30755=CARTESIAN_POINT('Ctrl Pts',(1.51229052606682E-11,-206.593984254242,
8.40164026751963));
#30756=CARTESIAN_POINT('Ctrl Pts',(4.85068927010198,-206.418984254242,8.4016402675109));
#30757=CARTESIAN_POINT('Ctrl Pts',(7.27603390513784,-206.243984254242,4.20082013374673));
#30758=CARTESIAN_POINT('Ctrl Pts',(9.70137854017372,-206.068984254242,-1.74445996981217E-11));
#30759=CARTESIAN_POINT('Ctrl Pts',(7.27603390512273,-205.893984254242,-4.20082013377289));
#30760=CARTESIAN_POINT('Ctrl Pts',(4.85068927007176,-205.718984254242,-8.40164026752835));
#30761=CARTESIAN_POINT('Ctrl Pts',(-1.51218763564821E-11,-205.543984254242,
-8.40164026751963));
#30762=CARTESIAN_POINT('Ctrl Pts',(-4.85068927010197,-205.368984254242,
-8.4016402675109));
#30763=CARTESIAN_POINT('Ctrl Pts',(-7.27603390513784,-205.193984254242,
-4.20082013374673));
#30764=CARTESIAN_POINT('Ctrl Pts',(-9.70137854017372,-205.018984254242,
1.74434116219041E-11));
#30765=CARTESIAN_POINT('Ctrl Pts',(-7.27603390512274,-204.843984254242,
4.20082013377289));
#30766=CARTESIAN_POINT('Ctrl Pts',(-4.85068927007176,-204.668984254242,
8.40164026752834));
#30767=CARTESIAN_POINT('Ctrl Pts',(1.50909988299932E-11,-204.493984254242,
8.40164026751963));
#30768=CARTESIAN_POINT('Ctrl Pts',(4.85068927010197,-204.318984254242,8.4016402675109));
#30769=CARTESIAN_POINT('Ctrl Pts',(7.27603390513784,-204.143984254242,4.20082013374673));
#30770=CARTESIAN_POINT('Ctrl Pts',(9.70137854017372,-203.968984254242,-1.74422235456864E-11));
#30771=CARTESIAN_POINT('Ctrl Pts',(7.27603390512274,-203.793984254242,-4.20082013377289));
#30772=CARTESIAN_POINT('Ctrl Pts',(4.85068927007176,-203.618984254242,-8.40164026752834));
#30773=CARTESIAN_POINT('Ctrl Pts',(-1.50899699258071E-11,-203.443984254242,
-8.40164026751963));
#30774=CARTESIAN_POINT('Ctrl Pts',(-4.85068927010197,-203.268984254242,
-8.4016402675109));
#30775=CARTESIAN_POINT('Ctrl Pts',(-7.27603390513784,-203.093984254242,
-4.20082013374673));
#30776=CARTESIAN_POINT('Ctrl Pts',(-9.70137854017372,-202.918984254242,
1.74065692492259E-11));
#30777=CARTESIAN_POINT('Ctrl Pts',(-7.27603390512274,-202.743984254242,
4.20082013377289));
#30778=CARTESIAN_POINT('Ctrl Pts',(-4.85068927007173,-202.568984254242,
8.40164026752836));
#30779=CARTESIAN_POINT('Ctrl Pts',(1.5088941021621E-11,-202.393984254242,
8.40164026751963));
#30780=CARTESIAN_POINT('Ctrl Pts',(4.85068927010197,-202.218984254242,8.4016402675109));
#30781=CARTESIAN_POINT('Ctrl Pts',(7.27603390513783,-202.043984254242,4.20082013374676));
#30782=CARTESIAN_POINT('Ctrl Pts',(9.70137854017372,-201.868984254242,-1.74398473932511E-11));
#30783=CARTESIAN_POINT('Ctrl Pts',(7.27603390512275,-201.693984254242,-4.20082013377287));
#30784=CARTESIAN_POINT('Ctrl Pts',(4.85068927007176,-201.518984254242,-8.40164026752834));
#30785=CARTESIAN_POINT('Ctrl Pts',(-1.51177607397376E-11,-201.343984254242,
-8.40164026751963));
#30786=CARTESIAN_POINT('Ctrl Pts',(-4.85068927010194,-201.168984254242,
-8.40164026751092));
#30787=CARTESIAN_POINT('Ctrl Pts',(-7.27603390513784,-200.993984254242,
-4.20082013374673));
#30788=CARTESIAN_POINT('Ctrl Pts',(-9.70137854017372,-200.818984254242,
1.74041930967906E-11));
#30789=CARTESIAN_POINT('Ctrl Pts',(-7.27603390512274,-200.643984254242,
4.20082013377289));
#30790=CARTESIAN_POINT('Ctrl Pts',(-4.85068927007174,-200.468984254242,
8.40164026752836));
#30791=CARTESIAN_POINT('Ctrl Pts',(1.50868832132487E-11,-200.293984254242,
8.40164026751963));
#30792=CARTESIAN_POINT('Ctrl Pts',(4.85068927010197,-200.118984254242,8.4016402675109));
#30793=CARTESIAN_POINT('Ctrl Pts',(7.27603390513783,-199.943984254242,4.20082013374676));
#30794=CARTESIAN_POINT('Ctrl Pts',(9.70137854017372,-199.768984254242,-1.74374712408158E-11));
#30795=CARTESIAN_POINT('Ctrl Pts',(7.27603390512275,-199.593984254242,-4.20082013377286));
#30796=CARTESIAN_POINT('Ctrl Pts',(4.85068927007177,-199.418984254242,-8.40164026752834));
#30797=CARTESIAN_POINT('Ctrl Pts',(-1.51157029313654E-11,-199.243984254242,
-8.40164026751963));
#30798=CARTESIAN_POINT('Ctrl Pts',(-4.85068927010194,-199.068984254242,
-8.40164026751092));
#30799=CARTESIAN_POINT('Ctrl Pts',(-7.27603390513784,-198.893984254242,
-4.20082013374673));
#30800=CARTESIAN_POINT('Ctrl Pts',(-9.70137854017372,-198.718984254242,
1.74018169443553E-11));
#30801=CARTESIAN_POINT('Ctrl Pts',(-7.27603390512274,-198.543984254242,
4.20082013377289));
#30802=CARTESIAN_POINT('Ctrl Pts',(-4.8506892700718,-198.368984254242,8.40164026752832));
#30803=CARTESIAN_POINT('Ctrl Pts',(1.50848254048765E-11,-198.193984254242,
8.40164026751963));
#30804=CARTESIAN_POINT('Ctrl Pts',(4.85068927010197,-198.018984254242,8.4016402675109));
#30805=CARTESIAN_POINT('Ctrl Pts',(7.27603390513782,-197.843984254242,4.20082013374676));
#30806=CARTESIAN_POINT('Ctrl Pts',(9.70137854017372,-197.668984254242,-1.74350950883805E-11));
#30807=CARTESIAN_POINT('Ctrl Pts',(7.27603390512276,-197.493984254242,-4.20082013377286));
#30808=CARTESIAN_POINT('Ctrl Pts',(4.85068927007177,-197.318984254242,-8.40164026752834));
#30809=CARTESIAN_POINT('Ctrl Pts',(-1.51136451229931E-11,-197.143984254242,
-8.40164026751963));
#30810=CARTESIAN_POINT('Ctrl Pts',(-4.85068927010194,-196.968984254242,
-8.40164026751092));
#30811=CARTESIAN_POINT('Ctrl Pts',(-7.27603390513784,-196.793984254242,
-4.20082013374673));
#30812=CARTESIAN_POINT('Ctrl Pts',(-9.70137854017372,-196.618984254242,
1.739944079192E-11));
#30813=CARTESIAN_POINT('Ctrl Pts',(-7.27603390512274,-196.443984254242,
4.20082013377289));
#30814=CARTESIAN_POINT('Ctrl Pts',(-4.8506892700718,-196.268984254242,8.40164026752832));
#30815=CARTESIAN_POINT('Ctrl Pts',(1.50827675965043E-11,-196.093984254242,
8.40164026751963));
#30816=CARTESIAN_POINT('Ctrl Pts',(4.85068927010196,-195.918984254242,8.40164026751091));
#30817=CARTESIAN_POINT('Ctrl Pts',(7.27603390513782,-195.743984254242,4.20082013374676));
#30818=CARTESIAN_POINT('Ctrl Pts',(9.70137854017372,-195.568984254242,-1.74327189359452E-11));
#30819=CARTESIAN_POINT('Ctrl Pts',(7.27603390512276,-195.393984254242,-4.20082013377286));
#30820=CARTESIAN_POINT('Ctrl Pts',(4.85068927007177,-195.218984254242,-8.40164026752834));
#30821=CARTESIAN_POINT('Ctrl Pts',(-1.50518900700154E-11,-195.043984254242,
-8.40164026751963));
#30822=CARTESIAN_POINT('Ctrl Pts',(-4.85068927010193,-194.868984254242,
-8.40164026751092));
#30823=CARTESIAN_POINT('Ctrl Pts',(-7.27603390513784,-194.693984254242,
-4.20082013374674));
#30824=CARTESIAN_POINT('Ctrl Pts',(-9.70137854017372,-194.518984254242,
1.73970646394847E-11));
#30825=CARTESIAN_POINT('Ctrl Pts',(-7.27603390512274,-194.343984254242,
4.20082013377288));
#30826=CARTESIAN_POINT('Ctrl Pts',(-4.8506892700718,-194.168984254242,8.40164026752832));
#30827=CARTESIAN_POINT('Ctrl Pts',(1.5080709788132E-11,-193.993984254242,
8.40164026751963));
#30828=CARTESIAN_POINT('Ctrl Pts',(4.8506892701019,-193.818984254242,8.40164026751094));
#30829=CARTESIAN_POINT('Ctrl Pts',(7.27603390513782,-193.643984254242,4.20082013374676));
#30830=CARTESIAN_POINT('Ctrl Pts',(9.70137854017372,-193.468984254242,-1.74303427835099E-11));
#30831=CARTESIAN_POINT('Ctrl Pts',(7.27603390512276,-193.293984254242,-4.20082013377286));
#30832=CARTESIAN_POINT('Ctrl Pts',(4.85068927007177,-193.118984254242,-8.40164026752834));
#30833=CARTESIAN_POINT('Ctrl Pts',(-1.50498322616431E-11,-192.943984254242,
-8.40164026751963));
#30834=CARTESIAN_POINT('Ctrl Pts',(-4.85068927010193,-192.768984254242,
-8.40164026751093));
#30835=CARTESIAN_POINT('Ctrl Pts',(-7.27603390513784,-192.593984254242,
-4.20082013374674));
#30836=CARTESIAN_POINT('Ctrl Pts',(-9.70137854017372,-192.418984254242,
1.73946884870493E-11));
#30837=CARTESIAN_POINT('Ctrl Pts',(-7.27603390512274,-192.243984254242,
4.20082013377288));
#30838=CARTESIAN_POINT('Ctrl Pts',(-4.85068927007174,-192.068984254242,
8.40164026752836));
#30839=CARTESIAN_POINT('Ctrl Pts',(1.50189547351542E-11,-191.893984254242,
8.40164026751963));
#30840=CARTESIAN_POINT('Ctrl Pts',(4.8506892701019,-191.718984254242,8.40164026751094));
#30841=CARTESIAN_POINT('Ctrl Pts',(7.27603390513782,-191.543984254242,4.20082013374676));
#30842=CARTESIAN_POINT('Ctrl Pts',(9.70137854017372,-191.368984254242,-1.74279666310746E-11));
#30843=CARTESIAN_POINT('Ctrl Pts',(7.27603390512273,-191.193984254242,-4.20082013377291));
#30844=CARTESIAN_POINT('Ctrl Pts',(4.85068927007184,-191.018984254242,-8.4016402675283));
#30845=CARTESIAN_POINT('Ctrl Pts',(-1.50477744532709E-11,-190.843984254242,
-8.40164026751963));
#30846=CARTESIAN_POINT('Ctrl Pts',(-4.85068927010193,-190.668984254242,
-8.40164026751093));
#30847=CARTESIAN_POINT('Ctrl Pts',(-7.27603390513784,-190.493984254242,
-4.20082013374674));
#30848=CARTESIAN_POINT('Ctrl Pts',(-9.70137854017372,-190.318984254242,
1.74612447750998E-11));
#30849=CARTESIAN_POINT('Ctrl Pts',(-7.27603390512277,-190.143984254242,
4.20082013377283));
#30850=CARTESIAN_POINT('Ctrl Pts',(-4.8506892700718,-189.968984254242,8.40164026752832));
#30851=CARTESIAN_POINT('Ctrl Pts',(1.50765941713875E-11,-189.793984254242,
8.40164026751963));
#30852=CARTESIAN_POINT('Ctrl Pts',(4.85068927010196,-189.618984254242,8.40164026751091));
#30853=CARTESIAN_POINT('Ctrl Pts',(7.27603390513779,-189.443984254242,4.20082013374682));
#30854=CARTESIAN_POINT('Ctrl Pts',(9.70137854017372,-189.268984254242,-1.73566580381535E-11));
#30855=CARTESIAN_POINT('Ctrl Pts',(7.27603390512276,-189.093984254242,-4.20082013377285));
#30856=CARTESIAN_POINT('Ctrl Pts',(4.85068927007178,-188.918984254242,-8.40164026752834));
#30857=CARTESIAN_POINT('Ctrl Pts',(-1.51054138895042E-11,-188.743984254242,
-8.40164026751963));
#30858=CARTESIAN_POINT('Ctrl Pts',(-4.85068927010187,-188.568984254242,
-8.40164026751096));
#30859=CARTESIAN_POINT('Ctrl Pts',(-7.27603390513781,-188.393984254242,
-4.20082013374679));
#30860=CARTESIAN_POINT('Ctrl Pts',(-9.70137854017372,-188.218984254242,
1.73899361821787E-11));
#30861=CARTESIAN_POINT('Ctrl Pts',(-7.27603390512274,-188.043984254242,
4.20082013377288));
#30862=CARTESIAN_POINT('Ctrl Pts',(-4.85068927007175,-187.868984254242,
8.40164026752835));
#30863=CARTESIAN_POINT('Ctrl Pts',(1.50148391184097E-11,-187.693984254242,
8.40164026751963));
#30864=CARTESIAN_POINT('Ctrl Pts',(4.8506892701019,-187.518984254242,8.40164026751095));
#30865=CARTESIAN_POINT('Ctrl Pts',(7.27603390513782,-187.343984254242,4.20082013374677));
#30866=CARTESIAN_POINT('Ctrl Pts',(9.70137854017372,-187.168984254242,-1.7423214326204E-11));
#30867=CARTESIAN_POINT('Ctrl Pts',(7.27603390512273,-186.993984254242,-4.2008201337729));
#30868=CARTESIAN_POINT('Ctrl Pts',(4.85068927007184,-186.818984254242,-8.4016402675283));
#30869=CARTESIAN_POINT('Ctrl Pts',(-1.50436588365264E-11,-186.643984254242,
-8.40164026751963));
#30870=CARTESIAN_POINT('Ctrl Pts',(-4.85068927010193,-186.468984254242,
-8.40164026751093));
#30871=CARTESIAN_POINT('Ctrl Pts',(-7.27603390513783,-186.293984254242,
-4.20082013374674));
#30872=CARTESIAN_POINT('Ctrl Pts',(-9.70137854017372,-186.118984254242,
1.73186275892576E-11));
#30873=CARTESIAN_POINT('Ctrl Pts',(-7.27603390512277,-185.943984254242,
4.20082013377283));
#30874=CARTESIAN_POINT('Ctrl Pts',(-4.85068927007181,-185.768984254242,
8.40164026752832));
#30875=CARTESIAN_POINT('Ctrl Pts',(1.5072478554643E-11,-185.593984254242,
8.40164026751963));
#30876=CARTESIAN_POINT('Ctrl Pts',(4.85068927010196,-185.418984254242,8.40164026751091));
#30877=CARTESIAN_POINT('Ctrl Pts',(7.27603390513779,-185.243984254242,4.20082013374682));
#30878=CARTESIAN_POINT('Ctrl Pts',(9.70137854017372,-185.068984254242,-1.73519057332829E-11));
#30879=CARTESIAN_POINT('Ctrl Pts',(7.27603390512276,-184.893984254242,-4.20082013377285));
#30880=CARTESIAN_POINT('Ctrl Pts',(4.85068927007178,-184.718984254242,-8.40164026752833));
#30881=CARTESIAN_POINT('Ctrl Pts',(-1.51012982727597E-11,-184.543984254242,
-8.40164026751963));
#30882=CARTESIAN_POINT('Ctrl Pts',(-4.85068927010186,-184.368984254242,
-8.40164026751097));
#30883=CARTESIAN_POINT('Ctrl Pts',(-7.2760339051378,-184.193984254242,-4.2008201337468));
#30884=CARTESIAN_POINT('Ctrl Pts',(-9.70137854017372,-184.018984254242,
1.73851838773081E-11));
#30885=CARTESIAN_POINT('Ctrl Pts',(-7.27603390512275,-183.843984254242,
4.20082013377288));
#30886=CARTESIAN_POINT('Ctrl Pts',(-4.85068927007175,-183.668984254242,
8.40164026752835));
#30887=CARTESIAN_POINT('Ctrl Pts',(1.50107235016652E-11,-183.493984254242,
8.40164026751963));
#30888=CARTESIAN_POINT('Ctrl Pts',(4.85068927010189,-183.318984254242,8.40164026751095));
#30889=CARTESIAN_POINT('Ctrl Pts',(7.27603390513782,-183.143984254242,4.20082013374677));
#30890=CARTESIAN_POINT('Ctrl Pts',(9.70137854017372,-182.968984254242,-1.74184620213334E-11));
#30891=CARTESIAN_POINT('Ctrl Pts',(7.27603390512279,-182.793984254242,-4.2008201337728));
#30892=CARTESIAN_POINT('Ctrl Pts',(4.85068927007184,-182.618984254242,-8.4016402675283));
#30893=CARTESIAN_POINT('Ctrl Pts',(-1.50395432197819E-11,-182.443984254242,
-8.40164026751963));
#30894=CARTESIAN_POINT('Ctrl Pts',(-4.85068927010192,-182.268984254242,
-8.40164026751093));
#30895=CARTESIAN_POINT('Ctrl Pts',(-7.27603390513783,-182.093984254242,
-4.20082013374675));
#30896=CARTESIAN_POINT('Ctrl Pts',(-9.70137854017372,-181.918984254242,
1.7313875284387E-11));
#30897=CARTESIAN_POINT('Ctrl Pts',(-7.27603390512278,-181.743984254242,
4.20082013377282));
#30898=CARTESIAN_POINT('Ctrl Pts',(-4.85068927007181,-181.568984254242,
8.40164026752832));
#30899=CARTESIAN_POINT('Ctrl Pts',(1.50683629378986E-11,-181.393984254242,
8.40164026751963));
#30900=CARTESIAN_POINT('Ctrl Pts',(4.85068927010195,-181.218984254242,8.40164026751092));
#30901=CARTESIAN_POINT('Ctrl Pts',(7.27603390513779,-181.043984254242,4.20082013374683));
#30902=CARTESIAN_POINT('Ctrl Pts',(9.70137854017372,-180.868984254242,-1.73471534284123E-11));
#30903=CARTESIAN_POINT('Ctrl Pts',(7.27603390512276,-180.693984254242,-4.20082013377285));
#30904=CARTESIAN_POINT('Ctrl Pts',(4.85068927007178,-180.518984254242,-8.40164026752833));
#30905=CARTESIAN_POINT('Ctrl Pts',(-1.50971826560152E-11,-180.343984254242,
-8.40164026751963));
#30906=CARTESIAN_POINT('Ctrl Pts',(-4.85068927010186,-180.168984254242,
-8.40164026751097));
#30907=CARTESIAN_POINT('Ctrl Pts',(-7.2760339051378,-179.993984254242,-4.2008201337468));
#30908=CARTESIAN_POINT('Ctrl Pts',(-9.70137854017372,-179.818984254242,
1.73804315724375E-11));
#30909=CARTESIAN_POINT('Ctrl Pts',(-7.27603390512275,-179.643984254242,
4.20082013377287));
#30910=CARTESIAN_POINT('Ctrl Pts',(-4.85068927007188,-179.468984254242,
8.40164026752828));
#30911=CARTESIAN_POINT('Ctrl Pts',(1.50066078849208E-11,-179.293984254242,
8.40164026751963));
#30912=CARTESIAN_POINT('Ctrl Pts',(4.85068927010189,-179.118984254242,8.40164026751095));
#30913=CARTESIAN_POINT('Ctrl Pts',(7.27603390513782,-178.943984254242,4.20082013374678));
#30914=CARTESIAN_POINT('Ctrl Pts',(9.70137854017372,-178.768984254242,-1.74137097164627E-11));
#30915=CARTESIAN_POINT('Ctrl Pts',(7.27603390512279,-178.593984254242,-4.20082013377279));
#30916=CARTESIAN_POINT('Ctrl Pts',(4.85068927007185,-178.418984254242,-8.4016402675283));
#30917=CARTESIAN_POINT('Ctrl Pts',(-1.50354276030374E-11,-178.243984254242,
-8.40164026751963));
#30918=CARTESIAN_POINT('Ctrl Pts',(-4.85068927010192,-178.068984254242,
-8.40164026751093));
#30919=CARTESIAN_POINT('Ctrl Pts',(-7.27603390513783,-177.893984254242,
-4.20082013374675));
#30920=CARTESIAN_POINT('Ctrl Pts',(-9.70137854017372,-177.718984254242,
1.73091229795164E-11));
#30921=CARTESIAN_POINT('Ctrl Pts',(-7.27603390512278,-177.543984254242,
4.20082013377282));
#30922=CARTESIAN_POINT('Ctrl Pts',(-4.85068927007182,-177.368984254242,
8.40164026752831));
#30923=CARTESIAN_POINT('Ctrl Pts',(1.50642473211541E-11,-177.193984254242,
8.40164026751963));
#30924=CARTESIAN_POINT('Ctrl Pts',(4.85068927010183,-177.018984254242,8.40164026751099));
#30925=CARTESIAN_POINT('Ctrl Pts',(7.27603390513778,-176.843984254242,4.20082013374683));
#30926=CARTESIAN_POINT('Ctrl Pts',(9.70137854017372,-176.668984254242,-1.73424011235416E-11));
#30927=CARTESIAN_POINT('Ctrl Pts',(7.27603390512277,-176.493984254242,-4.20082013377284));
#30928=CARTESIAN_POINT('Ctrl Pts',(4.85068927007179,-176.318984254242,-8.40164026752833));
#30929=CARTESIAN_POINT('Ctrl Pts',(-1.49736725500596E-11,-176.143984254242,
-8.40164026751963));
#30930=CARTESIAN_POINT('Ctrl Pts',(-4.85068927010185,-175.968984254242,
-8.40164026751097));
#30931=CARTESIAN_POINT('Ctrl Pts',(-7.2760339051378,-175.793984254242,-4.2008201337468));
#30932=CARTESIAN_POINT('Ctrl Pts',(-9.70137854017372,-175.618984254242,
1.73756792675669E-11));
#30933=CARTESIAN_POINT('Ctrl Pts',(-7.27603390512275,-175.443984254242,
4.20082013377287));
#30934=CARTESIAN_POINT('Ctrl Pts',(-4.85068927007188,-175.268984254242,
8.40164026752828));
#30935=CARTESIAN_POINT('Ctrl Pts',(1.50024922681763E-11,-175.093984254242,
8.40164026751963));
#30936=CARTESIAN_POINT('Ctrl Pts',(4.85068927010188,-174.918984254242,8.40164026751095));
#30937=CARTESIAN_POINT('Ctrl Pts',(7.27603390513781,-174.743984254242,4.20082013374678));
#30938=CARTESIAN_POINT('Ctrl Pts',(9.70137854017372,-174.568984254242,-1.74089574115921E-11));
#30939=CARTESIAN_POINT('Ctrl Pts',(7.2760339051228,-174.393984254242,-4.20082013377279));
#30940=CARTESIAN_POINT('Ctrl Pts',(4.85068927007185,-174.218984254242,-8.4016402675283));
#30941=CARTESIAN_POINT('Ctrl Pts',(-1.50313119862929E-11,-174.043984254242,
-8.40164026751963));
#30942=CARTESIAN_POINT('Ctrl Pts',(-4.85068927010191,-173.868984254242,
-8.40164026751094));
#30943=CARTESIAN_POINT('Ctrl Pts',(-7.27603390513777,-173.693984254242,
-4.20082013374686));
#30944=CARTESIAN_POINT('Ctrl Pts',(-9.70137854017372,-173.518984254242,
1.73043706746458E-11));
#30945=CARTESIAN_POINT('Ctrl Pts',(-7.27603390512278,-173.343984254242,
4.20082013377282));
#30946=CARTESIAN_POINT('Ctrl Pts',(-4.85068927007182,-173.168984254242,
8.40164026752831));
#30947=CARTESIAN_POINT('Ctrl Pts',(1.50601317044096E-11,-172.993984254242,
8.40164026751963));
#30948=CARTESIAN_POINT('Ctrl Pts',(4.85068927010182,-172.818984254242,8.40164026751099));
#30949=CARTESIAN_POINT('Ctrl Pts',(7.27603390513778,-172.643984254242,4.20082013374683));
#30950=CARTESIAN_POINT('Ctrl Pts',(9.70137854017372,-172.468984254242,-1.7337648818671E-11));
#30951=CARTESIAN_POINT('Ctrl Pts',(7.27603390512277,-172.293984254242,-4.20082013377284));
#30952=CARTESIAN_POINT('Ctrl Pts',(4.85068927007179,-172.118984254242,-8.40164026752833));
#30953=CARTESIAN_POINT('Ctrl Pts',(-1.49695569333151E-11,-171.943984254242,
-8.40164026751963));
#30954=CARTESIAN_POINT('Ctrl Pts',(-4.85068927010185,-171.768984254242,
-8.40164026751097));
#30955=CARTESIAN_POINT('Ctrl Pts',(-7.2760339051378,-171.593984254242,-4.20082013374681));
#30956=CARTESIAN_POINT('Ctrl Pts',(-9.70137854017372,-171.418984254242,
1.73709269626963E-11));
#30957=CARTESIAN_POINT('Ctrl Pts',(-7.27603390512275,-171.243984254242,
4.20082013377287));
#30958=CARTESIAN_POINT('Ctrl Pts',(-4.85068927007176,-171.068984254242,
8.40164026752834));
#30959=CARTESIAN_POINT('Ctrl Pts',(1.49983766514318E-11,-170.893984254242,
8.40164026751963));
#30960=CARTESIAN_POINT('Ctrl Pts',(4.85068927010176,-170.718984254242,8.40164026751102));
#30961=CARTESIAN_POINT('Ctrl Pts',(7.27603390513781,-170.543984254242,4.20082013374678));
#30962=CARTESIAN_POINT('Ctrl Pts',(9.70137854017372,-170.368984254242,-1.72663402257499E-11));
#30963=CARTESIAN_POINT('Ctrl Pts',(7.27603390512274,-170.193984254242,-4.20082013377289));
#30964=CARTESIAN_POINT('Ctrl Pts',(4.85068927007186,-170.018984254242,-8.40164026752829));
#30965=CARTESIAN_POINT('Ctrl Pts',(-1.49078018803373E-11,-169.843984254242,
-8.40164026751963));
#30966=CARTESIAN_POINT('Ctrl Pts',(-4.85068927010191,-169.668984254242,
-8.40164026751094));
#30967=CARTESIAN_POINT('Ctrl Pts',(-7.27603390513777,-169.493984254242,
-4.20082013374686));
#30968=CARTESIAN_POINT('Ctrl Pts',(-9.70137854017372,-169.318984254242,
1.74374832507468E-11));
#30969=CARTESIAN_POINT('Ctrl Pts',(-7.27603390512278,-169.143984254242,
4.20082013377281));
#30970=CARTESIAN_POINT('Ctrl Pts',(-4.85068927007195,-168.968984254242,
8.40164026752824));
#30971=CARTESIAN_POINT('Ctrl Pts',(1.50560160876651E-11,-168.793984254242,
8.40164026751963));
#30972=CARTESIAN_POINT('Ctrl Pts',(4.85068927010182,-168.618984254242,8.40164026751099));
#30973=CARTESIAN_POINT('Ctrl Pts',(7.27603390513784,-168.443984254242,4.20082013374673));
#30974=CARTESIAN_POINT('Ctrl Pts',(9.70137854017372,-168.268984254242,-1.73328965138004E-11));
#30975=CARTESIAN_POINT('Ctrl Pts',(7.27603390512283,-168.093984254242,-4.20082013377273));
#30976=CARTESIAN_POINT('Ctrl Pts',(4.8506892700718,-167.918984254242,-8.40164026752832));
#30977=CARTESIAN_POINT('Ctrl Pts',(-1.49654413165707E-11,-167.743984254242,
-8.40164026751963));
#30978=CARTESIAN_POINT('Ctrl Pts',(-4.85068927010197,-167.568984254242,
-8.4016402675109));
#30979=CARTESIAN_POINT('Ctrl Pts',(-7.27603390513779,-167.393984254242,
-4.20082013374681));
#30980=CARTESIAN_POINT('Ctrl Pts',(-9.70137854017372,-167.218984254242,
1.72283097768541E-11));
#30981=CARTESIAN_POINT('Ctrl Pts',(-7.27603390512276,-167.043984254242,
4.20082013377286));
#30982=CARTESIAN_POINT('Ctrl Pts',(-4.85068927007189,-166.868984254242,
8.40164026752827));
#30983=CARTESIAN_POINT('Ctrl Pts',(1.51136555238984E-11,-166.693984254242,
8.40164026751963));
#30984=CARTESIAN_POINT('Ctrl Pts',(4.85068927010188,-166.518984254242,8.40164026751096));
#30985=CARTESIAN_POINT('Ctrl Pts',(7.27603390513775,-166.343984254242,4.20082013374689));
#30986=CARTESIAN_POINT('Ctrl Pts',(9.70137854017372,-166.168984254242,-1.73994528018509E-11));
#30987=CARTESIAN_POINT('Ctrl Pts',(7.2760339051228,-165.993984254242,-4.20082013377278));
#30988=CARTESIAN_POINT('Ctrl Pts',(4.85068927007198,-165.818984254242,-8.40164026752822));
#30989=CARTESIAN_POINT('Ctrl Pts',(-1.5023080752804E-11,-165.643984254242,
-8.40164026751963));
#30990=CARTESIAN_POINT('Ctrl Pts',(-4.85068927010179,-165.468984254242,
-8.40164026751101));
#30991=CARTESIAN_POINT('Ctrl Pts',(-7.27603390513782,-165.293984254242,
-4.20082013374676));
#30992=CARTESIAN_POINT('Ctrl Pts',(-9.70137854017372,-165.118984254242,
1.72948660649045E-11));
#30993=CARTESIAN_POINT('Ctrl Pts',(-7.27603390512285,-164.943984254242,
4.20082013377271));
#30994=CARTESIAN_POINT('Ctrl Pts',(-4.85068927007183,-164.768984254242,
8.40164026752831));
#30995=CARTESIAN_POINT('Ctrl Pts',(1.49325059817095E-11,-164.593984254242,
8.40164026751963));
#30996=CARTESIAN_POINT('Ctrl Pts',(4.85068927010193,-164.418984254242,8.40164026751092));
#30997=CARTESIAN_POINT('Ctrl Pts',(7.27603390513778,-164.243984254242,4.20082013374684));
#30998=CARTESIAN_POINT('Ctrl Pts',(9.70137854017372,-164.068984254242,-1.71902793279582E-11));
#30999=CARTESIAN_POINT('Ctrl Pts',(7.27603390512277,-163.893984254242,-4.20082013377283));
#31000=CARTESIAN_POINT('Ctrl Pts',(4.85068927007192,-163.718984254242,-8.40164026752825));
#31001=CARTESIAN_POINT('Ctrl Pts',(-1.50807201890373E-11,-163.543984254242,
-8.40164026751963));
#31002=CARTESIAN_POINT('Ctrl Pts',(-4.85068927010184,-163.368984254242,
-8.40164026751098));
#31003=CARTESIAN_POINT('Ctrl Pts',(-7.27603390513773,-163.193984254242,
-4.20082013374692));
#31004=CARTESIAN_POINT('Ctrl Pts',(-9.70137854017372,-163.018984254242,
1.7361422352955E-11));
#31005=CARTESIAN_POINT('Ctrl Pts',(-7.27603390512282,-162.843984254242,
4.20082013377275));
#31006=CARTESIAN_POINT('Ctrl Pts',(-4.85068927007177,-162.668984254242,
8.40164026752834));
#31007=CARTESIAN_POINT('Ctrl Pts',(1.49901454179428E-11,-162.493984254242,
8.40164026751963));
#31008=CARTESIAN_POINT('Ctrl Pts',(4.85068927010175,-162.318984254242,8.40164026751103));
#31009=CARTESIAN_POINT('Ctrl Pts',(7.27603390513781,-162.143984254242,4.20082013374679));
#31010=CARTESIAN_POINT('Ctrl Pts',(9.70137854017372,-161.968984254242,-1.72568356160087E-11));
#31011=CARTESIAN_POINT('Ctrl Pts',(7.27603390512274,-161.793984254242,-4.20082013377288));
#31012=CARTESIAN_POINT('Ctrl Pts',(4.85068927007186,-161.618984254242,-8.40164026752829));
#31013=CARTESIAN_POINT('Ctrl Pts',(-1.48995706468484E-11,-161.443984254242,
-8.40164026751963));
#31014=CARTESIAN_POINT('Ctrl Pts',(-4.8506892701019,-161.268984254242,-8.40164026751094));
#31015=CARTESIAN_POINT('Ctrl Pts',(-7.27603390513776,-161.093984254242,
-4.20082013374687));
#31016=CARTESIAN_POINT('Ctrl Pts',(-9.70137854017372,-160.918984254242,
1.74279786410055E-11));
#31017=CARTESIAN_POINT('Ctrl Pts',(-7.27603390512279,-160.743984254242,
4.2008201337728));
#31018=CARTESIAN_POINT('Ctrl Pts',(-4.85068927007195,-160.568984254242,
8.40164026752823));
#31019=CARTESIAN_POINT('Ctrl Pts',(1.50477848541761E-11,-160.393984254242,
8.40164026751963));
#31020=CARTESIAN_POINT('Ctrl Pts',(4.85068927010181,-160.218984254242,8.401640267511));
#31021=CARTESIAN_POINT('Ctrl Pts',(7.27603390513784,-160.043984254242,4.20082013374674));
#31022=CARTESIAN_POINT('Ctrl Pts',(9.70137854017372,-159.868984254242,-1.73233919040592E-11));
#31023=CARTESIAN_POINT('Ctrl Pts',(7.27603390512283,-159.693984254242,-4.20082013377273));
#31024=CARTESIAN_POINT('Ctrl Pts',(4.8506892700718,-159.518984254242,-8.40164026752832));
#31025=CARTESIAN_POINT('Ctrl Pts',(-1.49572100830817E-11,-159.343984254242,
-8.40164026751963));
#31026=CARTESIAN_POINT('Ctrl Pts',(-4.85068927010172,-159.168984254242,
-8.40164026751105));
#31027=CARTESIAN_POINT('Ctrl Pts',(-7.27603390513779,-158.993984254242,
-4.20082013374682));
#31028=CARTESIAN_POINT('Ctrl Pts',(-9.70137854017372,-158.818984254242,
1.72188051671128E-11));
#31029=CARTESIAN_POINT('Ctrl Pts',(-7.27603390512276,-158.643984254242,
4.20082013377285));
#31030=CARTESIAN_POINT('Ctrl Pts',(-4.8506892700719,-158.468984254242,8.40164026752827));
#31031=CARTESIAN_POINT('Ctrl Pts',(1.48666353119872E-11,-158.293984254242,
8.40164026751963));
#31032=CARTESIAN_POINT('Ctrl Pts',(4.85068927010187,-158.118984254242,8.40164026751096));
#31033=CARTESIAN_POINT('Ctrl Pts',(7.27603390513774,-157.943984254242,4.2008201337469));
#31034=CARTESIAN_POINT('Ctrl Pts',(9.70137854017372,-157.768984254242,-1.73899481921097E-11));
#31035=CARTESIAN_POINT('Ctrl Pts',(7.27603390512281,-157.593984254242,-4.20082013377278));
#31036=CARTESIAN_POINT('Ctrl Pts',(4.85068927007199,-157.418984254242,-8.40164026752822));
#31037=CARTESIAN_POINT('Ctrl Pts',(-1.5014849519315E-11,-157.243984254242,
-8.40164026751963));
#31038=CARTESIAN_POINT('Ctrl Pts',(-4.85068927010178,-157.068984254242,
-8.40164026751101));
#31039=CARTESIAN_POINT('Ctrl Pts',(-7.27603390513782,-156.893984254242,
-4.20082013374677));
#31040=CARTESIAN_POINT('Ctrl Pts',(-9.70137854017372,-156.718984254242,
1.72853614551633E-11));
#31041=CARTESIAN_POINT('Ctrl Pts',(-7.27603390512285,-156.543984254242,
4.2008201337727));
#31042=CARTESIAN_POINT('Ctrl Pts',(-4.85068927007184,-156.368984254242,
8.4016402675283));
#31043=CARTESIAN_POINT('Ctrl Pts',(1.49242747482206E-11,-156.193984254242,
8.40164026751963));
#31044=CARTESIAN_POINT('Ctrl Pts',(4.85068927010193,-156.018984254242,8.40164026751093));
#31045=CARTESIAN_POINT('Ctrl Pts',(7.27603390513778,-155.843984254242,4.20082013374685));
#31046=CARTESIAN_POINT('Ctrl Pts',(9.70137854017372,-155.668984254242,-1.7180774718217E-11));
#31047=CARTESIAN_POINT('Ctrl Pts',(7.27603390512277,-155.493984254242,-4.20082013377283));
#31048=CARTESIAN_POINT('Ctrl Pts',(4.85068927007193,-155.318984254242,-8.40164026752825));
#31049=CARTESIAN_POINT('Ctrl Pts',(-1.50724889555483E-11,-155.143984254242,
-8.40164026751963));
#31050=CARTESIAN_POINT('Ctrl Pts',(-4.85068927010184,-154.968984254242,
-8.40164026751098));
#31051=CARTESIAN_POINT('Ctrl Pts',(-7.27603390513773,-154.793984254242,
-4.20082013374692));
#31052=CARTESIAN_POINT('Ctrl Pts',(-9.70137854017372,-154.618984254242,
1.73519177432138E-11));
#31053=CARTESIAN_POINT('Ctrl Pts',(-7.27603390512282,-154.443984254242,
4.20082013377275));
#31054=CARTESIAN_POINT('Ctrl Pts',(-4.85068927007178,-154.268984254242,
8.40164026752833));
#31055=CARTESIAN_POINT('Ctrl Pts',(1.49819141844539E-11,-154.093984254242,
8.40164026751963));
#31056=CARTESIAN_POINT('Ctrl Pts',(4.85068927010175,-153.918984254242,8.40164026751103));
#31057=CARTESIAN_POINT('Ctrl Pts',(7.2760339051378,-153.743984254242,4.2008201337468));
#31058=CARTESIAN_POINT('Ctrl Pts',(9.70137854017372,-153.568984254242,-1.72473310062675E-11));
#31059=CARTESIAN_POINT('Ctrl Pts',(7.27603390512275,-153.393984254242,-4.20082013377288));
#31060=CARTESIAN_POINT('Ctrl Pts',(4.85068927007187,-153.218984254242,-8.40164026752828));
#31061=CARTESIAN_POINT('Ctrl Pts',(-1.48913394133594E-11,-153.043984254242,
-8.40164026751963));
#31062=CARTESIAN_POINT('Ctrl Pts',(-4.85068927010189,-152.868984254242,
-8.40164026751095));
#31063=CARTESIAN_POINT('Ctrl Pts',(-7.27603390513776,-152.693984254242,
-4.20082013374688));
#31064=CARTESIAN_POINT('Ctrl Pts',(-9.70137854017372,-152.518984254242,
1.71427442693211E-11));
#31065=CARTESIAN_POINT('Ctrl Pts',(-7.27603390512279,-152.343984254242,
4.2008201337728));
#31066=CARTESIAN_POINT('Ctrl Pts',(-4.85068927007196,-152.168984254242,
8.40164026752823));
#31067=CARTESIAN_POINT('Ctrl Pts',(1.50395536206872E-11,-151.993984254242,
8.40164026751963));
#31068=CARTESIAN_POINT('Ctrl Pts',(4.8506892701018,-151.818984254242,8.401640267511));
#31069=CARTESIAN_POINT('Ctrl Pts',(7.27603390513771,-151.643984254242,4.20082013374695));
#31070=CARTESIAN_POINT('Ctrl Pts',(9.70137854017372,-151.468984254242,-1.73138872943179E-11));
#31071=CARTESIAN_POINT('Ctrl Pts',(7.27603390512284,-151.293984254242,-4.20082013377272));
#31072=CARTESIAN_POINT('Ctrl Pts',(4.85068927007181,-151.118984254242,-8.40164026752832));
#31073=CARTESIAN_POINT('Ctrl Pts',(-1.49489788495927E-11,-150.943984254242,
-8.40164026751963));
#31074=CARTESIAN_POINT('Ctrl Pts',(-4.85068927010171,-150.768984254242,
-8.40164026751105));
#31075=CARTESIAN_POINT('Ctrl Pts',(-7.27603390513779,-150.593984254242,
-4.20082013374683));
#31076=CARTESIAN_POINT('Ctrl Pts',(-9.70137854017372,-150.418984254242,
1.72093005573716E-11));
#31077=CARTESIAN_POINT('Ctrl Pts',(-7.27603390512276,-150.243984254242,
4.20082013377285));
#31078=CARTESIAN_POINT('Ctrl Pts',(-4.8506892700719,-150.068984254242,8.40164026752826));
#31079=CARTESIAN_POINT('Ctrl Pts',(1.48584040784983E-11,-149.893984254242,
8.40164026751963));
#31080=CARTESIAN_POINT('Ctrl Pts',(4.85068927010186,-149.718984254242,8.40164026751097));
#31081=CARTESIAN_POINT('Ctrl Pts',(7.27603390513774,-149.543984254242,4.2008201337469));
#31082=CARTESIAN_POINT('Ctrl Pts',(9.70137854017372,-149.368984254242,-1.73804435823684E-11));
#31083=CARTESIAN_POINT('Ctrl Pts',(7.27603390512281,-149.193984254242,-4.20082013377277));
#31084=CARTESIAN_POINT('Ctrl Pts',(4.85068927007199,-149.018984254242,-8.40164026752821));
#31085=CARTESIAN_POINT('Ctrl Pts',(-1.5006618285826E-11,-148.843984254242,
-8.40164026751963));
#31086=CARTESIAN_POINT('Ctrl Pts',(-4.85068927010177,-148.668984254242,
-8.40164026751102));
#31087=CARTESIAN_POINT('Ctrl Pts',(-7.27603390513782,-148.493984254242,
-4.20082013374678));
#31088=CARTESIAN_POINT('Ctrl Pts',(-9.70137854017372,-148.318984254242,
1.72758568454221E-11));
#31089=CARTESIAN_POINT('Ctrl Pts',(-7.27603390512285,-148.143984254242,
4.20082013377269));
#31090=CARTESIAN_POINT('Ctrl Pts',(-4.85068927007185,-147.968984254242,
8.4016402675283));
#31091=CARTESIAN_POINT('Ctrl Pts',(1.49160435147316E-11,-147.793984254242,
8.40164026751963));
#31092=CARTESIAN_POINT('Ctrl Pts',(4.85068927010192,-147.618984254242,8.40164026751093));
#31093=CARTESIAN_POINT('Ctrl Pts',(7.27603390513777,-147.443984254242,4.20082013374685));
#31094=CARTESIAN_POINT('Ctrl Pts',(9.70137854017372,-147.268984254242,-1.71712701084757E-11));
#31095=CARTESIAN_POINT('Ctrl Pts',(7.27603390512278,-147.093984254242,-4.20082013377282));
#31096=CARTESIAN_POINT('Ctrl Pts',(4.85068927007194,-146.918984254242,-8.40164026752825));
#31097=CARTESIAN_POINT('Ctrl Pts',(-1.50642577220594E-11,-146.743984254242,
-8.40164026751963));
#31098=CARTESIAN_POINT('Ctrl Pts',(-4.85068927010183,-146.568984254242,
-8.40164026751099));
#31099=CARTESIAN_POINT('Ctrl Pts',(-7.27603390513773,-146.393984254242,
-4.20082013374693));
#31100=CARTESIAN_POINT('Ctrl Pts',(-9.70137854017372,-146.218984254242,
1.73424131334726E-11));
#31101=CARTESIAN_POINT('Ctrl Pts',(-7.27603390512282,-146.043984254242,
4.20082013377274));
#31102=CARTESIAN_POINT('Ctrl Pts',(-4.85068927007203,-145.868984254242,
8.40164026752819));
#31103=CARTESIAN_POINT('Ctrl Pts',(1.49736829509649E-11,-145.693984254242,
8.40164026751963));
#31104=CARTESIAN_POINT('Ctrl Pts',(4.85068927010174,-145.518984254242,8.40164026751104));
#31105=CARTESIAN_POINT('Ctrl Pts',(7.2760339051378,-145.343984254242,4.2008201337468));
#31106=CARTESIAN_POINT('Ctrl Pts',(9.70137854017372,-145.168984254242,-1.72378263965262E-11));
#31107=CARTESIAN_POINT('Ctrl Pts',(7.27603390512287,-144.993984254242,-4.20082013377266));
#31108=CARTESIAN_POINT('Ctrl Pts',(4.85068927007188,-144.818984254242,-8.40164026752828));
#31109=CARTESIAN_POINT('Ctrl Pts',(-1.48831081798705E-11,-144.643984254242,
-8.40164026751963));
#31110=CARTESIAN_POINT('Ctrl Pts',(-4.85068927010188,-144.468984254242,
-8.40164026751095));
#31111=CARTESIAN_POINT('Ctrl Pts',(-7.27603390513775,-144.293984254242,
-4.20082013374688));
#31112=CARTESIAN_POINT('Ctrl Pts',(-9.70137854017372,-144.118984254242,
1.71332396595799E-11));
#31113=CARTESIAN_POINT('Ctrl Pts',(-7.2760339051228,-143.943984254242,4.20082013377279));
#31114=CARTESIAN_POINT('Ctrl Pts',(-4.85068927007197,-143.768984254242,
8.40164026752823));
#31115=CARTESIAN_POINT('Ctrl Pts',(1.50313223871982E-11,-143.593984254242,
8.40164026751963));
#31116=CARTESIAN_POINT('Ctrl Pts',(4.85068927010179,-143.418984254242,8.401640267511));
#31117=CARTESIAN_POINT('Ctrl Pts',(7.27603390513771,-143.243984254242,4.20082013374696));
#31118=CARTESIAN_POINT('Ctrl Pts',(9.70137854017372,-143.068984254242,-1.73043826845767E-11));
#31119=CARTESIAN_POINT('Ctrl Pts',(7.27603390512284,-142.893984254242,-4.20082013377271));
#31120=CARTESIAN_POINT('Ctrl Pts',(4.85068927007182,-142.718984254242,-8.40164026752831));
#31121=CARTESIAN_POINT('Ctrl Pts',(-1.49407476161038E-11,-142.543984254242,
-8.40164026751963));
#31122=CARTESIAN_POINT('Ctrl Pts',(-4.8506892701017,-142.368984254242,-8.40164026751106));
#31123=CARTESIAN_POINT('Ctrl Pts',(-7.27603390513778,-142.193984254242,
-4.20082013374683));
#31124=CARTESIAN_POINT('Ctrl Pts',(-9.70137854017372,-142.018984254242,
1.71997959476304E-11));
#31125=CARTESIAN_POINT('Ctrl Pts',(-7.27603390512277,-141.843984254242,
4.20082013377284));
#31126=CARTESIAN_POINT('Ctrl Pts',(-4.85068927007191,-141.668984254242,
8.40164026752826));
#31127=CARTESIAN_POINT('Ctrl Pts',(1.48501728450093E-11,-141.493984254242,
8.40164026751963));
#31128=CARTESIAN_POINT('Ctrl Pts',(4.85068927010185,-141.318984254242,8.40164026751097));
#31129=CARTESIAN_POINT('Ctrl Pts',(7.27603390513774,-141.143984254242,4.20082013374691));
#31130=CARTESIAN_POINT('Ctrl Pts',(9.70137854017372,-140.968984254242,-1.73709389726272E-11));
#31131=CARTESIAN_POINT('Ctrl Pts',(7.27603390512281,-140.793984254242,-4.20082013377276));
#31132=CARTESIAN_POINT('Ctrl Pts',(4.850689270072,-140.618984254242,-8.40164026752821));
#31133=CARTESIAN_POINT('Ctrl Pts',(-1.49983870523371E-11,-140.443984254242,
-8.40164026751963));
#31134=CARTESIAN_POINT('Ctrl Pts',(-4.85068927010176,-140.268984254242,
-8.40164026751102));
#31135=CARTESIAN_POINT('Ctrl Pts',(-7.27603390513769,-140.093984254242,
-4.20082013374699));
#31136=CARTESIAN_POINT('Ctrl Pts',(-9.70137854017372,-139.918984254242,
1.72663522356809E-11));
#31137=CARTESIAN_POINT('Ctrl Pts',(-7.27603390512286,-139.743984254242,
4.20082013377268));
#31138=CARTESIAN_POINT('Ctrl Pts',(-4.85068927007186,-139.568984254242,
8.40164026752829));
#31139=CARTESIAN_POINT('Ctrl Pts',(1.49078122812426E-11,-139.393984254242,
8.40164026751963));
#31140=CARTESIAN_POINT('Ctrl Pts',(4.85068927010167,-139.218984254242,8.40164026751108));
#31141=CARTESIAN_POINT('Ctrl Pts',(7.27603390513777,-139.043984254242,4.20082013374686));
#31142=CARTESIAN_POINT('Ctrl Pts',(9.70137854017372,-138.868984254242,-1.71617654987345E-11));
#31143=CARTESIAN_POINT('Ctrl Pts',(7.27603390512278,-138.693984254242,-4.20082013377281));
#31144=CARTESIAN_POINT('Ctrl Pts',(4.85068927007195,-138.518984254242,-8.40164026752824));
#31145=CARTESIAN_POINT('Ctrl Pts',(-1.48172375101482E-11,-138.343984254242,
-8.40164026751963));
#31146=CARTESIAN_POINT('Ctrl Pts',(-4.85068927010182,-138.168984254242,
-8.40164026751099));
#31147=CARTESIAN_POINT('Ctrl Pts',(-7.27603390513772,-137.993984254242,
-4.20082013374694));
#31148=CARTESIAN_POINT('Ctrl Pts',(-9.70137854017372,-137.818984254242,
1.73329085237313E-11));
#31149=CARTESIAN_POINT('Ctrl Pts',(-7.27603390512283,-137.643984254242,
4.20082013377273));
#31150=CARTESIAN_POINT('Ctrl Pts',(-4.85068927007204,-137.468984254242,
8.40164026752819));
#31151=CARTESIAN_POINT('Ctrl Pts',(1.49654517174759E-11,-137.293984254242,
8.40164026751963));
#31152=CARTESIAN_POINT('Ctrl Pts',(4.85068927010173,-137.118984254242,8.40164026751104));
#31153=CARTESIAN_POINT('Ctrl Pts',(7.27603390513779,-136.943984254242,4.20082013374681));
#31154=CARTESIAN_POINT('Ctrl Pts',(9.70137854017372,-136.768984254242,-1.7228321786785E-11));
#31155=CARTESIAN_POINT('Ctrl Pts',(7.27603390512287,-136.593984254242,-4.20082013377265));
#31156=CARTESIAN_POINT('Ctrl Pts',(4.85068927007189,-136.418984254242,-8.40164026752827));
#31157=CARTESIAN_POINT('Ctrl Pts',(-1.48748769463815E-11,-136.243984254242,
-8.40164026751963));
#31158=CARTESIAN_POINT('Ctrl Pts',(-4.85068927010188,-136.068984254242,
-8.40164026751096));
#31159=CARTESIAN_POINT('Ctrl Pts',(-7.27603390513775,-135.893984254242,
-4.20082013374689));
#31160=CARTESIAN_POINT('Ctrl Pts',(-9.70137854017372,-135.718984254242,
1.71237350498386E-11));
#31161=CARTESIAN_POINT('Ctrl Pts',(-7.2760339051228,-135.543984254242,4.20082013377278));
#31162=CARTESIAN_POINT('Ctrl Pts',(-4.85068927007198,-135.368984254242,
8.40164026752822));
#31163=CARTESIAN_POINT('Ctrl Pts',(1.50230911537093E-11,-135.193984254242,
8.40164026751963));
#31164=CARTESIAN_POINT('Ctrl Pts',(4.85068927010179,-135.018984254242,8.40164026751101));
#31165=CARTESIAN_POINT('Ctrl Pts',(7.2760339051377,-134.843984254242,4.20082013374697));
#31166=CARTESIAN_POINT('Ctrl Pts',(9.70137854017372,-134.668984254242,-1.72948780748355E-11));
#31167=CARTESIAN_POINT('Ctrl Pts',(7.27603390512285,-134.493984254242,-4.20082013377271));
#31168=CARTESIAN_POINT('Ctrl Pts',(4.85068927007183,-134.318984254242,-8.40164026752831));
#31169=CARTESIAN_POINT('Ctrl Pts',(-1.49325163826148E-11,-134.143984254242,
-8.40164026751963));
#31170=CARTESIAN_POINT('Ctrl Pts',(-4.85068927010169,-133.968984254242,
-8.40164026751106));
#31171=CARTESIAN_POINT('Ctrl Pts',(-7.27603390513778,-133.793984254242,
-4.20082013374684));
#31172=CARTESIAN_POINT('Ctrl Pts',(-9.70137854017372,-133.618984254242,
1.71902913378891E-11));
#31173=CARTESIAN_POINT('Ctrl Pts',(-7.27603390512289,-133.443984254242,
4.20082013377263));
#31174=CARTESIAN_POINT('Ctrl Pts',(-4.85068927007192,-133.268984254242,
8.40164026752825));
#31175=CARTESIAN_POINT('Ctrl Pts',(1.48419416115203E-11,-133.093984254242,
8.40164026751963));
#31176=CARTESIAN_POINT('Ctrl Pts',(4.85068927010184,-132.918984254242,8.40164026751098));
#31177=CARTESIAN_POINT('Ctrl Pts',(7.27603390513773,-132.743984254242,4.20082013374692));
#31178=CARTESIAN_POINT('Ctrl Pts',(9.70137854017372,-132.568984254242,-1.70857046009428E-11));
#31179=CARTESIAN_POINT('Ctrl Pts',(7.27603390512282,-132.393984254242,-4.20082013377275));
#31180=CARTESIAN_POINT('Ctrl Pts',(4.85068927007201,-132.218984254242,-8.4016402675282));
#31181=CARTESIAN_POINT('Ctrl Pts',(-1.49901558188481E-11,-132.043984254242,
-8.40164026751963));
#31182=CARTESIAN_POINT('Ctrl Pts',(-4.85068927010175,-131.868984254242,
-8.40164026751103));
#31183=CARTESIAN_POINT('Ctrl Pts',(-7.27603390513769,-131.693984254242,
-4.200820133747));
#31184=CARTESIAN_POINT('Ctrl Pts',(-9.70137854017372,-131.518984254242,
1.72568476259396E-11));
#31185=CARTESIAN_POINT('Ctrl Pts',(-7.27603390512286,-131.343984254242,
4.20082013377267));
#31186=CARTESIAN_POINT('Ctrl Pts',(-4.85068927007186,-131.168984254242,
8.40164026752829));
#31187=CARTESIAN_POINT('Ctrl Pts',(1.48995810477537E-11,-130.993984254242,
8.40164026751963));
#31188=CARTESIAN_POINT('Ctrl Pts',(4.85068927010166,-130.818984254242,8.40164026751108));
#31189=CARTESIAN_POINT('Ctrl Pts',(7.27603390513776,-130.643984254242,4.20082013374687));
#31190=CARTESIAN_POINT('Ctrl Pts',(9.70137854017372,-130.468984254242,-1.71522608889933E-11));
#31191=CARTESIAN_POINT('Ctrl Pts',(7.27603390512279,-130.293984254242,-4.2008201337728));
#31192=CARTESIAN_POINT('Ctrl Pts',(4.85068927007195,-130.118984254242,-8.40164026752823));
#31193=CARTESIAN_POINT('Ctrl Pts',(-1.48090062766592E-11,-129.943984254242,
-8.40164026751963));
#31194=CARTESIAN_POINT('Ctrl Pts',(-4.85068927010181,-129.768984254242,
-8.401640267511));
#31195=CARTESIAN_POINT('Ctrl Pts',(-7.27603390513772,-129.593984254242,
-4.20082013374695));
#31196=CARTESIAN_POINT('Ctrl Pts',(-9.70137854017372,-129.418984254242,
1.73234039139901E-11));
#31197=CARTESIAN_POINT('Ctrl Pts',(-7.27603390512283,-129.243984254242,
4.20082013377273));
#31198=CARTESIAN_POINT('Ctrl Pts',(-4.85068927007204,-129.068984254242,
8.40164026752818));
#31199=CARTESIAN_POINT('Ctrl Pts',(1.4957220483987E-11,-128.893984254242,
8.40164026751963));
#31200=CARTESIAN_POINT('Ctrl Pts',(4.85068927010172,-128.718984254242,8.40164026751105));
#31201=CARTESIAN_POINT('Ctrl Pts',(7.27603390513779,-128.543984254242,4.20082013374682));
#31202=CARTESIAN_POINT('Ctrl Pts',(9.70137854017372,-128.368984254242,-1.72188171770438E-11));
#31203=CARTESIAN_POINT('Ctrl Pts',(7.27603390512276,-128.193984254242,-4.20082013377285));
#31204=CARTESIAN_POINT('Ctrl Pts',(4.85068927007213,-128.018984254242,-8.40164026752813));
#31205=CARTESIAN_POINT('Ctrl Pts',(-1.48666457128925E-11,-127.843984254242,
-8.40164026751963));
#31206=CARTESIAN_POINT('Ctrl Pts',(-4.85068927010187,-127.668984254242,
-8.40164026751096));
#31207=CARTESIAN_POINT('Ctrl Pts',(-7.27603390513763,-127.493984254242,
-4.2008201337471));
#31208=CARTESIAN_POINT('Ctrl Pts',(-9.70137854017372,-127.318984254242,
1.71142304400974E-11));
#31209=CARTESIAN_POINT('Ctrl Pts',(-7.27603390512281,-127.143984254242,
4.20082013377278));
#31210=CARTESIAN_POINT('Ctrl Pts',(-4.85068927007175,-126.968984254242,
8.40164026752835));
#31211=CARTESIAN_POINT('Ctrl Pts',(1.47760709417981E-11,-126.793984254242,
8.40164026751963));
#31212=CARTESIAN_POINT('Ctrl Pts',(4.85068927010178,-126.618984254242,8.40164026751101));
#31213=CARTESIAN_POINT('Ctrl Pts',(7.27603390513782,-126.443984254242,4.20082013374677));
#31214=CARTESIAN_POINT('Ctrl Pts',(9.70137854017372,-126.268984254242,-1.70096437031511E-11));
#31215=CARTESIAN_POINT('Ctrl Pts',(7.27603390512285,-126.093984254242,-4.2008201337727));
#31216=CARTESIAN_POINT('Ctrl Pts',(4.85068927007184,-125.918984254242,-8.4016402675283));
#31217=CARTESIAN_POINT('Ctrl Pts',(-1.46854961707036E-11,-125.743984254242,
-8.40164026751963));
#31218=CARTESIAN_POINT('Ctrl Pts',(-4.85068927010169,-125.568984254242,
-8.40164026751107));
#31219=CARTESIAN_POINT('Ctrl Pts',(-7.27603390513778,-125.393984254242,
-4.20082013374685));
#31220=CARTESIAN_POINT('Ctrl Pts',(-9.70137854017372,-125.218984254242,
1.74565164900911E-11));
#31221=CARTESIAN_POINT('Ctrl Pts',(-7.27603390512289,-125.043984254242,
4.20082013377262));
#31222=CARTESIAN_POINT('Ctrl Pts',(-4.85068927007193,-124.868984254242,
8.40164026752825));
#31223=CARTESIAN_POINT('Ctrl Pts',(1.50724993564536E-11,-124.693984254242,
8.40164026751963));
#31224=CARTESIAN_POINT('Ctrl Pts',(4.8506892701016,-124.518984254242,8.40164026751112));
#31225=CARTESIAN_POINT('Ctrl Pts',(7.27603390513773,-124.343984254242,4.20082013374692));
#31226=CARTESIAN_POINT('Ctrl Pts',(9.70137854017372,-124.168984254242,-1.73519297531447E-11));
#31227=CARTESIAN_POINT('Ctrl Pts',(7.27603390512294,-123.993984254242,-4.20082013377254));
#31228=CARTESIAN_POINT('Ctrl Pts',(4.85068927007202,-123.818984254242,-8.4016402675282));
#31229=CARTESIAN_POINT('Ctrl Pts',(-1.49819245853592E-11,-123.643984254242,
-8.40164026751963));
#31230=CARTESIAN_POINT('Ctrl Pts',(-4.85068927010151,-123.468984254242,
-8.40164026751117));
#31231=CARTESIAN_POINT('Ctrl Pts',(-7.27603390513768,-123.293984254242,
-4.200820133747));
#31232=CARTESIAN_POINT('Ctrl Pts',(-9.70137854017372,-123.118984254242,
1.72473430161984E-11));
#31233=CARTESIAN_POINT('Ctrl Pts',(-7.27603390512275,-122.943984254242,
4.20082013377288));
#31234=CARTESIAN_POINT('Ctrl Pts',(-4.85068927007211,-122.768984254242,
8.40164026752814));
#31235=CARTESIAN_POINT('Ctrl Pts',(1.48913498142647E-11,-122.593984254242,
8.40164026751963));
#31236=CARTESIAN_POINT('Ctrl Pts',(4.85068927010189,-122.418984254242,8.40164026751095));
#31237=CARTESIAN_POINT('Ctrl Pts',(7.27603390513764,-122.243984254242,4.20082013374708));
#31238=CARTESIAN_POINT('Ctrl Pts',(9.70137854017372,-122.068984254242,-1.7142756279252E-11));
#31239=CARTESIAN_POINT('Ctrl Pts',(7.27603390512279,-121.893984254242,-4.2008201337728));
#31240=CARTESIAN_POINT('Ctrl Pts',(4.8506892700722,-121.718984254242,-8.40164026752809));
#31241=CARTESIAN_POINT('Ctrl Pts',(-1.48007750431702E-11,-121.543984254242,
-8.40164026751963));
#31242=CARTESIAN_POINT('Ctrl Pts',(-4.8506892701018,-121.368984254242,-8.401640267511));
#31243=CARTESIAN_POINT('Ctrl Pts',(-7.27603390513783,-121.193984254242,
-4.20082013374675));
#31244=CARTESIAN_POINT('Ctrl Pts',(-9.70137854017372,-121.018984254242,
1.70381695423057E-11));
#31245=CARTESIAN_POINT('Ctrl Pts',(-7.27603390512284,-120.843984254242,
4.20082013377272));
#31246=CARTESIAN_POINT('Ctrl Pts',(-4.85068927007181,-120.668984254242,
8.40164026752832));
#31247=CARTESIAN_POINT('Ctrl Pts',(1.47102002720758E-11,-120.493984254242,
8.40164026751963));
#31248=CARTESIAN_POINT('Ctrl Pts',(4.85068927010171,-120.318984254242,8.40164026751105));
#31249=CARTESIAN_POINT('Ctrl Pts',(7.27603390513779,-120.143984254242,4.20082013374683));
#31250=CARTESIAN_POINT('Ctrl Pts',(9.70137854017372,-119.968984254242,-1.69335828053594E-11));
#31251=CARTESIAN_POINT('Ctrl Pts',(7.27603390512288,-119.793984254242,-4.20082013377264));
#31252=CARTESIAN_POINT('Ctrl Pts',(4.8506892700719,-119.618984254242,-8.40164026752826));
#31253=CARTESIAN_POINT('Ctrl Pts',(-1.50972034578258E-11,-119.443984254242,
-8.40164026751963));
#31254=CARTESIAN_POINT('Ctrl Pts',(-4.85068927010162,-119.268984254242,
-8.40164026751111));
#31255=CARTESIAN_POINT('Ctrl Pts',(-7.27603390513774,-119.093984254242,
-4.2008201337469));
#31256=CARTESIAN_POINT('Ctrl Pts',(-9.70137854017372,-118.918984254242,
1.73804555922994E-11));
#31257=CARTESIAN_POINT('Ctrl Pts',(-7.27603390512293,-118.743984254242,
4.20082013377256));
#31258=CARTESIAN_POINT('Ctrl Pts',(-4.85068927007199,-118.568984254242,
8.40164026752821));
#31259=CARTESIAN_POINT('Ctrl Pts',(1.50066286867313E-11,-118.393984254242,
8.40164026751963));
#31260=CARTESIAN_POINT('Ctrl Pts',(4.85068927010153,-118.218984254242,8.40164026751116));
#31261=CARTESIAN_POINT('Ctrl Pts',(7.2760339051377,-118.043984254242,4.20082013374698));
#31262=CARTESIAN_POINT('Ctrl Pts',(9.70137854017372,-117.868984254242,-1.7275868855353E-11));
#31263=CARTESIAN_POINT('Ctrl Pts',(7.27603390512297,-117.693984254242,-4.20082013377248));
#31264=CARTESIAN_POINT('Ctrl Pts',(4.85068927007208,-117.518984254242,-8.40164026752816));
#31265=CARTESIAN_POINT('Ctrl Pts',(-1.49160539156369E-11,-117.343984254242,
-8.40164026751963));
#31266=CARTESIAN_POINT('Ctrl Pts',(-4.85068927010192,-117.168984254242,
-8.40164026751093));
#31267=CARTESIAN_POINT('Ctrl Pts',(-7.27603390513765,-116.993984254242,
-4.20082013374706));
#31268=CARTESIAN_POINT('Ctrl Pts',(-9.70137854017372,-116.818984254242,
1.71712821184067E-11));
#31269=CARTESIAN_POINT('Ctrl Pts',(-7.27603390512278,-116.643984254242,
4.20082013377282));
#31270=CARTESIAN_POINT('Ctrl Pts',(-4.85068927007218,-116.468984254242,
8.40164026752811));
#31271=CARTESIAN_POINT('Ctrl Pts',(1.48254791445424E-11,-116.293984254242,
8.40164026751963));
#31272=CARTESIAN_POINT('Ctrl Pts',(4.85068927010183,-116.118984254242,8.40164026751099));
#31273=CARTESIAN_POINT('Ctrl Pts',(7.27603390513761,-115.943984254242,4.20082013374714));
#31274=CARTESIAN_POINT('Ctrl Pts',(9.70137854017372,-115.768984254242,-1.70666953814603E-11));
#31275=CARTESIAN_POINT('Ctrl Pts',(7.27603390512282,-115.593984254242,-4.20082013377274));
#31276=CARTESIAN_POINT('Ctrl Pts',(4.85068927007179,-115.418984254242,-8.40164026752833));
#31277=CARTESIAN_POINT('Ctrl Pts',(-1.4734904373448E-11,-115.243984254242,
-8.40164026751963));
#31278=CARTESIAN_POINT('Ctrl Pts',(-4.85068927010174,-115.068984254242,
-8.40164026751104));
#31279=CARTESIAN_POINT('Ctrl Pts',(-7.2760339051378,-114.893984254242,-4.2008201337468));
#31280=CARTESIAN_POINT('Ctrl Pts',(-9.70137854017372,-114.718984254242,
1.6962108644514E-11));
#31281=CARTESIAN_POINT('Ctrl Pts',(-7.27603390512287,-114.543984254242,
4.20082013377266));
#31282=CARTESIAN_POINT('Ctrl Pts',(-4.85068927007188,-114.368984254242,
8.40164026752828));
#31283=CARTESIAN_POINT('Ctrl Pts',(1.46443296023535E-11,-114.193984254242,
8.40164026751963));
#31284=CARTESIAN_POINT('Ctrl Pts',(4.85068927010165,-114.018984254242,8.40164026751109));
#31285=CARTESIAN_POINT('Ctrl Pts',(7.27603390513775,-113.843984254242,4.20082013374688));
#31286=CARTESIAN_POINT('Ctrl Pts',(9.70137854017372,-113.668984254242,-1.7408981431454E-11));
#31287=CARTESIAN_POINT('Ctrl Pts',(7.27603390512292,-113.493984254242,-4.20082013377258));
#31288=CARTESIAN_POINT('Ctrl Pts',(4.85068927007197,-113.318984254242,-8.40164026752823));
#31289=CARTESIAN_POINT('Ctrl Pts',(-1.50313327881035E-11,-113.143984254242,
-8.40164026751963));
#31290=CARTESIAN_POINT('Ctrl Pts',(-4.85068927010155,-112.968984254242,
-8.40164026751114));
#31291=CARTESIAN_POINT('Ctrl Pts',(-7.27603390513771,-112.793984254242,
-4.20082013374696));
#31292=CARTESIAN_POINT('Ctrl Pts',(-9.70137854017372,-112.618984254242,
1.73043946945076E-11));
#31293=CARTESIAN_POINT('Ctrl Pts',(-7.27603390512296,-112.443984254242,
4.2008201337725));
#31294=CARTESIAN_POINT('Ctrl Pts',(-4.85068927007206,-112.268984254242,
8.40164026752817));
#31295=CARTESIAN_POINT('Ctrl Pts',(1.49407580170091E-11,-112.093984254242,
8.40164026751963));
#31296=CARTESIAN_POINT('Ctrl Pts',(4.85068927010194,-111.918984254242,8.40164026751092));
#31297=CARTESIAN_POINT('Ctrl Pts',(7.27603390513766,-111.743984254242,4.20082013374704));
#31298=CARTESIAN_POINT('Ctrl Pts',(9.70137854017372,-111.568984254242,-1.71998079575613E-11));
#31299=CARTESIAN_POINT('Ctrl Pts',(7.27603390512277,-111.393984254242,-4.20082013377284));
#31300=CARTESIAN_POINT('Ctrl Pts',(4.85068927007215,-111.218984254242,-8.40164026752812));
#31301=CARTESIAN_POINT('Ctrl Pts',(-1.48501832459146E-11,-111.043984254242,
-8.40164026751963));
#31302=CARTESIAN_POINT('Ctrl Pts',(-4.85068927010185,-110.868984254242,
-8.40164026751097));
#31303=CARTESIAN_POINT('Ctrl Pts',(-7.27603390513762,-110.693984254242,
-4.20082013374712));
#31304=CARTESIAN_POINT('Ctrl Pts',(-9.70137854017372,-110.518984254242,
1.7095221220615E-11));
#31305=CARTESIAN_POINT('Ctrl Pts',(-7.27603390512281,-110.343984254242,
4.20082013377276));
#31306=CARTESIAN_POINT('Ctrl Pts',(-4.85068927007224,-110.168984254242,
8.40164026752807));
#31307=CARTESIAN_POINT('Ctrl Pts',(1.47596084748201E-11,-109.993984254242,
8.40164026751963));
#31308=CARTESIAN_POINT('Ctrl Pts',(4.85068927010176,-109.818984254242,8.40164026751102));
#31309=CARTESIAN_POINT('Ctrl Pts',(7.27603390513781,-109.643984254242,4.20082013374678));
#31310=CARTESIAN_POINT('Ctrl Pts',(9.70137854017372,-109.468984254242,-1.69906344836686E-11));
#31311=CARTESIAN_POINT('Ctrl Pts',(7.27603390512286,-109.293984254242,-4.20082013377268));
#31312=CARTESIAN_POINT('Ctrl Pts',(4.85068927007186,-109.118984254242,-8.40164026752829));
#31313=CARTESIAN_POINT('Ctrl Pts',(-1.46690337037257E-11,-108.943984254242,
-8.40164026751963));
#31314=CARTESIAN_POINT('Ctrl Pts',(-4.85068927010167,-108.768984254242,
-8.40164026751108));
#31315=CARTESIAN_POINT('Ctrl Pts',(-7.27603390513777,-108.593984254242,
-4.20082013374686));
#31316=CARTESIAN_POINT('Ctrl Pts',(-9.70137854017372,-108.418984254242,
1.68860477467223E-11));
#31317=CARTESIAN_POINT('Ctrl Pts',(-7.2760339051229,-108.243984254242,4.2008201337726));
#31318=CARTESIAN_POINT('Ctrl Pts',(-4.85068927007195,-108.068984254242,
8.40164026752824));
#31319=CARTESIAN_POINT('Ctrl Pts',(1.50560368894757E-11,-107.893984254242,
8.40164026751963));
#31320=CARTESIAN_POINT('Ctrl Pts',(4.85068927010158,-107.718984254242,8.40164026751113));
#31321=CARTESIAN_POINT('Ctrl Pts',(7.27603390513772,-107.543984254242,4.20082013374694));
#31322=CARTESIAN_POINT('Ctrl Pts',(9.70137854017372,-107.368984254242,-1.73329205336623E-11));
#31323=CARTESIAN_POINT('Ctrl Pts',(7.27603390512295,-107.193984254242,-4.20082013377253));
#31324=CARTESIAN_POINT('Ctrl Pts',(4.85068927007204,-107.018984254242,-8.40164026752819));
#31325=CARTESIAN_POINT('Ctrl Pts',(-1.49654621183812E-11,-106.843984254242,
-8.40164026751963));
#31326=CARTESIAN_POINT('Ctrl Pts',(-4.85068927010149,-106.668984254242,
-8.40164026751118));
#31327=CARTESIAN_POINT('Ctrl Pts',(-7.27603390513768,-106.493984254242,
-4.20082013374702));
#31328=CARTESIAN_POINT('Ctrl Pts',(-9.70137854017372,-106.318984254242,
1.72283337967159E-11));
#31329=CARTESIAN_POINT('Ctrl Pts',(-7.27603390512276,-106.143984254242,
4.20082013377286));
#31330=CARTESIAN_POINT('Ctrl Pts',(-4.85068927007213,-105.968984254242,
8.40164026752814));
#31331=CARTESIAN_POINT('Ctrl Pts',(1.48748873472868E-11,-105.793984254242,
8.40164026751963));
#31332=CARTESIAN_POINT('Ctrl Pts',(4.85068927010188,-105.618984254242,8.40164026751096));
#31333=CARTESIAN_POINT('Ctrl Pts',(7.27603390513763,-105.443984254242,4.2008201337471));
#31334=CARTESIAN_POINT('Ctrl Pts',(9.70137854017372,-105.268984254242,-1.71237470597696E-11));
#31335=CARTESIAN_POINT('Ctrl Pts',(7.2760339051228,-105.093984254242,-4.20082013377278));
#31336=CARTESIAN_POINT('Ctrl Pts',(4.85068927007222,-104.918984254242,-8.40164026752808));
#31337=CARTESIAN_POINT('Ctrl Pts',(-1.47843125761923E-11,-104.743984254242,
-8.40164026751963));
#31338=CARTESIAN_POINT('Ctrl Pts',(-4.85068927010179,-104.568984254242,
-8.40164026751101));
#31339=CARTESIAN_POINT('Ctrl Pts',(-7.27603390513758,-104.393984254242,
-4.20082013374717));
#31340=CARTESIAN_POINT('Ctrl Pts',(-9.70137854017372,-104.218984254242,
1.70191603228232E-11));
#31341=CARTESIAN_POINT('Ctrl Pts',(-7.27603390512285,-104.043984254242,
4.20082013377271));
#31342=CARTESIAN_POINT('Ctrl Pts',(-4.85068927007183,-103.868984254242,
8.40164026752831));
#31343=CARTESIAN_POINT('Ctrl Pts',(1.46937378050979E-11,-103.693984254242,
8.40164026751963));
#31344=CARTESIAN_POINT('Ctrl Pts',(4.85068927010169,-103.518984254242,8.40164026751106));
#31345=CARTESIAN_POINT('Ctrl Pts',(7.27603390513778,-103.343984254242,4.20082013374684));
#31346=CARTESIAN_POINT('Ctrl Pts',(9.70137854017372,-103.168984254242,-1.69145735858769E-11));
#31347=CARTESIAN_POINT('Ctrl Pts',(7.27603390512289,-102.993984254242,-4.20082013377263));
#31348=CARTESIAN_POINT('Ctrl Pts',(4.85068927007192,-102.818984254242,-8.40164026752825));
#31349=CARTESIAN_POINT('Ctrl Pts',(-1.46031630340034E-11,-102.643984254242,
-8.40164026751963));
#31350=CARTESIAN_POINT('Ctrl Pts',(-4.8506892701016,-102.468984254242,-8.40164026751111));
#31351=CARTESIAN_POINT('Ctrl Pts',(-7.27603390513773,-102.293984254242,
-4.20082013374692));
#31352=CARTESIAN_POINT('Ctrl Pts',(-9.70137854017372,-102.118984254242,
1.73614463728169E-11));
#31353=CARTESIAN_POINT('Ctrl Pts',(-7.27603390512294,-101.943984254242,
4.20082013377255));
#31354=CARTESIAN_POINT('Ctrl Pts',(-4.85068927007201,-101.768984254242,
8.4016402675282));
#31355=CARTESIAN_POINT('Ctrl Pts',(1.49901662197534E-11,-101.593984254242,
8.40164026751963));
#31356=CARTESIAN_POINT('Ctrl Pts',(4.85068927010151,-101.418984254242,8.40164026751117));
#31357=CARTESIAN_POINT('Ctrl Pts',(7.27603390513769,-101.243984254242,4.200820133747));
#31358=CARTESIAN_POINT('Ctrl Pts',(9.70137854017372,-101.068984254242,-1.72568596358705E-11));
#31359=CARTESIAN_POINT('Ctrl Pts',(7.27603390512298,-100.893984254242,-4.20082013377247));
#31360=CARTESIAN_POINT('Ctrl Pts',(4.8506892700721,-100.718984254242,-8.40164026752815));
#31361=CARTESIAN_POINT('Ctrl Pts',(-1.48995914486589E-11,-100.543984254242,
-8.40164026751963));
#31362=CARTESIAN_POINT('Ctrl Pts',(-4.8506892701019,-100.368984254242,-8.40164026751094));
#31363=CARTESIAN_POINT('Ctrl Pts',(-7.27603390513764,-100.193984254242,
-4.20082013374707));
#31364=CARTESIAN_POINT('Ctrl Pts',(-9.70137854017372,-100.018984254242,
1.71522728989242E-11));
#31365=CARTESIAN_POINT('Ctrl Pts',(-7.27603390512279,-99.8439842542419,
4.2008201337728));
#31366=CARTESIAN_POINT('Ctrl Pts',(-4.85068927007219,-99.6689842542419,
8.4016402675281));
#31367=CARTESIAN_POINT('Ctrl Pts',(1.48090166775645E-11,-99.4939842542419,
8.40164026751963));
#31368=CARTESIAN_POINT('Ctrl Pts',(4.85068927010181,-99.3189842542419,8.401640267511));
#31369=CARTESIAN_POINT('Ctrl Pts',(7.2760339051376,-99.1439842542419,4.20082013374715));
#31370=CARTESIAN_POINT('Ctrl Pts',(9.70137854017372,-98.9689842542419,-1.70476861619779E-11));
#31371=CARTESIAN_POINT('Ctrl Pts',(7.27603390512283,-98.7939842542419,-4.20082013377273));
#31372=CARTESIAN_POINT('Ctrl Pts',(4.85068927007228,-98.6189842542419,-8.40164026752804));
#31373=CARTESIAN_POINT('Ctrl Pts',(-1.471844190647E-11,-98.4439842542419,
-8.40164026751963));
#31374=CARTESIAN_POINT('Ctrl Pts',(-4.85068927010172,-98.2689842542419,
-8.40164026751105));
#31375=CARTESIAN_POINT('Ctrl Pts',(-7.27603390513779,-98.0939842542419,
-4.20082013374682));
#31376=CARTESIAN_POINT('Ctrl Pts',(-9.70137854017372,-97.9189842542419,
1.69430994250315E-11));
#31377=CARTESIAN_POINT('Ctrl Pts',(-7.27603390512288,-97.7439842542419,
4.20082013377265));
#31378=CARTESIAN_POINT('Ctrl Pts',(-4.8506892700719,-97.5689842542419,8.40164026752827));
#31379=CARTESIAN_POINT('Ctrl Pts',(1.46278671353756E-11,-97.3939842542419,
8.40164026751963));
#31380=CARTESIAN_POINT('Ctrl Pts',(4.85068927010163,-97.2189842542419,8.4016402675111));
#31381=CARTESIAN_POINT('Ctrl Pts',(7.27603390513774,-97.0439842542419,4.2008201337469));
#31382=CARTESIAN_POINT('Ctrl Pts',(9.70137854017372,-96.8689842542419,-1.68385126880852E-11));
#31383=CARTESIAN_POINT('Ctrl Pts',(7.27603390512292,-96.6939842542419,-4.20082013377257));
#31384=CARTESIAN_POINT('Ctrl Pts',(4.85068927007199,-96.5189842542419,-8.40164026752822));
#31385=CARTESIAN_POINT('Ctrl Pts',(-1.50148703211256E-11,-96.3439842542419,
-8.40164026751963));
#31386=CARTESIAN_POINT('Ctrl Pts',(-4.85068927010154,-96.1689842542419,
-8.40164026751115));
#31387=CARTESIAN_POINT('Ctrl Pts',(-7.2760339051377,-95.9939842542419,-4.20082013374698));
#31388=CARTESIAN_POINT('Ctrl Pts',(-9.70137854017372,-95.8189842542419,
1.72853854750252E-11));
#31389=CARTESIAN_POINT('Ctrl Pts',(-7.27603390512297,-95.6439842542419,
4.20082013377249));
#31390=CARTESIAN_POINT('Ctrl Pts',(-4.85068927007208,-95.4689842542419,
8.40164026752816));
#31391=CARTESIAN_POINT('Ctrl Pts',(1.49242955500311E-11,-95.2939842542419,
8.40164026751963));
#31392=CARTESIAN_POINT('Ctrl Pts',(4.85068927010145,-95.1189842542419,8.40164026751121));
#31393=CARTESIAN_POINT('Ctrl Pts',(7.27603390513766,-94.9439842542419,4.20082013374705));
#31394=CARTESIAN_POINT('Ctrl Pts',(9.70137854017372,-94.7689842542419,-1.71807987380788E-11));
#31395=CARTESIAN_POINT('Ctrl Pts',(7.27603390512277,-94.5939842542419,-4.20082013377283));
#31396=CARTESIAN_POINT('Ctrl Pts',(4.85068927007217,-94.4189842542419,-8.40164026752811));
#31397=CARTESIAN_POINT('Ctrl Pts',(-1.48337207789367E-11,-94.2439842542419,
-8.40164026751963));
#31398=CARTESIAN_POINT('Ctrl Pts',(-4.85068927010184,-94.0689842542419,
-8.40164026751098));
#31399=CARTESIAN_POINT('Ctrl Pts',(-7.27603390513761,-93.8939842542419,
-4.20082013374713));
#31400=CARTESIAN_POINT('Ctrl Pts',(-9.70137854017372,-93.7189842542419,
1.70762120011325E-11));
#31401=CARTESIAN_POINT('Ctrl Pts',(-7.27603390512282,-93.5439842542419,
4.20082013377275));
#31402=CARTESIAN_POINT('Ctrl Pts',(-4.85068927007226,-93.3689842542419,
8.40164026752806));
#31403=CARTESIAN_POINT('Ctrl Pts',(1.47431460078422E-11,-93.1939842542419,
8.40164026751963));
#31404=CARTESIAN_POINT('Ctrl Pts',(4.85068927010175,-93.0189842542419,8.40164026751103));
#31405=CARTESIAN_POINT('Ctrl Pts',(7.2760339051378,-92.8439842542419,4.2008201337468));
#31406=CARTESIAN_POINT('Ctrl Pts',(9.70137854017372,-92.6689842542419,-1.69716252641861E-11));
#31407=CARTESIAN_POINT('Ctrl Pts',(7.27603390512287,-92.4939842542419,-4.20082013377267));
#31408=CARTESIAN_POINT('Ctrl Pts',(4.85068927007187,-92.3189842542419,-8.40164026752828));
#31409=CARTESIAN_POINT('Ctrl Pts',(-1.46525712367478E-11,-92.1439842542419,
-8.40164026751963));
#31410=CARTESIAN_POINT('Ctrl Pts',(-4.85068927010165,-91.9689842542419,
-8.40164026751109));
#31411=CARTESIAN_POINT('Ctrl Pts',(-7.27603390513776,-91.7939842542419,
-4.20082013374688));
#31412=CARTESIAN_POINT('Ctrl Pts',(-9.70137854017372,-91.6189842542419,
1.68670385272398E-11));
#31413=CARTESIAN_POINT('Ctrl Pts',(-7.27603390512291,-91.4439842542419,
4.20082013377259));
#31414=CARTESIAN_POINT('Ctrl Pts',(-4.85068927007196,-91.2689842542419,
8.40164026752823));
#31415=CARTESIAN_POINT('Ctrl Pts',(1.45619964656533E-11,-91.0939842542419,
8.40164026751963));
#31416=CARTESIAN_POINT('Ctrl Pts',(4.85068927010157,-90.9189842542419,8.40164026751114));
#31417=CARTESIAN_POINT('Ctrl Pts',(7.27603390513771,-90.7439842542419,4.20082013374695));
#31418=CARTESIAN_POINT('Ctrl Pts',(9.70137854017372,-90.5689842542419,-1.73139113141798E-11));
#31419=CARTESIAN_POINT('Ctrl Pts',(7.27603390512296,-90.3939842542419,-4.20082013377251));
#31420=CARTESIAN_POINT('Ctrl Pts',(4.85068927007205,-90.2189842542419,-8.40164026752818));
#31421=CARTESIAN_POINT('Ctrl Pts',(-1.49489996514033E-11,-90.0439842542419,
-8.40164026751963));
#31422=CARTESIAN_POINT('Ctrl Pts',(-4.85068927010147,-89.8689842542419,
-8.40164026751119));
#31423=CARTESIAN_POINT('Ctrl Pts',(-7.27603390513767,-89.6939842542419,
-4.20082013374703));
#31424=CARTESIAN_POINT('Ctrl Pts',(-9.70137854017372,-89.5189842542419,
1.72093245772335E-11));
#31425=CARTESIAN_POINT('Ctrl Pts',(-7.276033905123,-89.3439842542419,4.20082013377243));
#31426=CARTESIAN_POINT('Ctrl Pts',(-4.85068927007214,-89.1689842542419,
8.40164026752813));
#31427=CARTESIAN_POINT('Ctrl Pts',(1.48584248803088E-11,-88.9939842542419,
8.40164026751963));
#31428=CARTESIAN_POINT('Ctrl Pts',(4.85068927010186,-88.8189842542419,8.40164026751097));
#31429=CARTESIAN_POINT('Ctrl Pts',(7.27603390513762,-88.6439842542419,4.20082013374711));
#31430=CARTESIAN_POINT('Ctrl Pts',(9.70137854017372,-88.4689842542419,-1.71047378402871E-11));
#31431=CARTESIAN_POINT('Ctrl Pts',(7.27603390512281,-88.2939842542419,-4.20082013377277));
#31432=CARTESIAN_POINT('Ctrl Pts',(4.85068927007223,-88.1189842542419,-8.40164026752807));
#31433=CARTESIAN_POINT('Ctrl Pts',(-1.47678501092144E-11,-87.9439842542419,
-8.40164026751963));
#31434=CARTESIAN_POINT('Ctrl Pts',(-4.85068927010177,-87.7689842542419,
-8.40164026751102));
#31435=CARTESIAN_POINT('Ctrl Pts',(-7.27603390513758,-87.5939842542419,
-4.20082013374719));
#31436=CARTESIAN_POINT('Ctrl Pts',(-9.70137854017372,-87.4189842542419,
1.70001511033408E-11));
#31437=CARTESIAN_POINT('Ctrl Pts',(-7.27603390512285,-87.2439842542419,
4.20082013377269));
#31438=CARTESIAN_POINT('Ctrl Pts',(-4.85068927007185,-87.0689842542419,
8.4016402675283));
#31439=CARTESIAN_POINT('Ctrl Pts',(1.46772753381199E-11,-86.8939842542419,
8.40164026751963));
#31440=CARTESIAN_POINT('Ctrl Pts',(4.85068927010168,-86.7189842542419,8.40164026751107));
#31441=CARTESIAN_POINT('Ctrl Pts',(7.27603390513777,-86.5439842542419,4.20082013374685));
#31442=CARTESIAN_POINT('Ctrl Pts',(9.70137854017372,-86.3689842542419,-1.68955643663944E-11));
#31443=CARTESIAN_POINT('Ctrl Pts',(7.2760339051229,-86.1939842542419,-4.20082013377261));
#31444=CARTESIAN_POINT('Ctrl Pts',(4.85068927007194,-86.0189842542419,-8.40164026752825));
#31445=CARTESIAN_POINT('Ctrl Pts',(-1.45867005670255E-11,-85.8439842542419,
-8.40164026751963));
#31446=CARTESIAN_POINT('Ctrl Pts',(-4.85068927010159,-85.6689842542419,
-8.40164026751112));
#31447=CARTESIAN_POINT('Ctrl Pts',(-7.27603390513773,-85.4939842542419,
-4.20082013374693));
#31448=CARTESIAN_POINT('Ctrl Pts',(-9.70137854017372,-85.3189842542419,
1.67909776294481E-11));
#31449=CARTESIAN_POINT('Ctrl Pts',(-7.27603390512294,-85.143984254242,4.20082013377253));
#31450=CARTESIAN_POINT('Ctrl Pts',(-4.85068927007203,-84.9689842542419,
8.40164026752819));
#31451=CARTESIAN_POINT('Ctrl Pts',(1.49737037527755E-11,-84.7939842542419,
8.40164026751963));
#31452=CARTESIAN_POINT('Ctrl Pts',(4.8506892701015,-84.6189842542419,8.40164026751117));
#31453=CARTESIAN_POINT('Ctrl Pts',(7.27603390513768,-84.443984254242,4.20082013374701));
#31454=CARTESIAN_POINT('Ctrl Pts',(9.70137854017372,-84.2689842542419,-1.72378504163881E-11));
#31455=CARTESIAN_POINT('Ctrl Pts',(7.27603390512299,-84.0939842542419,-4.20082013377245));
#31456=CARTESIAN_POINT('Ctrl Pts',(4.85068927007212,-83.9189842542419,-8.40164026752814));
#31457=CARTESIAN_POINT('Ctrl Pts',(-1.4883128981681E-11,-83.7439842542419,
-8.40164026751963));
#31458=CARTESIAN_POINT('Ctrl Pts',(-4.85068927010141,-83.5689842542419,
-8.40164026751123));
#31459=CARTESIAN_POINT('Ctrl Pts',(-7.27603390513763,-83.3939842542419,
-4.20082013374709));
#31460=CARTESIAN_POINT('Ctrl Pts',(-9.70137854017372,-83.2189842542419,
1.71332636794417E-11));
#31461=CARTESIAN_POINT('Ctrl Pts',(-7.2760339051228,-83.0439842542419,4.20082013377279));
#31462=CARTESIAN_POINT('Ctrl Pts',(-4.85068927007221,-82.868984254242,8.40164026752809));
#31463=CARTESIAN_POINT('Ctrl Pts',(1.47925542105866E-11,-82.6939842542419,
8.40164026751963));
#31464=CARTESIAN_POINT('Ctrl Pts',(4.85068927010179,-82.5189842542419,8.401640267511));
#31465=CARTESIAN_POINT('Ctrl Pts',(7.27603390513759,-82.3439842542419,4.20082013374717));
#31466=CARTESIAN_POINT('Ctrl Pts',(9.70137854017372,-82.1689842542419,-1.70286769424954E-11));
#31467=CARTESIAN_POINT('Ctrl Pts',(7.27603390512284,-81.993984254242,-4.20082013377271));
#31468=CARTESIAN_POINT('Ctrl Pts',(4.8506892700723,-81.8189842542419,-8.40164026752804));
#31469=CARTESIAN_POINT('Ctrl Pts',(-1.47019794394921E-11,-81.6439842542419,
-8.40164026751963));
#31470=CARTESIAN_POINT('Ctrl Pts',(-4.8506892701017,-81.4689842542419,-8.40164026751106));
#31471=CARTESIAN_POINT('Ctrl Pts',(-7.27603390513778,-81.293984254242,-4.20082013374683));
#31472=CARTESIAN_POINT('Ctrl Pts',(-9.70137854017372,-81.1189842542419,
1.69240902055491E-11));
#31473=CARTESIAN_POINT('Ctrl Pts',(-7.27603390512289,-80.9439842542419,
4.20082013377263));
#31474=CARTESIAN_POINT('Ctrl Pts',(-4.85068927007191,-80.768984254242,8.40164026752826));
#31475=CARTESIAN_POINT('Ctrl Pts',(1.46114046683977E-11,-80.5939842542419,
8.40164026751963));
#31476=CARTESIAN_POINT('Ctrl Pts',(4.85068927010161,-80.4189842542419,8.40164026751111));
#31477=CARTESIAN_POINT('Ctrl Pts',(7.27603390513774,-80.243984254242,4.20082013374691));
#31478=CARTESIAN_POINT('Ctrl Pts',(9.70137854017372,-80.068984254242,-1.68195034686027E-11));
#31479=CARTESIAN_POINT('Ctrl Pts',(7.27603390512293,-79.8939842542419,-4.20082013377256));
#31480=CARTESIAN_POINT('Ctrl Pts',(4.850689270072,-79.718984254242,-8.40164026752821));
#31481=CARTESIAN_POINT('Ctrl Pts',(-1.49984078541476E-11,-79.5439842542419,
-8.40164026751963));
#31482=CARTESIAN_POINT('Ctrl Pts',(-4.85068927010152,-79.3689842542419,
-8.40164026751116));
#31483=CARTESIAN_POINT('Ctrl Pts',(-7.27603390513769,-79.193984254242,-4.20082013374699));
#31484=CARTESIAN_POINT('Ctrl Pts',(-9.70137854017372,-79.0189842542419,
1.72663762555427E-11));
#31485=CARTESIAN_POINT('Ctrl Pts',(-7.27603390512298,-78.8439842542419,
4.20082013377248));
#31486=CARTESIAN_POINT('Ctrl Pts',(-4.85068927007209,-78.668984254242,8.40164026752815));
#31487=CARTESIAN_POINT('Ctrl Pts',(1.49078330830532E-11,-78.493984254242,
8.40164026751963));
#31488=CARTESIAN_POINT('Ctrl Pts',(4.85068927010143,-78.3189842542419,8.40164026751122));
#31489=CARTESIAN_POINT('Ctrl Pts',(7.27603390513765,-78.143984254242,4.20082013374707));
#31490=CARTESIAN_POINT('Ctrl Pts',(9.70137854017372,-77.9689842542419,-1.71617895185964E-11));
#31491=CARTESIAN_POINT('Ctrl Pts',(7.27603390512302,-77.7939842542419,-4.2008201337724));
#31492=CARTESIAN_POINT('Ctrl Pts',(4.85068927007219,-77.618984254242,-8.4016402675281));
#31493=CARTESIAN_POINT('Ctrl Pts',(-1.48172583119587E-11,-77.443984254242,
-8.40164026751963));
#31494=CARTESIAN_POINT('Ctrl Pts',(-4.85068927010182,-77.268984254242,-8.40164026751099));
#31495=CARTESIAN_POINT('Ctrl Pts',(-7.2760339051376,-77.0939842542419,-4.20082013374715));
#31496=CARTESIAN_POINT('Ctrl Pts',(-9.70137854017372,-76.918984254242,1.705720278165E-11));
#31497=CARTESIAN_POINT('Ctrl Pts',(-7.27603390512283,-76.743984254242,4.20082013377273));
#31498=CARTESIAN_POINT('Ctrl Pts',(-4.85068927007227,-76.5689842542419,
8.40164026752805));
#31499=CARTESIAN_POINT('Ctrl Pts',(1.47266835408643E-11,-76.393984254242,
8.40164026751963));
#31500=CARTESIAN_POINT('Ctrl Pts',(4.85068927010173,-76.2189842542419,8.40164026751104));
#31501=CARTESIAN_POINT('Ctrl Pts',(7.27603390513756,-76.0439842542419,4.20082013374722));
#31502=CARTESIAN_POINT('Ctrl Pts',(9.70137854017372,-75.868984254242,-1.69526160447037E-11));
#31503=CARTESIAN_POINT('Ctrl Pts',(7.27603390512287,-75.693984254242,-4.20082013377265));
#31504=CARTESIAN_POINT('Ctrl Pts',(4.85068927007189,-75.518984254242,-8.40164026752827));
#31505=CARTESIAN_POINT('Ctrl Pts',(-1.46361087697698E-11,-75.343984254242,
-8.40164026751963));
#31506=CARTESIAN_POINT('Ctrl Pts',(-4.85068927010164,-75.1689842542419,
-8.40164026751109));
#31507=CARTESIAN_POINT('Ctrl Pts',(-7.27603390513775,-74.993984254242,-4.20082013374689));
#31508=CARTESIAN_POINT('Ctrl Pts',(-9.70137854017372,-74.818984254242,1.68480293077573E-11));
#31509=CARTESIAN_POINT('Ctrl Pts',(-7.27603390512292,-74.643984254242,4.20082013377258));
#31510=CARTESIAN_POINT('Ctrl Pts',(-4.85068927007198,-74.4689842542419,
8.40164026752822));
#31511=CARTESIAN_POINT('Ctrl Pts',(1.45455339986754E-11,-74.293984254242,
8.40164026751963));
#31512=CARTESIAN_POINT('Ctrl Pts',(4.85068927010155,-74.118984254242,8.40164026751115));
#31513=CARTESIAN_POINT('Ctrl Pts',(7.2760339051377,-73.943984254242,4.20082013374697));
#31514=CARTESIAN_POINT('Ctrl Pts',(9.70137854017372,-73.768984254242,-1.72949020946973E-11));
#31515=CARTESIAN_POINT('Ctrl Pts',(7.27603390512296,-73.593984254242,-4.2008201337725));
#31516=CARTESIAN_POINT('Ctrl Pts',(4.85068927007207,-73.4189842542419,-8.40164026752817));
#31517=CARTESIAN_POINT('Ctrl Pts',(-1.49325371844254E-11,-73.243984254242,
-8.40164026751963));
#31518=CARTESIAN_POINT('Ctrl Pts',(-4.85068927010146,-73.068984254242,-8.4016402675112));
#31519=CARTESIAN_POINT('Ctrl Pts',(-7.27603390513766,-72.893984254242,-4.20082013374705));
#31520=CARTESIAN_POINT('Ctrl Pts',(-9.70137854017372,-72.718984254242,1.7190315357751E-11));
#31521=CARTESIAN_POINT('Ctrl Pts',(-7.27603390512301,-72.543984254242,4.20082013377242));
#31522=CARTESIAN_POINT('Ctrl Pts',(-4.85068927007216,-72.368984254242,8.40164026752812));
#31523=CARTESIAN_POINT('Ctrl Pts',(1.48419624133309E-11,-72.193984254242,
8.40164026751963));
#31524=CARTESIAN_POINT('Ctrl Pts',(4.85068927010137,-72.018984254242,8.40164026751125));
#31525=CARTESIAN_POINT('Ctrl Pts',(7.27603390513761,-71.843984254242,4.20082013374713));
#31526=CARTESIAN_POINT('Ctrl Pts',(9.70137854017372,-71.6689842542419,-1.70857286208046E-11));
#31527=CARTESIAN_POINT('Ctrl Pts',(7.27603390512282,-71.493984254242,-4.20082013377275));
#31528=CARTESIAN_POINT('Ctrl Pts',(4.85068927007225,-71.318984254242,-8.40164026752806));
#31529=CARTESIAN_POINT('Ctrl Pts',(-1.47513876422365E-11,-71.143984254242,
-8.40164026751963));
#31530=CARTESIAN_POINT('Ctrl Pts',(-4.85068927010175,-70.968984254242,-8.40164026751103));
#31531=CARTESIAN_POINT('Ctrl Pts',(-7.27603390513757,-70.793984254242,-4.2008201337472));
#31532=CARTESIAN_POINT('Ctrl Pts',(-9.70137854017372,-70.618984254242,1.69811418838583E-11));
#31533=CARTESIAN_POINT('Ctrl Pts',(-7.27603390512286,-70.443984254242,4.20082013377267));
#31534=CARTESIAN_POINT('Ctrl Pts',(-4.85068927007234,-70.268984254242,8.40164026752801));
#31535=CARTESIAN_POINT('Ctrl Pts',(1.4660812871142E-11,-70.093984254242,
8.40164026751963));
#31536=CARTESIAN_POINT('Ctrl Pts',(4.85068927010166,-69.918984254242,8.40164026751108));
#31537=CARTESIAN_POINT('Ctrl Pts',(7.27603390513776,-69.743984254242,4.20082013374687));
#31538=CARTESIAN_POINT('Ctrl Pts',(9.70137854017372,-69.568984254242,-1.6876555146912E-11));
#31539=CARTESIAN_POINT('Ctrl Pts',(7.27603390512291,-69.393984254242,-4.2008201337726));
#31540=CARTESIAN_POINT('Ctrl Pts',(4.85068927007195,-69.218984254242,-8.40164026752823));
#31541=CARTESIAN_POINT('Ctrl Pts',(-1.45702381000475E-11,-69.043984254242,
-8.40164026751963));
#31542=CARTESIAN_POINT('Ctrl Pts',(-4.85068927010157,-68.868984254242,-8.40164026751113));
#31543=CARTESIAN_POINT('Ctrl Pts',(-7.27603390513772,-68.693984254242,-4.20082013374695));
#31544=CARTESIAN_POINT('Ctrl Pts',(-9.70137854017372,-68.518984254242,1.67719684099656E-11));
#31545=CARTESIAN_POINT('Ctrl Pts',(-7.27603390512295,-68.343984254242,4.20082013377252));
#31546=CARTESIAN_POINT('Ctrl Pts',(-4.85068927007204,-68.168984254242,8.40164026752818));
#31547=CARTESIAN_POINT('Ctrl Pts',(1.49572412857975E-11,-67.993984254242,
8.40164026751963));
#31548=CARTESIAN_POINT('Ctrl Pts',(4.85068927010148,-67.818984254242,8.40164026751119));
#31549=CARTESIAN_POINT('Ctrl Pts',(7.27603390513767,-67.643984254242,4.20082013374703));
#31550=CARTESIAN_POINT('Ctrl Pts',(9.70137854017372,-67.468984254242,-1.72188411969056E-11));
#31551=CARTESIAN_POINT('Ctrl Pts',(7.276033905123,-67.293984254242,-4.20082013377244));
#31552=CARTESIAN_POINT('Ctrl Pts',(4.85068927007213,-67.118984254242,-8.40164026752813));
#31553=CARTESIAN_POINT('Ctrl Pts',(-1.48666665147031E-11,-66.943984254242,
-8.40164026751963));
#31554=CARTESIAN_POINT('Ctrl Pts',(-4.85068927010139,-66.768984254242,-8.40164026751124));
#31555=CARTESIAN_POINT('Ctrl Pts',(-7.27603390513763,-66.593984254242,-4.2008201337471));
#31556=CARTESIAN_POINT('Ctrl Pts',(-9.70137854017372,-66.418984254242,1.71142544599593E-11));
#31557=CARTESIAN_POINT('Ctrl Pts',(-7.27603390512304,-66.243984254242,4.20082013377236));
#31558=CARTESIAN_POINT('Ctrl Pts',(-4.85068927007222,-66.068984254242,8.40164026752808));
#31559=CARTESIAN_POINT('Ctrl Pts',(1.47760917436086E-11,-65.893984254242,
8.40164026751963));
#31560=CARTESIAN_POINT('Ctrl Pts',(4.85068927010178,-65.718984254242,8.40164026751101));
#31561=CARTESIAN_POINT('Ctrl Pts',(7.27603390513758,-65.543984254242,4.20082013374718));
#31562=CARTESIAN_POINT('Ctrl Pts',(9.70137854017372,-65.368984254242,-1.70096677230129E-11));
#31563=CARTESIAN_POINT('Ctrl Pts',(7.27603390512285,-65.193984254242,-4.2008201337727));
#31564=CARTESIAN_POINT('Ctrl Pts',(4.85068927007232,-65.018984254242,-8.40164026752803));
#31565=CARTESIAN_POINT('Ctrl Pts',(-1.46855169725142E-11,-64.843984254242,
-8.40164026751963));
#31566=CARTESIAN_POINT('Ctrl Pts',(-4.85068927010169,-64.668984254242,-8.40164026751107));
#31567=CARTESIAN_POINT('Ctrl Pts',(-7.27603390513754,-64.493984254242,-4.20082013374726));
#31568=CARTESIAN_POINT('Ctrl Pts',(-9.70137854017372,-64.318984254242,1.69050809860666E-11));
#31569=CARTESIAN_POINT('Ctrl Pts',(-7.27603390512289,-64.143984254242,4.20082013377262));
#31570=CARTESIAN_POINT('Ctrl Pts',(-4.85068927007193,-63.968984254242,8.40164026752825));
#31571=CARTESIAN_POINT('Ctrl Pts',(1.45949422014197E-11,-63.793984254242,
8.40164026751963));
#31572=CARTESIAN_POINT('Ctrl Pts',(4.8506892701016,-63.618984254242,8.40164026751112));
#31573=CARTESIAN_POINT('Ctrl Pts',(7.27603390513773,-63.443984254242,4.20082013374692));
#31574=CARTESIAN_POINT('Ctrl Pts',(9.70137854017372,-63.268984254242,-1.68004942491202E-11));
#31575=CARTESIAN_POINT('Ctrl Pts',(7.27603390512294,-63.093984254242,-4.20082013377254));
#31576=CARTESIAN_POINT('Ctrl Pts',(4.85068927007202,-62.918984254242,-8.4016402675282));
#31577=CARTESIAN_POINT('Ctrl Pts',(-1.45043674303253E-11,-62.743984254242,
-8.40164026751963));
#31578=CARTESIAN_POINT('Ctrl Pts',(-4.85068927010151,-62.568984254242,-8.40164026751117));
#31579=CARTESIAN_POINT('Ctrl Pts',(-7.27603390513768,-62.393984254242,-4.200820133747));
#31580=CARTESIAN_POINT('Ctrl Pts',(-9.70137854017372,-62.218984254242,1.72473670360602E-11));
#31581=CARTESIAN_POINT('Ctrl Pts',(-7.27603390512298,-62.043984254242,4.20082013377246));
#31582=CARTESIAN_POINT('Ctrl Pts',(-4.85068927007211,-61.868984254242,8.40164026752814));
#31583=CARTESIAN_POINT('Ctrl Pts',(1.48913706160753E-11,-61.693984254242,
8.40164026751963));
#31584=CARTESIAN_POINT('Ctrl Pts',(4.85068927010141,-61.518984254242,8.40164026751122));
#31585=CARTESIAN_POINT('Ctrl Pts',(7.27603390513764,-61.343984254242,4.20082013374708));
#31586=CARTESIAN_POINT('Ctrl Pts',(9.70137854017372,-61.168984254242,-1.71427802991139E-11));
#31587=CARTESIAN_POINT('Ctrl Pts',(7.27603390512303,-60.993984254242,-4.20082013377238));
#31588=CARTESIAN_POINT('Ctrl Pts',(4.8506892700722,-60.818984254242,-8.40164026752809));
#31589=CARTESIAN_POINT('Ctrl Pts',(-1.48007958449808E-11,-60.643984254242,
-8.40164026751963));
#31590=CARTESIAN_POINT('Ctrl Pts',(-4.8506892701018,-60.468984254242,-8.401640267511));
#31591=CARTESIAN_POINT('Ctrl Pts',(-7.27603390513759,-60.293984254242,-4.20082013374716));
#31592=CARTESIAN_POINT('Ctrl Pts',(-9.70137854017372,-60.118984254242,1.70381935621676E-11));
#31593=CARTESIAN_POINT('Ctrl Pts',(-7.27603390512284,-59.943984254242,4.20082013377272));
#31594=CARTESIAN_POINT('Ctrl Pts',(-4.85068927007229,-59.768984254242,8.40164026752804));
#31595=CARTESIAN_POINT('Ctrl Pts',(1.47102210738864E-11,-59.593984254242,
8.40164026751963));
#31596=CARTESIAN_POINT('Ctrl Pts',(4.85068927010171,-59.418984254242,8.40164026751105));
#31597=CARTESIAN_POINT('Ctrl Pts',(7.27603390513755,-59.243984254242,4.20082013374724));
#31598=CARTESIAN_POINT('Ctrl Pts',(9.70137854017372,-59.068984254242,-1.69336068252212E-11));
#31599=CARTESIAN_POINT('Ctrl Pts',(7.27603390512288,-58.893984254242,-4.20082013377264));
#31600=CARTESIAN_POINT('Ctrl Pts',(4.85068927007238,-58.718984254242,-8.40164026752799));
#31601=CARTESIAN_POINT('Ctrl Pts',(-1.46196463027919E-11,-58.543984254242,
-8.40164026751963));
#31602=CARTESIAN_POINT('Ctrl Pts',(-4.85068927010162,-58.368984254242,-8.40164026751111));
#31603=CARTESIAN_POINT('Ctrl Pts',(-7.27603390513774,-58.193984254242,-4.2008201337469));
#31604=CARTESIAN_POINT('Ctrl Pts',(-9.70137854017372,-58.018984254242,1.68290200882749E-11));
#31605=CARTESIAN_POINT('Ctrl Pts',(-7.27603390512293,-57.843984254242,4.20082013377256));
#31606=CARTESIAN_POINT('Ctrl Pts',(-4.85068927007199,-57.668984254242,8.40164026752821));
#31607=CARTESIAN_POINT('Ctrl Pts',(1.45290715316974E-11,-57.493984254242,
8.40164026751963));
#31608=CARTESIAN_POINT('Ctrl Pts',(4.85068927010153,-57.318984254242,8.40164026751116));
#31609=CARTESIAN_POINT('Ctrl Pts',(7.2760339051377,-57.143984254242,4.20082013374698));
#31610=CARTESIAN_POINT('Ctrl Pts',(9.70137854017372,-56.968984254242,-1.67244333513285E-11));
#31611=CARTESIAN_POINT('Ctrl Pts',(7.27603390512297,-56.793984254242,-4.20082013377248));
#31612=CARTESIAN_POINT('Ctrl Pts',(4.85068927007208,-56.618984254242,-8.40164026752816));
#31613=CARTESIAN_POINT('Ctrl Pts',(-1.49160747174474E-11,-56.443984254242,
-8.40164026751963));
#31614=CARTESIAN_POINT('Ctrl Pts',(-4.85068927010144,-56.268984254242,-8.40164026751121));
#31615=CARTESIAN_POINT('Ctrl Pts',(-7.27603390513765,-56.093984254242,-4.20082013374706));
#31616=CARTESIAN_POINT('Ctrl Pts',(-9.70137854017372,-55.918984254242,1.71713061382685E-11));
#31617=CARTESIAN_POINT('Ctrl Pts',(-7.27603390512302,-55.743984254242,4.2008201337724));
#31618=CARTESIAN_POINT('Ctrl Pts',(-4.85068927007218,-55.568984254242,8.40164026752811));
#31619=CARTESIAN_POINT('Ctrl Pts',(1.4825499946353E-11,-55.393984254242,
8.40164026751963));
#31620=CARTESIAN_POINT('Ctrl Pts',(4.85068927010135,-55.218984254242,8.40164026751126));
#31621=CARTESIAN_POINT('Ctrl Pts',(7.27603390513761,-55.043984254242,4.20082013374714));
#31622=CARTESIAN_POINT('Ctrl Pts',(9.70137854017372,-54.868984254242,-1.70667194013222E-11));
#31623=CARTESIAN_POINT('Ctrl Pts',(7.27603390512282,-54.693984254242,-4.20082013377274));
#31624=CARTESIAN_POINT('Ctrl Pts',(4.85068927007227,-54.518984254242,-8.40164026752806));
#31625=CARTESIAN_POINT('Ctrl Pts',(-1.47349251752585E-11,-54.343984254242,
-8.40164026751963));
#31626=CARTESIAN_POINT('Ctrl Pts',(-4.85068927010174,-54.168984254242,-8.40164026751104));
#31627=CARTESIAN_POINT('Ctrl Pts',(-7.27603390513756,-53.993984254242,-4.20082013374722));
#31628=CARTESIAN_POINT('Ctrl Pts',(-9.70137854017372,-53.818984254242,1.69621326643758E-11));
#31629=CARTESIAN_POINT('Ctrl Pts',(-7.27603390512287,-53.643984254242,4.20082013377266));
#31630=CARTESIAN_POINT('Ctrl Pts',(-4.85068927007236,-53.468984254242,8.401640267528));
#31631=CARTESIAN_POINT('Ctrl Pts',(1.46443504041641E-11,-53.293984254242,
8.40164026751963));
#31632=CARTESIAN_POINT('Ctrl Pts',(4.85068927010165,-53.118984254242,8.40164026751109));
#31633=CARTESIAN_POINT('Ctrl Pts',(7.27603390513752,-52.943984254242,4.2008201337473));
#31634=CARTESIAN_POINT('Ctrl Pts',(9.70137854017372,-52.768984254242,-1.68575459274295E-11));
#31635=CARTESIAN_POINT('Ctrl Pts',(7.27603390512292,-52.593984254242,-4.20082013377258));
#31636=CARTESIAN_POINT('Ctrl Pts',(4.85068927007197,-52.418984254242,-8.40164026752823));
#31637=CARTESIAN_POINT('Ctrl Pts',(-1.45537756330696E-11,-52.243984254242,
-8.40164026751963));
#31638=CARTESIAN_POINT('Ctrl Pts',(-4.85068927010155,-52.068984254242,-8.40164026751114));
#31639=CARTESIAN_POINT('Ctrl Pts',(-7.27603390513771,-51.893984254242,-4.20082013374696));
#31640=CARTESIAN_POINT('Ctrl Pts',(-9.70137854017372,-51.718984254242,1.67529591904832E-11));
#31641=CARTESIAN_POINT('Ctrl Pts',(-7.27603390512296,-51.543984254242,4.2008201337725));
#31642=CARTESIAN_POINT('Ctrl Pts',(-4.85068927007206,-51.368984254242,8.40164026752817));
#31643=CARTESIAN_POINT('Ctrl Pts',(1.44632008619752E-11,-51.193984254242,
8.40164026751963));
#31644=CARTESIAN_POINT('Ctrl Pts',(4.85068927010146,-51.018984254242,8.4016402675112));
#31645=CARTESIAN_POINT('Ctrl Pts',(7.27603390513766,-50.843984254242,4.20082013374704));
#31646=CARTESIAN_POINT('Ctrl Pts',(9.70137854017372,-50.668984254242,-1.71998319774232E-11));
#31647=CARTESIAN_POINT('Ctrl Pts',(7.27603390512301,-50.493984254242,-4.20082013377243));
#31648=CARTESIAN_POINT('Ctrl Pts',(4.85068927007215,-50.318984254242,-8.40164026752812));
#31649=CARTESIAN_POINT('Ctrl Pts',(-1.48502040477252E-11,-50.143984254242,
-8.40164026751963));
#31650=CARTESIAN_POINT('Ctrl Pts',(-4.85068927010137,-49.968984254242,-8.40164026751125));
#31651=CARTESIAN_POINT('Ctrl Pts',(-7.27603390513762,-49.793984254242,-4.20082013374712));
#31652=CARTESIAN_POINT('Ctrl Pts',(-9.70137854017372,-49.618984254242,1.70952452404768E-11));
#31653=CARTESIAN_POINT('Ctrl Pts',(-7.27603390512305,-49.443984254242,4.20082013377235));
#31654=CARTESIAN_POINT('Ctrl Pts',(-4.85068927007224,-49.268984254242,8.40164026752807));
#31655=CARTESIAN_POINT('Ctrl Pts',(1.47596292766307E-11,-49.093984254242,
8.40164026751963));
#31656=CARTESIAN_POINT('Ctrl Pts',(4.85068927010176,-48.918984254242,8.40164026751102));
#31657=CARTESIAN_POINT('Ctrl Pts',(7.27603390513757,-48.743984254242,4.2008201337472));
#31658=CARTESIAN_POINT('Ctrl Pts',(9.70137854017372,-48.568984254242,-1.69906585035305E-11));
#31659=CARTESIAN_POINT('Ctrl Pts',(7.27603390512286,-48.393984254242,-4.20082013377268));
#31660=CARTESIAN_POINT('Ctrl Pts',(4.85068927007233,-48.218984254242,-8.40164026752802));
#31661=CARTESIAN_POINT('Ctrl Pts',(-1.46690545055362E-11,-48.043984254242,
-8.40164026751963));
#31662=CARTESIAN_POINT('Ctrl Pts',(-4.85068927010167,-47.868984254242,-8.40164026751108));
#31663=CARTESIAN_POINT('Ctrl Pts',(-7.27603390513753,-47.693984254242,-4.20082013374728));
#31664=CARTESIAN_POINT('Ctrl Pts',(-7.69929559114725,-47.6634439368035,
-3.46770938867822));
#31665=CARTESIAN_POINT('Ctrl Pts',(-7.96780251527898,-47.63,-2.66489817109789));
#31666=CARTESIAN_POINT('',(-0.219644606349537,-212.63,-9.92210040505713));
#31667=CARTESIAN_POINT('Ctrl Pts',(5.91264939824166,-212.63,5.96893091585755));
#31668=CARTESIAN_POINT('Ctrl Pts',(6.45001176255729,-212.63,5.51316655921169));
#31669=CARTESIAN_POINT('Ctrl Pts',(6.92646504757685,-212.63,4.99014851913996));
#31670=CARTESIAN_POINT('Ctrl Pts',(7.64146177750064,-212.63,3.96829926249844));
#31671=CARTESIAN_POINT('Ctrl Pts',(8.02934603926417,-212.63,3.32494664782914));
#31672=CARTESIAN_POINT('Ctrl Pts',(8.75489545839817,-212.63,1.42020078435432));
#31673=CARTESIAN_POINT('Ctrl Pts',(8.95163602245128,-212.63,0.279729502662558));
#31674=CARTESIAN_POINT('Ctrl Pts',(8.90204310970132,-212.63,-1.94200526332423));
#31675=CARTESIAN_POINT('Ctrl Pts',(8.6828950463362,-212.63,-3.00390386902858));
#31676=CARTESIAN_POINT('Ctrl Pts',(7.851506811291,-212.63,-5.05909339484079));
#31677=CARTESIAN_POINT('Ctrl Pts',(7.21763657197169,-212.63,-6.04291134052863));
#31678=CARTESIAN_POINT('Ctrl Pts',(5.59478772607511,-212.63,-7.78711679211931));
#31679=CARTESIAN_POINT('Ctrl Pts',(4.5846114302215,-212.63,-8.52028630432628));
#31680=CARTESIAN_POINT('Ctrl Pts',(2.63065283482949,-212.63,-9.42649812028965));
#31681=CARTESIAN_POINT('Ctrl Pts',(1.41906832976769,-212.63,-9.86110934044648));
#31682=CARTESIAN_POINT('Ctrl Pts',(-0.219644606349541,-212.63,-9.9221004050572));
#31683=CARTESIAN_POINT('Ctrl Pts',(-0.219644606349537,-212.63,-9.92210040505713));
#31684=CARTESIAN_POINT('Ctrl Pts',(-5.80268971544237,-212.457306795807,
-9.79850905895531));
#31685=CARTESIAN_POINT('Ctrl Pts',(-8.59489616871563,-212.28675111262,-4.96226561664434));
#31686=CARTESIAN_POINT('Ctrl Pts',(-11.4598615582757,-212.11175111262,2.05132644302783E-11));
#31687=CARTESIAN_POINT('Ctrl Pts',(-8.59489616869786,-211.93675111262,4.96226561667511));
#31688=CARTESIAN_POINT('Ctrl Pts',(-5.72993077912007,-211.76175111262,9.9245312333297));
#31689=CARTESIAN_POINT('Ctrl Pts',(1.77644004088984E-11,-211.58675111262,
9.92453123331945));
#31690=CARTESIAN_POINT('Ctrl Pts',(5.72993077915559,-211.41175111262,9.92453123330919));
#31691=CARTESIAN_POINT('Ctrl Pts',(8.59489616871563,-211.23675111262,4.96226561664434));
#31692=CARTESIAN_POINT('Ctrl Pts',(11.4598615582757,-211.06175111262,-2.05118610020007E-11));
#31693=CARTESIAN_POINT('Ctrl Pts',(8.59489616869787,-210.88675111262,-4.9622656166751));
#31694=CARTESIAN_POINT('Ctrl Pts',(5.72993077912007,-210.71175111262,-9.9245312333297));
#31695=CARTESIAN_POINT('Ctrl Pts',(-1.77631850043576E-11,-210.53675111262,
-9.92453123331945));
#31696=CARTESIAN_POINT('Ctrl Pts',(-5.72993077915559,-210.36175111262,-9.9245312333092));
#31697=CARTESIAN_POINT('Ctrl Pts',(-8.59489616871563,-210.18675111262,-4.96226561664434));
#31698=CARTESIAN_POINT('Ctrl Pts',(-11.4598615582757,-210.01175111262,2.05002791719943E-11));
#31699=CARTESIAN_POINT('Ctrl Pts',(-8.59489616869787,-209.83675111262,4.9622656166751));
#31700=CARTESIAN_POINT('Ctrl Pts',(-5.72993077912008,-209.66175111262,9.9245312333297));
#31701=CARTESIAN_POINT('Ctrl Pts',(1.77619695998168E-11,-209.48675111262,
9.92453123331945));
#31702=CARTESIAN_POINT('Ctrl Pts',(5.72993077915559,-209.31175111262,9.9245312333092));
#31703=CARTESIAN_POINT('Ctrl Pts',(8.59489616871562,-209.13675111262,4.96226561664435));
#31704=CARTESIAN_POINT('Ctrl Pts',(11.4598615582757,-208.96175111262,-2.05090541454455E-11));
#31705=CARTESIAN_POINT('Ctrl Pts',(8.59489616869787,-208.78675111262,-4.9622656166751));
#31706=CARTESIAN_POINT('Ctrl Pts',(5.72993077912008,-208.61175111262,-9.9245312333297));
#31707=CARTESIAN_POINT('Ctrl Pts',(-1.7760754195276E-11,-208.43675111262,
-9.92453123331945));
#31708=CARTESIAN_POINT('Ctrl Pts',(-5.72993077915559,-208.26175111262,-9.9245312333092));
#31709=CARTESIAN_POINT('Ctrl Pts',(-8.59489616871562,-208.08675111262,-4.96226561664435));
#31710=CARTESIAN_POINT('Ctrl Pts',(-11.4598615582757,-207.91175111262,2.04872939137103E-11));
#31711=CARTESIAN_POINT('Ctrl Pts',(-8.59489616869787,-207.73675111262,4.9622656166751));
#31712=CARTESIAN_POINT('Ctrl Pts',(-5.72993077912008,-207.56175111262,9.9245312333297));
#31713=CARTESIAN_POINT('Ctrl Pts',(1.7741909281801E-11,-207.38675111262,
9.92453123331945));
#31714=CARTESIAN_POINT('Ctrl Pts',(5.72993077915559,-207.21175111262,9.9245312333092));
#31715=CARTESIAN_POINT('Ctrl Pts',(8.59489616871562,-207.03675111262,4.96226561664435));
#31716=CARTESIAN_POINT('Ctrl Pts',(11.4598615582757,-206.86175111262,-2.04858904854327E-11));
#31717=CARTESIAN_POINT('Ctrl Pts',(8.59489616869788,-206.68675111262,-4.96226561667508));
#31718=CARTESIAN_POINT('Ctrl Pts',(5.7299307791201,-206.51175111262,-9.92453123332968));
#31719=CARTESIAN_POINT('Ctrl Pts',(-1.77583233861944E-11,-206.33675111262,
-9.92453123331945));
#31720=CARTESIAN_POINT('Ctrl Pts',(-5.72993077915558,-206.16175111262,-9.9245312333092));
#31721=CARTESIAN_POINT('Ctrl Pts',(-8.59489616871562,-205.98675111262,-4.96226561664435));
#31722=CARTESIAN_POINT('Ctrl Pts',(-11.4598615582757,-205.81175111262,2.04844870571551E-11));
#31723=CARTESIAN_POINT('Ctrl Pts',(-8.59489616869788,-205.63675111262,4.96226561667508));
#31724=CARTESIAN_POINT('Ctrl Pts',(-5.7299307791201,-205.46175111262,9.92453123332968));
#31725=CARTESIAN_POINT('Ctrl Pts',(1.77571079816536E-11,-205.28675111262,
9.92453123331945));
#31726=CARTESIAN_POINT('Ctrl Pts',(5.72993077915558,-205.11175111262,9.9245312333092));
#31727=CARTESIAN_POINT('Ctrl Pts',(8.59489616871562,-204.93675111262,4.96226561664436));
#31728=CARTESIAN_POINT('Ctrl Pts',(11.4598615582757,-204.76175111262,-2.04830836288775E-11));
#31729=CARTESIAN_POINT('Ctrl Pts',(8.59489616869788,-204.58675111262,-4.96226561667508));
#31730=CARTESIAN_POINT('Ctrl Pts',(5.72993077912011,-204.41175111262,-9.92453123332968));
#31731=CARTESIAN_POINT('Ctrl Pts',(-1.77558925771128E-11,-204.23675111262,
-9.92453123331945));
#31732=CARTESIAN_POINT('Ctrl Pts',(-5.72993077915558,-204.06175111262,-9.9245312333092));
#31733=CARTESIAN_POINT('Ctrl Pts',(-8.59489616871562,-203.88675111262,-4.96226561664436));
#31734=CARTESIAN_POINT('Ctrl Pts',(-11.4598615582757,-203.71175111262,2.04816802005999E-11));
#31735=CARTESIAN_POINT('Ctrl Pts',(-8.59489616869788,-203.53675111262,4.96226561667508));
#31736=CARTESIAN_POINT('Ctrl Pts',(-5.72993077912011,-203.36175111262,9.92453123332968));
#31737=CARTESIAN_POINT('Ctrl Pts',(1.77194181547037E-11,-203.18675111262,
9.92453123331945));
#31738=CARTESIAN_POINT('Ctrl Pts',(5.72993077915558,-203.01175111262,9.9245312333092));
#31739=CARTESIAN_POINT('Ctrl Pts',(8.59489616871562,-202.83675111262,4.96226561664436));
#31740=CARTESIAN_POINT('Ctrl Pts',(11.4598615582757,-202.66175111262,-2.04802767723223E-11));
#31741=CARTESIAN_POINT('Ctrl Pts',(8.59489616869788,-202.48675111262,-4.96226561667508));
#31742=CARTESIAN_POINT('Ctrl Pts',(5.72993077912011,-202.31175111262,-9.92453123332968));
#31743=CARTESIAN_POINT('Ctrl Pts',(-1.77182027501629E-11,-202.13675111262,
-9.92453123331945));
#31744=CARTESIAN_POINT('Ctrl Pts',(-5.72993077915558,-201.96175111262,-9.9245312333092));
#31745=CARTESIAN_POINT('Ctrl Pts',(-8.59489616871562,-201.78675111262,-4.96226561664436));
#31746=CARTESIAN_POINT('Ctrl Pts',(-11.4598615582757,-201.61175111262,2.04381597371295E-11));
#31747=CARTESIAN_POINT('Ctrl Pts',(-8.59489616869788,-201.43675111262,4.96226561667508));
#31748=CARTESIAN_POINT('Ctrl Pts',(-5.72993077912007,-201.26175111262,9.9245312333297));
#31749=CARTESIAN_POINT('Ctrl Pts',(1.77169873456222E-11,-201.08675111262,
9.92453123331945));
#31750=CARTESIAN_POINT('Ctrl Pts',(5.72993077915558,-200.91175111262,9.9245312333092));
#31751=CARTESIAN_POINT('Ctrl Pts',(8.5948961687156,-200.73675111262,4.96226561664439));
#31752=CARTESIAN_POINT('Ctrl Pts',(11.4598615582757,-200.56175111262,-2.04774699157671E-11));
#31753=CARTESIAN_POINT('Ctrl Pts',(8.5948961686979,-200.38675111262,-4.96226561667505));
#31754=CARTESIAN_POINT('Ctrl Pts',(5.72993077912011,-200.21175111262,-9.92453123332968));
#31755=CARTESIAN_POINT('Ctrl Pts',(-1.77510309589497E-11,-200.03675111262,
-9.92453123331945));
#31756=CARTESIAN_POINT('Ctrl Pts',(-5.72993077915554,-199.86175111262,-9.92453123330922));
#31757=CARTESIAN_POINT('Ctrl Pts',(-8.59489616871562,-199.68675111262,-4.96226561664436));
#31758=CARTESIAN_POINT('Ctrl Pts',(-11.4598615582757,-199.51175111262,2.04353528805743E-11));
#31759=CARTESIAN_POINT('Ctrl Pts',(-8.59489616869788,-199.33675111262,4.96226561667507));
#31760=CARTESIAN_POINT('Ctrl Pts',(-5.72993077912008,-199.16175111262,9.9245312333297));
#31761=CARTESIAN_POINT('Ctrl Pts',(1.77145565365406E-11,-198.98675111262,
9.92453123331945));
#31762=CARTESIAN_POINT('Ctrl Pts',(5.72993077915557,-198.81175111262,9.9245312333092));
#31763=CARTESIAN_POINT('Ctrl Pts',(8.5948961687156,-198.63675111262,4.96226561664439));
#31764=CARTESIAN_POINT('Ctrl Pts',(11.4598615582757,-198.46175111262,-2.04746630592119E-11));
#31765=CARTESIAN_POINT('Ctrl Pts',(8.5948961686979,-198.28675111262,-4.96226561667504));
#31766=CARTESIAN_POINT('Ctrl Pts',(5.72993077912011,-198.11175111262,-9.92453123332968));
#31767=CARTESIAN_POINT('Ctrl Pts',(-1.77486001498681E-11,-197.93675111262,
-9.92453123331945));
#31768=CARTESIAN_POINT('Ctrl Pts',(-5.72993077915554,-197.76175111262,-9.92453123330922));
#31769=CARTESIAN_POINT('Ctrl Pts',(-8.59489616871562,-197.58675111262,-4.96226561664436));
#31770=CARTESIAN_POINT('Ctrl Pts',(-11.4598615582757,-197.41175111262,2.04325460240191E-11));
#31771=CARTESIAN_POINT('Ctrl Pts',(-8.59489616869789,-197.23675111262,4.96226561667507));
#31772=CARTESIAN_POINT('Ctrl Pts',(-5.72993077912015,-197.06175111262,9.92453123332966));
#31773=CARTESIAN_POINT('Ctrl Pts',(1.7712125727459E-11,-196.88675111262,
9.92453123331945));
#31774=CARTESIAN_POINT('Ctrl Pts',(5.72993077915557,-196.71175111262,9.9245312333092));
#31775=CARTESIAN_POINT('Ctrl Pts',(8.5948961687156,-196.53675111262,4.9622656166444));
#31776=CARTESIAN_POINT('Ctrl Pts',(11.4598615582757,-196.36175111262,-2.04718562026567E-11));
#31777=CARTESIAN_POINT('Ctrl Pts',(8.5948961686979,-196.18675111262,-4.96226561667504));
#31778=CARTESIAN_POINT('Ctrl Pts',(5.72993077912011,-196.01175111262,-9.92453123332968));
#31779=CARTESIAN_POINT('Ctrl Pts',(-1.77461693407865E-11,-195.83675111262,
-9.92453123331945));
#31780=CARTESIAN_POINT('Ctrl Pts',(-5.72993077915554,-195.66175111262,-9.92453123330922));
#31781=CARTESIAN_POINT('Ctrl Pts',(-8.59489616871562,-195.48675111262,-4.96226561664437));
#31782=CARTESIAN_POINT('Ctrl Pts',(-11.4598615582757,-195.31175111262,2.04297391674638E-11));
#31783=CARTESIAN_POINT('Ctrl Pts',(-8.59489616869789,-195.13675111262,4.96226561667507));
#31784=CARTESIAN_POINT('Ctrl Pts',(-5.72993077912015,-194.96175111262,9.92453123332965));
#31785=CARTESIAN_POINT('Ctrl Pts',(1.77096949183774E-11,-194.78675111262,
9.92453123331945));
#31786=CARTESIAN_POINT('Ctrl Pts',(5.72993077915557,-194.61175111262,9.9245312333092));
#31787=CARTESIAN_POINT('Ctrl Pts',(8.5948961687156,-194.43675111262,4.9622656166444));
#31788=CARTESIAN_POINT('Ctrl Pts',(11.4598615582757,-194.26175111262,-2.04690493461015E-11));
#31789=CARTESIAN_POINT('Ctrl Pts',(8.5948961686979,-194.08675111262,-4.96226561667504));
#31790=CARTESIAN_POINT('Ctrl Pts',(5.72993077912012,-193.91175111262,-9.92453123332967));
#31791=CARTESIAN_POINT('Ctrl Pts',(-1.76732204959683E-11,-193.73675111262,
-9.92453123331945));
#31792=CARTESIAN_POINT('Ctrl Pts',(-5.72993077915553,-193.56175111262,-9.92453123330922));
#31793=CARTESIAN_POINT('Ctrl Pts',(-8.59489616871561,-193.38675111262,-4.96226561664437));
#31794=CARTESIAN_POINT('Ctrl Pts',(-11.4598615582757,-193.21175111262,2.04269323109086E-11));
#31795=CARTESIAN_POINT('Ctrl Pts',(-8.59489616869789,-193.03675111262,4.96226561667507));
#31796=CARTESIAN_POINT('Ctrl Pts',(-5.72993077912015,-192.86175111262,9.92453123332965));
#31797=CARTESIAN_POINT('Ctrl Pts',(1.77072641092958E-11,-192.68675111262,
9.92453123331945));
#31798=CARTESIAN_POINT('Ctrl Pts',(5.7299307791555,-192.51175111262,9.92453123330925));
#31799=CARTESIAN_POINT('Ctrl Pts',(8.5948961687156,-192.33675111262,4.9622656166444));
#31800=CARTESIAN_POINT('Ctrl Pts',(11.4598615582757,-192.16175111262,-2.04662424895463E-11));
#31801=CARTESIAN_POINT('Ctrl Pts',(8.59489616869791,-191.98675111262,-4.96226561667504));
#31802=CARTESIAN_POINT('Ctrl Pts',(5.72993077912012,-191.81175111262,-9.92453123332967));
#31803=CARTESIAN_POINT('Ctrl Pts',(-1.76707896868867E-11,-191.63675111262,
-9.92453123331945));
#31804=CARTESIAN_POINT('Ctrl Pts',(-5.72993077915553,-191.46175111262,-9.92453123330923));
#31805=CARTESIAN_POINT('Ctrl Pts',(-8.59489616871561,-191.28675111262,-4.96226561664437));
#31806=CARTESIAN_POINT('Ctrl Pts',(-11.4598615582757,-191.11175111262,2.04241254543534E-11));
#31807=CARTESIAN_POINT('Ctrl Pts',(-8.59489616869789,-190.93675111262,4.96226561667507));
#31808=CARTESIAN_POINT('Ctrl Pts',(-5.72993077912009,-190.76175111262,9.9245312333297));
#31809=CARTESIAN_POINT('Ctrl Pts',(1.76343152644776E-11,-190.58675111262,
9.92453123331945));
#31810=CARTESIAN_POINT('Ctrl Pts',(5.72993077915549,-190.41175111262,9.92453123330925));
#31811=CARTESIAN_POINT('Ctrl Pts',(8.5948961687156,-190.23675111262,4.9622656166444));
#31812=CARTESIAN_POINT('Ctrl Pts',(11.4598615582757,-190.06175111262,-2.04634356329911E-11));
#31813=CARTESIAN_POINT('Ctrl Pts',(8.59489616869787,-189.88675111262,-4.9622656166751));
#31814=CARTESIAN_POINT('Ctrl Pts',(5.72993077912019,-189.71175111262,-9.92453123332963));
#31815=CARTESIAN_POINT('Ctrl Pts',(-1.76683588778051E-11,-189.53675111262,
-9.92453123331945));
#31816=CARTESIAN_POINT('Ctrl Pts',(-5.72993077915553,-189.36175111262,-9.92453123330923));
#31817=CARTESIAN_POINT('Ctrl Pts',(-8.59489616871561,-189.18675111262,-4.96226561664437));
#31818=CARTESIAN_POINT('Ctrl Pts',(-11.4598615582757,-189.01175111262,2.05027458116287E-11));
#31819=CARTESIAN_POINT('Ctrl Pts',(-8.59489616869793,-188.83675111262,4.962265616675));
#31820=CARTESIAN_POINT('Ctrl Pts',(-5.72993077912016,-188.66175111262,9.92453123332965));
#31821=CARTESIAN_POINT('Ctrl Pts',(1.77024024911326E-11,-188.48675111262,
9.92453123331945));
#31822=CARTESIAN_POINT('Ctrl Pts',(5.72993077915556,-188.31175111262,9.92453123330921));
#31823=CARTESIAN_POINT('Ctrl Pts',(8.59489616871556,-188.13675111262,4.96226561664446));
#31824=CARTESIAN_POINT('Ctrl Pts',(11.4598615582757,-187.96175111262,-2.03792015626054E-11));
#31825=CARTESIAN_POINT('Ctrl Pts',(8.59489616869791,-187.78675111262,-4.96226561667503));
#31826=CARTESIAN_POINT('Ctrl Pts',(5.72993077912012,-187.61175111262,-9.92453123332967));
#31827=CARTESIAN_POINT('Ctrl Pts',(-1.77364461044601E-11,-187.43675111262,
-9.92453123331945));
#31828=CARTESIAN_POINT('Ctrl Pts',(-5.72993077915546,-187.26175111262,-9.92453123330927));
#31829=CARTESIAN_POINT('Ctrl Pts',(-8.59489616871558,-187.08675111262,-4.96226561664444));
#31830=CARTESIAN_POINT('Ctrl Pts',(-11.4598615582757,-186.91175111262,2.0418511741243E-11));
#31831=CARTESIAN_POINT('Ctrl Pts',(-8.59489616869789,-186.73675111262,4.96226561667506));
#31832=CARTESIAN_POINT('Ctrl Pts',(-5.72993077912009,-186.56175111262,9.92453123332969));
#31833=CARTESIAN_POINT('Ctrl Pts',(1.76294536463145E-11,-186.38675111262,
9.92453123331945));
#31834=CARTESIAN_POINT('Ctrl Pts',(5.72993077915549,-186.21175111262,9.92453123330925));
#31835=CARTESIAN_POINT('Ctrl Pts',(8.59489616871559,-186.03675111262,4.96226561664441));
#31836=CARTESIAN_POINT('Ctrl Pts',(11.4598615582757,-185.86175111262,-2.04578219198807E-11));
#31837=CARTESIAN_POINT('Ctrl Pts',(8.59489616869787,-185.68675111262,-4.96226561667509));
#31838=CARTESIAN_POINT('Ctrl Pts',(5.7299307791202,-185.51175111262,-9.92453123332963));
#31839=CARTESIAN_POINT('Ctrl Pts',(-1.7663497259642E-11,-185.33675111262,
-9.92453123331945));
#31840=CARTESIAN_POINT('Ctrl Pts',(-5.72993077915552,-185.16175111262,-9.92453123330923));
#31841=CARTESIAN_POINT('Ctrl Pts',(-8.59489616871561,-184.98675111262,-4.96226561664438));
#31842=CARTESIAN_POINT('Ctrl Pts',(-11.4598615582757,-184.81175111262,2.03342776708573E-11));
#31843=CARTESIAN_POINT('Ctrl Pts',(-8.59489616869793,-184.63675111262,4.962265616675));
#31844=CARTESIAN_POINT('Ctrl Pts',(-5.72993077912016,-184.46175111262,9.92453123332965));
#31845=CARTESIAN_POINT('Ctrl Pts',(1.76975408729695E-11,-184.28675111262,
9.92453123331945));
#31846=CARTESIAN_POINT('Ctrl Pts',(5.72993077915556,-184.11175111262,9.92453123330921));
#31847=CARTESIAN_POINT('Ctrl Pts',(8.59489616871556,-183.93675111262,4.96226561664447));
#31848=CARTESIAN_POINT('Ctrl Pts',(11.4598615582757,-183.76175111262,-2.0373587849495E-11));
#31849=CARTESIAN_POINT('Ctrl Pts',(8.59489616869791,-183.58675111262,-4.96226561667503));
#31850=CARTESIAN_POINT('Ctrl Pts',(5.72993077912013,-183.41175111262,-9.92453123332967));
#31851=CARTESIAN_POINT('Ctrl Pts',(-1.7731584486297E-11,-183.23675111262,
-9.92453123331945));
#31852=CARTESIAN_POINT('Ctrl Pts',(-5.72993077915545,-183.06175111262,-9.92453123330927));
#31853=CARTESIAN_POINT('Ctrl Pts',(-8.59489616871557,-182.88675111262,-4.96226561664444));
#31854=CARTESIAN_POINT('Ctrl Pts',(-11.4598615582757,-182.71175111262,2.04128980281326E-11));
#31855=CARTESIAN_POINT('Ctrl Pts',(-8.59489616869789,-182.53675111262,4.96226561667506));
#31856=CARTESIAN_POINT('Ctrl Pts',(-5.72993077912009,-182.36175111262,9.92453123332969));
#31857=CARTESIAN_POINT('Ctrl Pts',(1.76245920281513E-11,-182.18675111262,
9.92453123331945));
#31858=CARTESIAN_POINT('Ctrl Pts',(5.72993077915548,-182.01175111262,9.92453123330925));
#31859=CARTESIAN_POINT('Ctrl Pts',(8.59489616871559,-181.83675111262,4.96226561664441));
#31860=CARTESIAN_POINT('Ctrl Pts',(11.4598615582757,-181.66175111262,-2.04522082067703E-11));
#31861=CARTESIAN_POINT('Ctrl Pts',(8.59489616869794,-181.48675111262,-4.96226561667497));
#31862=CARTESIAN_POINT('Ctrl Pts',(5.7299307791202,-181.31175111262,-9.92453123332963));
#31863=CARTESIAN_POINT('Ctrl Pts',(-1.76586356414788E-11,-181.13675111262,
-9.92453123331945));
#31864=CARTESIAN_POINT('Ctrl Pts',(-5.72993077915552,-180.96175111262,-9.92453123330923));
#31865=CARTESIAN_POINT('Ctrl Pts',(-8.59489616871561,-180.78675111262,-4.96226561664438));
#31866=CARTESIAN_POINT('Ctrl Pts',(-11.4598615582757,-180.61175111262,2.03286639577469E-11));
#31867=CARTESIAN_POINT('Ctrl Pts',(-8.59489616869793,-180.43675111262,4.96226561667499));
#31868=CARTESIAN_POINT('Ctrl Pts',(-5.72993077912017,-180.26175111262,9.92453123332965));
#31869=CARTESIAN_POINT('Ctrl Pts',(1.76926792548063E-11,-180.08675111262,
9.92453123331945));
#31870=CARTESIAN_POINT('Ctrl Pts',(5.72993077915555,-179.91175111262,9.92453123330921));
#31871=CARTESIAN_POINT('Ctrl Pts',(8.59489616871555,-179.73675111262,4.96226561664447));
#31872=CARTESIAN_POINT('Ctrl Pts',(11.4598615582757,-179.56175111262,-2.03679741363846E-11));
#31873=CARTESIAN_POINT('Ctrl Pts',(8.59489616869791,-179.38675111262,-4.96226561667503));
#31874=CARTESIAN_POINT('Ctrl Pts',(5.72993077912013,-179.21175111262,-9.92453123332966));
#31875=CARTESIAN_POINT('Ctrl Pts',(-1.77267228681338E-11,-179.03675111262,
-9.92453123331945));
#31876=CARTESIAN_POINT('Ctrl Pts',(-5.72993077915545,-178.86175111262,-9.92453123330928));
#31877=CARTESIAN_POINT('Ctrl Pts',(-8.59489616871557,-178.68675111262,-4.96226561664444));
#31878=CARTESIAN_POINT('Ctrl Pts',(-11.4598615582757,-178.51175111262,2.04072843150222E-11));
#31879=CARTESIAN_POINT('Ctrl Pts',(-8.5948961686979,-178.33675111262,4.96226561667505));
#31880=CARTESIAN_POINT('Ctrl Pts',(-5.72993077912024,-178.16175111262,9.92453123332961));
#31881=CARTESIAN_POINT('Ctrl Pts',(1.76197304099881E-11,-177.98675111262,
9.92453123331945));
#31882=CARTESIAN_POINT('Ctrl Pts',(5.72993077915548,-177.81175111262,9.92453123330926));
#31883=CARTESIAN_POINT('Ctrl Pts',(8.59489616871559,-177.63675111262,4.96226561664442));
#31884=CARTESIAN_POINT('Ctrl Pts',(11.4598615582757,-177.46175111262,-2.04465944936599E-11));
#31885=CARTESIAN_POINT('Ctrl Pts',(8.59489616869795,-177.28675111262,-4.96226561667496));
#31886=CARTESIAN_POINT('Ctrl Pts',(5.72993077912021,-177.11175111262,-9.92453123332962));
#31887=CARTESIAN_POINT('Ctrl Pts',(-1.76537740233156E-11,-176.93675111262,
-9.92453123331945));
#31888=CARTESIAN_POINT('Ctrl Pts',(-5.72993077915551,-176.76175111262,-9.92453123330924));
#31889=CARTESIAN_POINT('Ctrl Pts',(-8.5948961687156,-176.58675111262,-4.96226561664438));
#31890=CARTESIAN_POINT('Ctrl Pts',(-11.4598615582757,-176.41175111262,2.03230502446365E-11));
#31891=CARTESIAN_POINT('Ctrl Pts',(-8.59489616869793,-176.23675111262,4.96226561667499));
#31892=CARTESIAN_POINT('Ctrl Pts',(-5.72993077912017,-176.06175111262,9.92453123332964));
#31893=CARTESIAN_POINT('Ctrl Pts',(1.76878176366431E-11,-175.88675111262,
9.92453123331945));
#31894=CARTESIAN_POINT('Ctrl Pts',(5.72993077915541,-175.71175111262,9.9245312333093));
#31895=CARTESIAN_POINT('Ctrl Pts',(8.59489616871555,-175.53675111262,4.96226561664448));
#31896=CARTESIAN_POINT('Ctrl Pts',(11.4598615582757,-175.36175111262,-2.03623604232742E-11));
#31897=CARTESIAN_POINT('Ctrl Pts',(8.59489616869791,-175.18675111262,-4.96226561667502));
#31898=CARTESIAN_POINT('Ctrl Pts',(5.72993077912014,-175.01175111262,-9.92453123332966));
#31899=CARTESIAN_POINT('Ctrl Pts',(-1.75808251784975E-11,-174.83675111262,
-9.92453123331945));
#31900=CARTESIAN_POINT('Ctrl Pts',(-5.72993077915544,-174.66175111262,-9.92453123330928));
#31901=CARTESIAN_POINT('Ctrl Pts',(-8.59489616871557,-174.48675111262,-4.96226561664445));
#31902=CARTESIAN_POINT('Ctrl Pts',(-11.4598615582757,-174.31175111262,2.04016706019118E-11));
#31903=CARTESIAN_POINT('Ctrl Pts',(-8.5948961686979,-174.13675111262,4.96226561667505));
#31904=CARTESIAN_POINT('Ctrl Pts',(-5.72993077912025,-173.96175111262,9.9245312333296));
#31905=CARTESIAN_POINT('Ctrl Pts',(1.7614868791825E-11,-173.78675111262,
9.92453123331945));
#31906=CARTESIAN_POINT('Ctrl Pts',(5.72993077915548,-173.61175111262,9.92453123330926));
#31907=CARTESIAN_POINT('Ctrl Pts',(8.59489616871558,-173.43675111262,4.96226561664442));
#31908=CARTESIAN_POINT('Ctrl Pts',(11.4598615582757,-173.26175111262,-2.04409807805495E-11));
#31909=CARTESIAN_POINT('Ctrl Pts',(8.59489616869795,-173.08675111262,-4.96226561667496));
#31910=CARTESIAN_POINT('Ctrl Pts',(5.72993077912021,-172.91175111262,-9.92453123332962));
#31911=CARTESIAN_POINT('Ctrl Pts',(-1.76489124051525E-11,-172.73675111262,
-9.92453123331945));
#31912=CARTESIAN_POINT('Ctrl Pts',(-5.72993077915551,-172.56175111262,-9.92453123330924));
#31913=CARTESIAN_POINT('Ctrl Pts',(-8.59489616871553,-172.38675111262,-4.96226561664451));
#31914=CARTESIAN_POINT('Ctrl Pts',(-11.4598615582757,-172.21175111262,2.03174365315261E-11));
#31915=CARTESIAN_POINT('Ctrl Pts',(-8.59489616869793,-172.03675111262,4.96226561667499));
#31916=CARTESIAN_POINT('Ctrl Pts',(-5.72993077912018,-171.86175111262,9.92453123332964));
#31917=CARTESIAN_POINT('Ctrl Pts',(1.768295601848E-11,-171.68675111262,
9.92453123331945));
#31918=CARTESIAN_POINT('Ctrl Pts',(5.7299307791554,-171.51175111262,9.9245312333093));
#31919=CARTESIAN_POINT('Ctrl Pts',(8.59489616871555,-171.33675111262,4.96226561664448));
#31920=CARTESIAN_POINT('Ctrl Pts',(11.4598615582757,-171.16175111262,-2.03567467101638E-11));
#31921=CARTESIAN_POINT('Ctrl Pts',(8.59489616869792,-170.98675111262,-4.96226561667502));
#31922=CARTESIAN_POINT('Ctrl Pts',(5.72993077912014,-170.81175111262,-9.92453123332966));
#31923=CARTESIAN_POINT('Ctrl Pts',(-1.75759635603343E-11,-170.63675111262,
-9.92453123331945));
#31924=CARTESIAN_POINT('Ctrl Pts',(-5.72993077915544,-170.46175111262,-9.92453123330928));
#31925=CARTESIAN_POINT('Ctrl Pts',(-8.59489616871556,-170.28675111262,-4.96226561664445));
#31926=CARTESIAN_POINT('Ctrl Pts',(-11.4598615582757,-170.11175111262,2.03960568888014E-11));
#31927=CARTESIAN_POINT('Ctrl Pts',(-8.5948961686979,-169.93675111262,4.96226561667505));
#31928=CARTESIAN_POINT('Ctrl Pts',(-5.72993077912011,-169.76175111262,9.92453123332968));
#31929=CARTESIAN_POINT('Ctrl Pts',(1.76100071736618E-11,-169.58675111262,
9.92453123331945));
#31930=CARTESIAN_POINT('Ctrl Pts',(5.72993077915533,-169.41175111262,9.92453123330935));
#31931=CARTESIAN_POINT('Ctrl Pts',(8.59489616871558,-169.23675111262,4.96226561664442));
#31932=CARTESIAN_POINT('Ctrl Pts',(11.4598615582757,-169.06175111262,-2.02725126397781E-11));
#31933=CARTESIAN_POINT('Ctrl Pts',(8.59489616869788,-168.88675111262,-4.96226561667507));
#31934=CARTESIAN_POINT('Ctrl Pts',(5.72993077912022,-168.71175111262,-9.92453123332962));
#31935=CARTESIAN_POINT('Ctrl Pts',(-1.75030147155161E-11,-168.53675111262,
-9.92453123331945));
#31936=CARTESIAN_POINT('Ctrl Pts',(-5.7299307791555,-168.36175111262,-9.92453123330924));
#31937=CARTESIAN_POINT('Ctrl Pts',(-8.59489616871553,-168.18675111262,-4.96226561664451));
#31938=CARTESIAN_POINT('Ctrl Pts',(-11.4598615582757,-168.01175111262,2.04746772460767E-11));
#31939=CARTESIAN_POINT('Ctrl Pts',(-8.59489616869794,-167.83675111262,4.96226561667498));
#31940=CARTESIAN_POINT('Ctrl Pts',(-5.72993077912033,-167.66175111262,9.92453123332955));
#31941=CARTESIAN_POINT('Ctrl Pts',(1.76780944003168E-11,-167.48675111262,
9.92453123331945));
#31942=CARTESIAN_POINT('Ctrl Pts',(5.7299307791554,-167.31175111262,9.92453123330931));
#31943=CARTESIAN_POINT('Ctrl Pts',(8.59489616871562,-167.13675111262,4.96226561664436));
#31944=CARTESIAN_POINT('Ctrl Pts',(11.4598615582757,-166.96175111262,-2.03511329970534E-11));
#31945=CARTESIAN_POINT('Ctrl Pts',(8.59489616869799,-166.78675111262,-4.96226561667489));
#31946=CARTESIAN_POINT('Ctrl Pts',(5.72993077912015,-166.61175111262,-9.92453123332966));
#31947=CARTESIAN_POINT('Ctrl Pts',(-1.75711019421711E-11,-166.43675111262,
-9.92453123331945));
#31948=CARTESIAN_POINT('Ctrl Pts',(-5.72993077915557,-166.26175111262,-9.9245312333092));
#31949=CARTESIAN_POINT('Ctrl Pts',(-8.59489616871556,-166.08675111262,-4.96226561664446));
#31950=CARTESIAN_POINT('Ctrl Pts',(-11.4598615582757,-165.91175111262,2.022758874803E-11));
#31951=CARTESIAN_POINT('Ctrl Pts',(-8.5948961686979,-165.73675111262,4.96226561667504));
#31952=CARTESIAN_POINT('Ctrl Pts',(-5.72993077912025,-165.56175111262,9.9245312333296));
#31953=CARTESIAN_POINT('Ctrl Pts',(1.77461816269718E-11,-165.38675111262,
9.92453123331945));
#31954=CARTESIAN_POINT('Ctrl Pts',(5.72993077915547,-165.21175111262,9.92453123330927));
#31955=CARTESIAN_POINT('Ctrl Pts',(8.59489616871551,-165.03675111262,4.96226561664455));
#31956=CARTESIAN_POINT('Ctrl Pts',(11.4598615582757,-164.86175111262,-2.04297533543287E-11));
#31957=CARTESIAN_POINT('Ctrl Pts',(8.59489616869796,-164.68675111262,-4.96226561667495));
#31958=CARTESIAN_POINT('Ctrl Pts',(5.72993077912036,-164.51175111262,-9.92453123332954));
#31959=CARTESIAN_POINT('Ctrl Pts',(-1.76391891688261E-11,-164.33675111262,
-9.92453123331945));
#31960=CARTESIAN_POINT('Ctrl Pts',(-5.72993077915536,-164.16175111262,-9.92453123330933));
#31961=CARTESIAN_POINT('Ctrl Pts',(-8.5948961687156,-163.98675111262,-4.9622656166444));
#31962=CARTESIAN_POINT('Ctrl Pts',(-11.4598615582757,-163.81175111262,2.03062091053053E-11));
#31963=CARTESIAN_POINT('Ctrl Pts',(-8.59489616869801,-163.63675111262,4.96226561667486));
#31964=CARTESIAN_POINT('Ctrl Pts',(-5.72993077912019,-163.46175111262,9.92453123332963));
#31965=CARTESIAN_POINT('Ctrl Pts',(1.75321967106804E-11,-163.28675111262,
9.92453123331945));
#31966=CARTESIAN_POINT('Ctrl Pts',(5.72993077915553,-163.11175111262,9.92453123330922));
#31967=CARTESIAN_POINT('Ctrl Pts',(8.59489616871554,-162.93675111262,4.96226561664449));
#31968=CARTESIAN_POINT('Ctrl Pts',(11.4598615582757,-162.76175111262,-2.0182664856282E-11));
#31969=CARTESIAN_POINT('Ctrl Pts',(8.59489616869792,-162.58675111262,-4.96226561667501));
#31970=CARTESIAN_POINT('Ctrl Pts',(5.7299307791203,-162.41175111262,-9.92453123332957));
#31971=CARTESIAN_POINT('Ctrl Pts',(-1.77072763954811E-11,-162.23675111262,
-9.92453123331945));
#31972=CARTESIAN_POINT('Ctrl Pts',(-5.72993077915543,-162.06175111262,-9.92453123330929));
#31973=CARTESIAN_POINT('Ctrl Pts',(-8.59489616871549,-161.88675111262,-4.96226561664458));
#31974=CARTESIAN_POINT('Ctrl Pts',(-11.4598615582757,-161.71175111262,2.03848294625806E-11));
#31975=CARTESIAN_POINT('Ctrl Pts',(-8.59489616869798,-161.53675111262,4.96226561667492));
#31976=CARTESIAN_POINT('Ctrl Pts',(-5.72993077912012,-161.36175111262,9.92453123332967));
#31977=CARTESIAN_POINT('Ctrl Pts',(1.76002839373354E-11,-161.18675111262,
9.92453123331945));
#31978=CARTESIAN_POINT('Ctrl Pts',(5.72993077915532,-161.01175111262,9.92453123330935));
#31979=CARTESIAN_POINT('Ctrl Pts',(8.59489616871558,-160.83675111262,4.96226561664443));
#31980=CARTESIAN_POINT('Ctrl Pts',(11.4598615582757,-160.66175111262,-2.02612852135573E-11));
#31981=CARTESIAN_POINT('Ctrl Pts',(8.59489616869789,-160.48675111262,-4.96226561667507));
#31982=CARTESIAN_POINT('Ctrl Pts',(5.72993077912023,-160.31175111262,-9.92453123332961));
#31983=CARTESIAN_POINT('Ctrl Pts',(-1.74932914791898E-11,-160.13675111262,
-9.92453123331945));
#31984=CARTESIAN_POINT('Ctrl Pts',(-5.72993077915549,-159.96175111262,-9.92453123330925));
#31985=CARTESIAN_POINT('Ctrl Pts',(-8.59489616871553,-159.78675111262,-4.96226561664452));
#31986=CARTESIAN_POINT('Ctrl Pts',(-11.4598615582757,-159.61175111262,2.04634498198559E-11));
#31987=CARTESIAN_POINT('Ctrl Pts',(-8.59489616869794,-159.43675111262,4.96226561667497));
#31988=CARTESIAN_POINT('Ctrl Pts',(-5.72993077912033,-159.26175111262,9.92453123332955));
#31989=CARTESIAN_POINT('Ctrl Pts',(1.76683711639905E-11,-159.08675111262,
9.92453123331945));
#31990=CARTESIAN_POINT('Ctrl Pts',(5.72993077915539,-158.91175111262,9.92453123330931));
#31991=CARTESIAN_POINT('Ctrl Pts',(8.59489616871561,-158.73675111262,4.96226561664437));
#31992=CARTESIAN_POINT('Ctrl Pts',(11.4598615582757,-158.56175111262,-2.03399055708326E-11));
#31993=CARTESIAN_POINT('Ctrl Pts',(8.594896168698,-158.38675111262,-4.96226561667488));
#31994=CARTESIAN_POINT('Ctrl Pts',(5.72993077912016,-158.21175111262,-9.92453123332965));
#31995=CARTESIAN_POINT('Ctrl Pts',(-1.75613787058448E-11,-158.03675111262,
-9.92453123331945));
#31996=CARTESIAN_POINT('Ctrl Pts',(-5.72993077915528,-157.86175111262,-9.92453123330937));
#31997=CARTESIAN_POINT('Ctrl Pts',(-8.59489616871556,-157.68675111262,-4.96226561664446));
#31998=CARTESIAN_POINT('Ctrl Pts',(-11.4598615582757,-157.51175111262,2.02163613218092E-11));
#31999=CARTESIAN_POINT('Ctrl Pts',(-8.59489616869791,-157.33675111262,4.96226561667503));
#32000=CARTESIAN_POINT('Ctrl Pts',(-5.72993077912026,-157.16175111262,9.92453123332959));
#32001=CARTESIAN_POINT('Ctrl Pts',(1.74543862476991E-11,-156.98675111262,
9.92453123331945));
#32002=CARTESIAN_POINT('Ctrl Pts',(5.72993077915546,-156.81175111262,9.92453123330927));
#32003=CARTESIAN_POINT('Ctrl Pts',(8.5948961687155,-156.63675111262,4.96226561664456));
#32004=CARTESIAN_POINT('Ctrl Pts',(11.4598615582757,-156.46175111262,-2.04185259281078E-11));
#32005=CARTESIAN_POINT('Ctrl Pts',(8.59489616869796,-156.28675111262,-4.96226561667494));
#32006=CARTESIAN_POINT('Ctrl Pts',(5.72993077912037,-156.11175111262,-9.92453123332953));
#32007=CARTESIAN_POINT('Ctrl Pts',(-1.76294659324998E-11,-155.93675111262,
-9.92453123331945));
#32008=CARTESIAN_POINT('Ctrl Pts',(-5.72993077915535,-155.76175111262,-9.92453123330933));
#32009=CARTESIAN_POINT('Ctrl Pts',(-8.59489616871559,-155.58675111262,-4.96226561664441));
#32010=CARTESIAN_POINT('Ctrl Pts',(-11.4598615582757,-155.41175111262,2.02949816790845E-11));
#32011=CARTESIAN_POINT('Ctrl Pts',(-8.59489616869802,-155.23675111262,4.96226561667485));
#32012=CARTESIAN_POINT('Ctrl Pts',(-5.7299307791202,-155.06175111262,9.92453123332963));
#32013=CARTESIAN_POINT('Ctrl Pts',(1.75224734743541E-11,-154.88675111262,
9.92453123331945));
#32014=CARTESIAN_POINT('Ctrl Pts',(5.72993077915552,-154.71175111262,9.92453123330923));
#32015=CARTESIAN_POINT('Ctrl Pts',(8.59489616871554,-154.53675111262,4.9622656166445));
#32016=CARTESIAN_POINT('Ctrl Pts',(11.4598615582757,-154.36175111262,-2.01714374300612E-11));
#32017=CARTESIAN_POINT('Ctrl Pts',(8.59489616869793,-154.18675111262,-4.962265616675));
#32018=CARTESIAN_POINT('Ctrl Pts',(5.7299307791203,-154.01175111262,-9.92453123332957));
#32019=CARTESIAN_POINT('Ctrl Pts',(-1.76975531591548E-11,-153.83675111262,
-9.92453123331945));
#32020=CARTESIAN_POINT('Ctrl Pts',(-5.72993077915542,-153.66175111262,-9.92453123330929));
#32021=CARTESIAN_POINT('Ctrl Pts',(-8.59489616871549,-153.48675111262,-4.96226561664459));
#32022=CARTESIAN_POINT('Ctrl Pts',(-11.4598615582757,-153.31175111262,2.03736020363598E-11));
#32023=CARTESIAN_POINT('Ctrl Pts',(-8.59489616869798,-153.13675111262,4.96226561667491));
#32024=CARTESIAN_POINT('Ctrl Pts',(-5.72993077912013,-152.96175111262,9.92453123332967));
#32025=CARTESIAN_POINT('Ctrl Pts',(1.75905607010091E-11,-152.78675111262,
9.92453123331945));
#32026=CARTESIAN_POINT('Ctrl Pts',(5.72993077915531,-152.61175111262,9.92453123330936));
#32027=CARTESIAN_POINT('Ctrl Pts',(8.59489616871557,-152.43675111262,4.96226561664444));
#32028=CARTESIAN_POINT('Ctrl Pts',(11.4598615582757,-152.26175111262,-2.02500577873365E-11));
#32029=CARTESIAN_POINT('Ctrl Pts',(8.59489616869789,-152.08675111262,-4.96226561667506));
#32030=CARTESIAN_POINT('Ctrl Pts',(5.72993077912024,-151.91175111262,-9.92453123332961));
#32031=CARTESIAN_POINT('Ctrl Pts',(-1.74835682428634E-11,-151.73675111262,
-9.92453123331945));
#32032=CARTESIAN_POINT('Ctrl Pts',(-5.72993077915548,-151.56175111262,-9.92453123330925));
#32033=CARTESIAN_POINT('Ctrl Pts',(-8.59489616871552,-151.38675111262,-4.96226561664453));
#32034=CARTESIAN_POINT('Ctrl Pts',(-11.4598615582757,-151.21175111262,2.01265135383131E-11));
#32035=CARTESIAN_POINT('Ctrl Pts',(-8.59489616869794,-151.03675111262,4.96226561667497));
#32036=CARTESIAN_POINT('Ctrl Pts',(-5.72993077912034,-150.86175111262,9.92453123332955));
#32037=CARTESIAN_POINT('Ctrl Pts',(1.76586479276641E-11,-150.68675111262,
9.92453123331945));
#32038=CARTESIAN_POINT('Ctrl Pts',(5.72993077915538,-150.51175111262,9.92453123330931));
#32039=CARTESIAN_POINT('Ctrl Pts',(8.59489616871547,-150.33675111262,4.96226561664462));
#32040=CARTESIAN_POINT('Ctrl Pts',(11.4598615582757,-150.16175111262,-2.03286781446117E-11));
#32041=CARTESIAN_POINT('Ctrl Pts',(8.594896168698,-149.98675111262,-4.96226561667487));
#32042=CARTESIAN_POINT('Ctrl Pts',(5.72993077912017,-149.81175111262,-9.92453123332965));
#32043=CARTESIAN_POINT('Ctrl Pts',(-1.75516554695184E-11,-149.63675111262,
-9.92453123331945));
#32044=CARTESIAN_POINT('Ctrl Pts',(-5.72993077915527,-149.46175111262,-9.92453123330938));
#32045=CARTESIAN_POINT('Ctrl Pts',(-8.59489616871555,-149.28675111262,-4.96226561664447));
#32046=CARTESIAN_POINT('Ctrl Pts',(-11.4598615582757,-149.11175111262,2.02051338955884E-11));
#32047=CARTESIAN_POINT('Ctrl Pts',(-8.59489616869791,-148.93675111262,4.96226561667503));
#32048=CARTESIAN_POINT('Ctrl Pts',(-5.72993077912027,-148.76175111262,9.92453123332958));
#32049=CARTESIAN_POINT('Ctrl Pts',(1.74446630113728E-11,-148.58675111262,
9.92453123331945));
#32050=CARTESIAN_POINT('Ctrl Pts',(5.72993077915545,-148.41175111262,9.92453123330928));
#32051=CARTESIAN_POINT('Ctrl Pts',(8.5948961687155,-148.23675111262,4.96226561664457));
#32052=CARTESIAN_POINT('Ctrl Pts',(11.4598615582757,-148.06175111262,-2.0407298501887E-11));
#32053=CARTESIAN_POINT('Ctrl Pts',(8.59489616869797,-147.88675111262,-4.96226561667493));
#32054=CARTESIAN_POINT('Ctrl Pts',(5.72993077912038,-147.71175111262,-9.92453123332952));
#32055=CARTESIAN_POINT('Ctrl Pts',(-1.76197426961734E-11,-147.53675111262,
-9.92453123331945));
#32056=CARTESIAN_POINT('Ctrl Pts',(-5.72993077915534,-147.36175111262,-9.92453123330934));
#32057=CARTESIAN_POINT('Ctrl Pts',(-8.59489616871559,-147.18675111262,-4.96226561664442));
#32058=CARTESIAN_POINT('Ctrl Pts',(-11.4598615582757,-147.01175111262,2.02837542528637E-11));
#32059=CARTESIAN_POINT('Ctrl Pts',(-8.59489616869802,-146.83675111262,4.96226561667484));
#32060=CARTESIAN_POINT('Ctrl Pts',(-5.72993077912021,-146.66175111262,9.92453123332962));
#32061=CARTESIAN_POINT('Ctrl Pts',(1.75127502380278E-11,-146.48675111262,
9.92453123331945));
#32062=CARTESIAN_POINT('Ctrl Pts',(5.72993077915551,-146.31175111262,9.92453123330924));
#32063=CARTESIAN_POINT('Ctrl Pts',(8.59489616871553,-146.13675111262,4.96226561664451));
#32064=CARTESIAN_POINT('Ctrl Pts',(11.4598615582757,-145.96175111262,-2.01602100038404E-11));
#32065=CARTESIAN_POINT('Ctrl Pts',(8.59489616869793,-145.78675111262,-4.96226561667499));
#32066=CARTESIAN_POINT('Ctrl Pts',(5.72993077912031,-145.61175111262,-9.92453123332956));
#32067=CARTESIAN_POINT('Ctrl Pts',(-1.76878299228285E-11,-145.43675111262,
-9.92453123331945));
#32068=CARTESIAN_POINT('Ctrl Pts',(-5.72993077915541,-145.26175111262,-9.9245312333093));
#32069=CARTESIAN_POINT('Ctrl Pts',(-8.59489616871548,-145.08675111262,-4.9622656166446));
#32070=CARTESIAN_POINT('Ctrl Pts',(-11.4598615582757,-144.91175111262,2.0362374610139E-11));
#32071=CARTESIAN_POINT('Ctrl Pts',(-8.59489616869799,-144.73675111262,4.9622656166749));
#32072=CARTESIAN_POINT('Ctrl Pts',(-5.72993077912042,-144.56175111262,9.9245312333295));
#32073=CARTESIAN_POINT('Ctrl Pts',(1.75808374646828E-11,-144.38675111262,
9.92453123331945));
#32074=CARTESIAN_POINT('Ctrl Pts',(5.7299307791553,-144.21175111262,9.92453123330936));
#32075=CARTESIAN_POINT('Ctrl Pts',(8.59489616871557,-144.03675111262,4.96226561664445));
#32076=CARTESIAN_POINT('Ctrl Pts',(11.4598615582757,-143.86175111262,-2.02388303611156E-11));
#32077=CARTESIAN_POINT('Ctrl Pts',(8.59489616869804,-143.68675111262,-4.96226561667481));
#32078=CARTESIAN_POINT('Ctrl Pts',(5.72993077912025,-143.51175111262,-9.9245312333296));
#32079=CARTESIAN_POINT('Ctrl Pts',(-1.74738450065371E-11,-143.33675111262,
-9.92453123331945));
#32080=CARTESIAN_POINT('Ctrl Pts',(-5.72993077915548,-143.16175111262,-9.92453123330926));
#32081=CARTESIAN_POINT('Ctrl Pts',(-8.59489616871551,-142.98675111262,-4.96226561664454));
#32082=CARTESIAN_POINT('Ctrl Pts',(-11.4598615582757,-142.81175111262,2.01152861120923E-11));
#32083=CARTESIAN_POINT('Ctrl Pts',(-8.59489616869795,-142.63675111262,4.96226561667496));
#32084=CARTESIAN_POINT('Ctrl Pts',(-5.72993077912035,-142.46175111262,9.92453123332954));
#32085=CARTESIAN_POINT('Ctrl Pts',(1.76489246913378E-11,-142.28675111262,
9.92453123331945));
#32086=CARTESIAN_POINT('Ctrl Pts',(5.72993077915537,-142.11175111262,9.92453123330932));
#32087=CARTESIAN_POINT('Ctrl Pts',(8.59489616871546,-141.93675111262,4.96226561664463));
#32088=CARTESIAN_POINT('Ctrl Pts',(11.4598615582757,-141.76175111262,-2.03174507183909E-11));
#32089=CARTESIAN_POINT('Ctrl Pts',(8.59489616869801,-141.58675111262,-4.96226561667487));
#32090=CARTESIAN_POINT('Ctrl Pts',(5.72993077912018,-141.41175111262,-9.92453123332964));
#32091=CARTESIAN_POINT('Ctrl Pts',(-1.75419322331921E-11,-141.23675111262,
-9.92453123331945));
#32092=CARTESIAN_POINT('Ctrl Pts',(-5.72993077915526,-141.06175111262,-9.92453123330938));
#32093=CARTESIAN_POINT('Ctrl Pts',(-8.59489616871555,-140.88675111262,-4.96226561664448));
#32094=CARTESIAN_POINT('Ctrl Pts',(-11.4598615582757,-140.71175111262,2.01939064693676E-11));
#32095=CARTESIAN_POINT('Ctrl Pts',(-8.59489616869792,-140.53675111262,4.96226561667502));
#32096=CARTESIAN_POINT('Ctrl Pts',(-5.72993077912029,-140.36175111262,9.92453123332958));
#32097=CARTESIAN_POINT('Ctrl Pts',(1.74349397750464E-11,-140.18675111262,
9.92453123331945));
#32098=CARTESIAN_POINT('Ctrl Pts',(5.72993077915544,-140.01175111262,9.92453123330928));
#32099=CARTESIAN_POINT('Ctrl Pts',(8.59489616871549,-139.83675111262,4.96226561664457));
#32100=CARTESIAN_POINT('Ctrl Pts',(11.4598615582757,-139.66175111262,-2.03960710756662E-11));
#32101=CARTESIAN_POINT('Ctrl Pts',(8.59489616869797,-139.48675111262,-4.96226561667492));
#32102=CARTESIAN_POINT('Ctrl Pts',(5.72993077912039,-139.31175111262,-9.92453123332952));
#32103=CARTESIAN_POINT('Ctrl Pts',(-1.76100194598471E-11,-139.13675111262,
-9.92453123331945));
#32104=CARTESIAN_POINT('Ctrl Pts',(-5.72993077915533,-138.96175111262,-9.92453123330935));
#32105=CARTESIAN_POINT('Ctrl Pts',(-8.59489616871544,-138.78675111262,-4.96226561664467));
#32106=CARTESIAN_POINT('Ctrl Pts',(-11.4598615582757,-138.61175111262,2.02725268266429E-11));
#32107=CARTESIAN_POINT('Ctrl Pts',(-8.59489616869802,-138.43675111262,4.96226561667483));
#32108=CARTESIAN_POINT('Ctrl Pts',(-5.72993077912022,-138.26175111262,9.92453123332962));
#32109=CARTESIAN_POINT('Ctrl Pts',(1.75030270017014E-11,-138.08675111262,
9.92453123331945));
#32110=CARTESIAN_POINT('Ctrl Pts',(5.72993077915522,-137.91175111262,9.92453123330941));
#32111=CARTESIAN_POINT('Ctrl Pts',(8.59489616871553,-137.73675111262,4.96226561664451));
#32112=CARTESIAN_POINT('Ctrl Pts',(11.4598615582757,-137.56175111262,-2.01489825776195E-11));
#32113=CARTESIAN_POINT('Ctrl Pts',(8.59489616869794,-137.38675111262,-4.96226561667498));
#32114=CARTESIAN_POINT('Ctrl Pts',(5.72993077912033,-137.21175111262,-9.92453123332955));
#32115=CARTESIAN_POINT('Ctrl Pts',(-1.73960345435557E-11,-137.03675111262,
-9.92453123331945));
#32116=CARTESIAN_POINT('Ctrl Pts',(-5.7299307791554,-136.86175111262,-9.92453123330931));
#32117=CARTESIAN_POINT('Ctrl Pts',(-8.59489616871548,-136.68675111262,-4.96226561664461));
#32118=CARTESIAN_POINT('Ctrl Pts',(-11.4598615582757,-136.51175111262,2.03511471839182E-11));
#32119=CARTESIAN_POINT('Ctrl Pts',(-8.59489616869799,-136.33675111262,4.96226561667489));
#32120=CARTESIAN_POINT('Ctrl Pts',(-5.72993077912043,-136.16175111262,9.92453123332949));
#32121=CARTESIAN_POINT('Ctrl Pts',(1.75711142283564E-11,-135.98675111262,
9.92453123331945));
#32122=CARTESIAN_POINT('Ctrl Pts',(5.72993077915529,-135.81175111262,9.92453123330937));
#32123=CARTESIAN_POINT('Ctrl Pts',(8.59489616871556,-135.63675111262,4.96226561664446));
#32124=CARTESIAN_POINT('Ctrl Pts',(11.4598615582757,-135.46175111262,-2.02276029348948E-11));
#32125=CARTESIAN_POINT('Ctrl Pts',(8.59489616869805,-135.28675111262,-4.9622656166748));
#32126=CARTESIAN_POINT('Ctrl Pts',(5.72993077912025,-135.11175111262,-9.9245312333296));
#32127=CARTESIAN_POINT('Ctrl Pts',(-1.74641217702107E-11,-134.93675111262,
-9.92453123331945));
#32128=CARTESIAN_POINT('Ctrl Pts',(-5.72993077915547,-134.76175111262,-9.92453123330927));
#32129=CARTESIAN_POINT('Ctrl Pts',(-8.59489616871551,-134.58675111262,-4.96226561664455));
#32130=CARTESIAN_POINT('Ctrl Pts',(-11.4598615582757,-134.41175111262,2.01040586858715E-11));
#32131=CARTESIAN_POINT('Ctrl Pts',(-8.59489616869796,-134.23675111262,4.96226561667495));
#32132=CARTESIAN_POINT('Ctrl Pts',(-5.72993077912036,-134.06175111262,9.92453123332954));
#32133=CARTESIAN_POINT('Ctrl Pts',(1.76392014550114E-11,-133.88675111262,
9.92453123331945));
#32134=CARTESIAN_POINT('Ctrl Pts',(5.72993077915536,-133.71175111262,9.92453123330933));
#32135=CARTESIAN_POINT('Ctrl Pts',(8.59489616871546,-133.53675111262,4.96226561664464));
#32136=CARTESIAN_POINT('Ctrl Pts',(11.4598615582757,-133.36175111262,-2.03062232921701E-11));
#32137=CARTESIAN_POINT('Ctrl Pts',(8.59489616869801,-133.18675111262,-4.96226561667486));
#32138=CARTESIAN_POINT('Ctrl Pts',(5.72993077912019,-133.01175111262,-9.92453123332963));
#32139=CARTESIAN_POINT('Ctrl Pts',(-1.75322089968658E-11,-132.83675111262,
-9.92453123331945));
#32140=CARTESIAN_POINT('Ctrl Pts',(-5.72993077915525,-132.66175111262,-9.92453123330939));
#32141=CARTESIAN_POINT('Ctrl Pts',(-8.59489616871554,-132.48675111262,-4.96226561664449));
#32142=CARTESIAN_POINT('Ctrl Pts',(-11.4598615582757,-132.31175111262,2.01826790431468E-11));
#32143=CARTESIAN_POINT('Ctrl Pts',(-8.59489616869806,-132.13675111262,4.96226561667476));
#32144=CARTESIAN_POINT('Ctrl Pts',(-5.7299307791203,-131.96175111262,9.92453123332957));
#32145=CARTESIAN_POINT('Ctrl Pts',(1.74252165387201E-11,-131.78675111262,
9.92453123331945));
#32146=CARTESIAN_POINT('Ctrl Pts',(5.72993077915543,-131.61175111262,9.92453123330929));
#32147=CARTESIAN_POINT('Ctrl Pts',(8.59489616871549,-131.43675111262,4.96226561664458));
#32148=CARTESIAN_POINT('Ctrl Pts',(11.4598615582757,-131.26175111262,-2.00591347941234E-11));
#32149=CARTESIAN_POINT('Ctrl Pts',(8.59489616869798,-131.08675111262,-4.96226561667492));
#32150=CARTESIAN_POINT('Ctrl Pts',(5.7299307791204,-130.91175111262,-9.92453123332951));
#32151=CARTESIAN_POINT('Ctrl Pts',(-1.76002962235208E-11,-130.73675111262,
-9.92453123331945));
#32152=CARTESIAN_POINT('Ctrl Pts',(-5.72993077915532,-130.56175111262,-9.92453123330935));
#32153=CARTESIAN_POINT('Ctrl Pts',(-8.59489616871544,-130.38675111262,-4.96226561664468));
#32154=CARTESIAN_POINT('Ctrl Pts',(-11.4598615582757,-130.21175111262,2.02612994004221E-11));
#32155=CARTESIAN_POINT('Ctrl Pts',(-8.59489616869803,-130.03675111262,4.96226561667482));
#32156=CARTESIAN_POINT('Ctrl Pts',(-5.72993077912023,-129.86175111262,9.92453123332961));
#32157=CARTESIAN_POINT('Ctrl Pts',(1.74933037653751E-11,-129.68675111262,
9.92453123331945));
#32158=CARTESIAN_POINT('Ctrl Pts',(5.72993077915521,-129.51175111262,9.92453123330941));
#32159=CARTESIAN_POINT('Ctrl Pts',(8.59489616871553,-129.33675111262,4.96226561664452));
#32160=CARTESIAN_POINT('Ctrl Pts',(11.4598615582757,-129.16175111262,-2.01377551513987E-11));
#32161=CARTESIAN_POINT('Ctrl Pts',(8.59489616869794,-128.98675111262,-4.96226561667497));
#32162=CARTESIAN_POINT('Ctrl Pts',(5.72993077912033,-128.81175111262,-9.92453123332955));
#32163=CARTESIAN_POINT('Ctrl Pts',(-1.73863113072294E-11,-128.63675111262,
-9.92453123331945));
#32164=CARTESIAN_POINT('Ctrl Pts',(-5.72993077915539,-128.46175111262,-9.92453123330931));
#32165=CARTESIAN_POINT('Ctrl Pts',(-8.59489616871547,-128.28675111262,-4.96226561664462));
#32166=CARTESIAN_POINT('Ctrl Pts',(-11.4598615582757,-128.11175111262,2.03399197576974E-11));
#32167=CARTESIAN_POINT('Ctrl Pts',(-8.59489616869799,-127.93675111262,4.96226561667488));
#32168=CARTESIAN_POINT('Ctrl Pts',(-5.72993077912044,-127.76175111262,9.92453123332949));
#32169=CARTESIAN_POINT('Ctrl Pts',(1.75613909920301E-11,-127.58675111262,
9.92453123331945));
#32170=CARTESIAN_POINT('Ctrl Pts',(5.72993077915528,-127.41175111262,9.92453123330937));
#32171=CARTESIAN_POINT('Ctrl Pts',(8.59489616871556,-127.23675111262,4.96226561664446));
#32172=CARTESIAN_POINT('Ctrl Pts',(11.4598615582757,-127.06175111262,-2.0216375508674E-11));
#32173=CARTESIAN_POINT('Ctrl Pts',(8.59489616869791,-126.88675111262,-4.96226561667503));
#32174=CARTESIAN_POINT('Ctrl Pts',(5.72993077912055,-126.71175111262,-9.92453123332943));
#32175=CARTESIAN_POINT('Ctrl Pts',(-1.74543985338844E-11,-126.53675111262,
-9.92453123331945));
#32176=CARTESIAN_POINT('Ctrl Pts',(-5.72993077915546,-126.36175111262,-9.92453123330927));
#32177=CARTESIAN_POINT('Ctrl Pts',(-8.59489616871537,-126.18675111262,-4.9622656166448));
#32178=CARTESIAN_POINT('Ctrl Pts',(-11.4598615582757,-126.01175111262,2.00928312596507E-11));
#32179=CARTESIAN_POINT('Ctrl Pts',(-8.59489616869796,-125.83675111262,4.96226561667494));
#32180=CARTESIAN_POINT('Ctrl Pts',(-5.72993077912009,-125.66175111262,9.92453123332969));
#32181=CARTESIAN_POINT('Ctrl Pts',(1.73474060757387E-11,-125.48675111262,
9.92453123331945));
#32182=CARTESIAN_POINT('Ctrl Pts',(5.72993077915535,-125.31175111262,9.92453123330933));
#32183=CARTESIAN_POINT('Ctrl Pts',(8.59489616871559,-125.13675111262,4.96226561664441));
#32184=CARTESIAN_POINT('Ctrl Pts',(11.4598615582757,-124.96175111262,-1.99692870106273E-11));
#32185=CARTESIAN_POINT('Ctrl Pts',(8.59489616869802,-124.78675111262,-4.96226561667485));
#32186=CARTESIAN_POINT('Ctrl Pts',(5.7299307791202,-124.61175111262,-9.92453123332963));
#32187=CARTESIAN_POINT('Ctrl Pts',(-1.7240413617593E-11,-124.43675111262,
-9.92453123331945));
#32188=CARTESIAN_POINT('Ctrl Pts',(-5.72993077915524,-124.26175111262,-9.92453123330939));
#32189=CARTESIAN_POINT('Ctrl Pts',(-8.59489616871554,-124.08675111262,-4.9622656166445));
#32190=CARTESIAN_POINT('Ctrl Pts',(-11.4598615582757,-123.91175111262,2.04971604722479E-11));
#32191=CARTESIAN_POINT('Ctrl Pts',(-8.59489616869807,-123.73675111262,4.96226561667476));
#32192=CARTESIAN_POINT('Ctrl Pts',(-5.7299307791203,-123.56175111262,9.92453123332957));
#32193=CARTESIAN_POINT('Ctrl Pts',(1.76975654453401E-11,-123.38675111262,
9.92453123331945));
#32194=CARTESIAN_POINT('Ctrl Pts',(5.72993077915513,-123.21175111262,9.92453123330946));
#32195=CARTESIAN_POINT('Ctrl Pts',(8.59489616871549,-123.03675111262,4.96226561664459));
#32196=CARTESIAN_POINT('Ctrl Pts',(11.4598615582757,-122.86175111262,-2.03736162232246E-11));
#32197=CARTESIAN_POINT('Ctrl Pts',(8.59489616869812,-122.68675111262,-4.96226561667466));
#32198=CARTESIAN_POINT('Ctrl Pts',(5.72993077912041,-122.51175111262,-9.92453123332951));
#32199=CARTESIAN_POINT('Ctrl Pts',(-1.75905729871944E-11,-122.33675111262,
-9.92453123331945));
#32200=CARTESIAN_POINT('Ctrl Pts',(-5.72993077915503,-122.16175111262,-9.92453123330952));
#32201=CARTESIAN_POINT('Ctrl Pts',(-8.59489616871543,-121.98675111262,-4.96226561664468));
#32202=CARTESIAN_POINT('Ctrl Pts',(-11.4598615582757,-121.81175111262,2.02500719742013E-11));
#32203=CARTESIAN_POINT('Ctrl Pts',(-8.59489616869789,-121.63675111262,4.96226561667506));
#32204=CARTESIAN_POINT('Ctrl Pts',(-5.72993077912052,-121.46175111262,9.92453123332944));
#32205=CARTESIAN_POINT('Ctrl Pts',(1.74835805290487E-11,-121.28675111262,
9.92453123331945));
#32206=CARTESIAN_POINT('Ctrl Pts',(5.72993077915548,-121.11175111262,9.92453123330925));
#32207=CARTESIAN_POINT('Ctrl Pts',(8.59489616871538,-120.93675111262,4.96226561664478));
#32208=CARTESIAN_POINT('Ctrl Pts',(11.4598615582757,-120.76175111262,-2.01265277251779E-11));
#32209=CARTESIAN_POINT('Ctrl Pts',(8.59489616869794,-120.58675111262,-4.96226561667497));
#32210=CARTESIAN_POINT('Ctrl Pts',(5.72993077912063,-120.41175111262,-9.92453123332938));
#32211=CARTESIAN_POINT('Ctrl Pts',(-1.73765880709031E-11,-120.23675111262,
-9.92453123331945));
#32212=CARTESIAN_POINT('Ctrl Pts',(-5.72993077915538,-120.06175111262,-9.92453123330931));
#32213=CARTESIAN_POINT('Ctrl Pts',(-8.59489616871561,-119.88675111262,-4.96226561664438));
#32214=CARTESIAN_POINT('Ctrl Pts',(-11.4598615582757,-119.71175111262,2.00029834761546E-11));
#32215=CARTESIAN_POINT('Ctrl Pts',(-8.594896168698,-119.53675111262,4.96226561667487));
#32216=CARTESIAN_POINT('Ctrl Pts',(-5.72993077912017,-119.36175111262,9.92453123332965));
#32217=CARTESIAN_POINT('Ctrl Pts',(1.72695956127574E-11,-119.18675111262,
9.92453123331945));
#32218=CARTESIAN_POINT('Ctrl Pts',(5.72993077915527,-119.01175111262,9.92453123330938));
#32219=CARTESIAN_POINT('Ctrl Pts',(8.59489616871555,-118.83675111262,4.96226561664447));
#32220=CARTESIAN_POINT('Ctrl Pts',(11.4598615582757,-118.66175111262,-1.98794392271312E-11));
#32221=CARTESIAN_POINT('Ctrl Pts',(8.59489616869805,-118.48675111262,-4.96226561667478));
#32222=CARTESIAN_POINT('Ctrl Pts',(5.72993077912027,-118.31175111262,-9.92453123332958));
#32223=CARTESIAN_POINT('Ctrl Pts',(-1.77267474405044E-11,-118.13675111262,
-9.92453123331945));
#32224=CARTESIAN_POINT('Ctrl Pts',(-5.72993077915516,-117.96175111262,-9.92453123330944));
#32225=CARTESIAN_POINT('Ctrl Pts',(-8.5948961687155,-117.78675111262,-4.96226561664457));
#32226=CARTESIAN_POINT('Ctrl Pts',(-11.4598615582757,-117.61175111262,2.04073126887518E-11));
#32227=CARTESIAN_POINT('Ctrl Pts',(-8.59489616869811,-117.43675111262,4.96226561667469));
#32228=CARTESIAN_POINT('Ctrl Pts',(-5.72993077912038,-117.26175111262,9.92453123332952));
#32229=CARTESIAN_POINT('Ctrl Pts',(1.76197549823588E-11,-117.08675111262,
9.92453123331945));
#32230=CARTESIAN_POINT('Ctrl Pts',(5.72993077915506,-116.91175111262,9.9245312333095));
#32231=CARTESIAN_POINT('Ctrl Pts',(8.59489616871545,-116.73675111262,4.96226561664466));
#32232=CARTESIAN_POINT('Ctrl Pts',(11.4598615582757,-116.56175111262,-2.02837684397285E-11));
#32233=CARTESIAN_POINT('Ctrl Pts',(8.59489616869816,-116.38675111262,-4.96226561667459));
#32234=CARTESIAN_POINT('Ctrl Pts',(5.72993077912049,-116.21175111262,-9.92453123332946));
#32235=CARTESIAN_POINT('Ctrl Pts',(-1.75127625242131E-11,-116.03675111262,
-9.92453123331945));
#32236=CARTESIAN_POINT('Ctrl Pts',(-5.72993077915551,-115.86175111262,-9.92453123330924));
#32237=CARTESIAN_POINT('Ctrl Pts',(-8.59489616871539,-115.68675111262,-4.96226561664475));
#32238=CARTESIAN_POINT('Ctrl Pts',(-11.4598615582757,-115.51175111262,2.01602241907052E-11));
#32239=CARTESIAN_POINT('Ctrl Pts',(-8.59489616869793,-115.33675111262,4.96226561667499));
#32240=CARTESIAN_POINT('Ctrl Pts',(-5.7299307791206,-115.16175111262,9.9245312333294));
#32241=CARTESIAN_POINT('Ctrl Pts',(1.74057700660674E-11,-114.98675111262,
9.92453123331945));
#32242=CARTESIAN_POINT('Ctrl Pts',(5.72993077915541,-114.81175111262,9.9245312333093));
#32243=CARTESIAN_POINT('Ctrl Pts',(8.59489616871534,-114.63675111262,4.96226561664484));
#32244=CARTESIAN_POINT('Ctrl Pts',(11.4598615582757,-114.46175111262,-2.00366799416818E-11));
#32245=CARTESIAN_POINT('Ctrl Pts',(8.59489616869799,-114.28675111262,-4.9622656166749));
#32246=CARTESIAN_POINT('Ctrl Pts',(5.72993077912014,-114.11175111262,-9.92453123332966));
#32247=CARTESIAN_POINT('Ctrl Pts',(-1.72987776079217E-11,-113.93675111262,
-9.92453123331945));
#32248=CARTESIAN_POINT('Ctrl Pts',(-5.7299307791553,-113.76175111262,-9.92453123330936));
#32249=CARTESIAN_POINT('Ctrl Pts',(-8.59489616871557,-113.58675111262,-4.96226561664445));
#32250=CARTESIAN_POINT('Ctrl Pts',(-11.4598615582757,-113.41175111262,1.99131356926585E-11));
#32251=CARTESIAN_POINT('Ctrl Pts',(-8.59489616869804,-113.23675111262,4.96226561667481));
#32252=CARTESIAN_POINT('Ctrl Pts',(-5.72993077912025,-113.06175111262,9.9245312333296));
#32253=CARTESIAN_POINT('Ctrl Pts',(1.7191785149776E-11,-112.88675111262,
9.92453123331945));
#32254=CARTESIAN_POINT('Ctrl Pts',(5.72993077915519,-112.71175111262,9.92453123330942));
#32255=CARTESIAN_POINT('Ctrl Pts',(8.59489616871551,-112.53675111262,4.96226561664454));
#32256=CARTESIAN_POINT('Ctrl Pts',(11.4598615582757,-112.36175111262,-2.04410091542791E-11));
#32257=CARTESIAN_POINT('Ctrl Pts',(8.59489616869809,-112.18675111262,-4.96226561667471));
#32258=CARTESIAN_POINT('Ctrl Pts',(5.72993077912035,-112.01175111262,-9.92453123332954));
#32259=CARTESIAN_POINT('Ctrl Pts',(-1.76489369775231E-11,-111.83675111262,
-9.92453123331945));
#32260=CARTESIAN_POINT('Ctrl Pts',(-5.72993077915509,-111.66175111262,-9.92453123330948));
#32261=CARTESIAN_POINT('Ctrl Pts',(-8.59489616871546,-111.48675111262,-4.96226561664463));
#32262=CARTESIAN_POINT('Ctrl Pts',(-11.4598615582757,-111.31175111262,2.03174649052557E-11));
#32263=CARTESIAN_POINT('Ctrl Pts',(-8.59489616869815,-111.13675111262,4.96226561667462));
#32264=CARTESIAN_POINT('Ctrl Pts',(-5.72993077912046,-110.96175111262,9.92453123332948));
#32265=CARTESIAN_POINT('Ctrl Pts',(1.75419445193774E-11,-110.78675111262,
9.92453123331945));
#32266=CARTESIAN_POINT('Ctrl Pts',(5.72993077915554,-110.61175111262,9.92453123330922));
#32267=CARTESIAN_POINT('Ctrl Pts',(8.59489616871541,-110.43675111262,4.96226561664473));
#32268=CARTESIAN_POINT('Ctrl Pts',(11.4598615582757,-110.26175111262,-2.01939206562324E-11));
#32269=CARTESIAN_POINT('Ctrl Pts',(8.59489616869792,-110.08675111262,-4.96226561667502));
#32270=CARTESIAN_POINT('Ctrl Pts',(5.72993077912057,-109.91175111262,-9.92453123332941));
#32271=CARTESIAN_POINT('Ctrl Pts',(-1.74349520612317E-11,-109.73675111262,
-9.92453123331945));
#32272=CARTESIAN_POINT('Ctrl Pts',(-5.72993077915544,-109.56175111262,-9.92453123330928));
#32273=CARTESIAN_POINT('Ctrl Pts',(-8.59489616871535,-109.38675111262,-4.96226561664482));
#32274=CARTESIAN_POINT('Ctrl Pts',(-11.4598615582757,-109.21175111262,2.00703764072091E-11));
#32275=CARTESIAN_POINT('Ctrl Pts',(-8.59489616869797,-109.03675111262,4.96226561667492));
#32276=CARTESIAN_POINT('Ctrl Pts',(-5.72993077912067,-108.86175111262,9.92453123332935));
#32277=CARTESIAN_POINT('Ctrl Pts',(1.73279596030861E-11,-108.68675111262,
9.92453123331945));
#32278=CARTESIAN_POINT('Ctrl Pts',(5.72993077915533,-108.51175111262,9.92453123330935));
#32279=CARTESIAN_POINT('Ctrl Pts',(8.59489616871558,-108.33675111262,4.96226561664442));
#32280=CARTESIAN_POINT('Ctrl Pts',(11.4598615582757,-108.16175111262,-1.99468321581857E-11));
#32281=CARTESIAN_POINT('Ctrl Pts',(8.59489616869802,-107.98675111262,-4.96226561667483));
#32282=CARTESIAN_POINT('Ctrl Pts',(5.72993077912022,-107.81175111262,-9.92453123332962));
#32283=CARTESIAN_POINT('Ctrl Pts',(-1.72209671449404E-11,-107.63675111262,
-9.92453123331945));
#32284=CARTESIAN_POINT('Ctrl Pts',(-5.72993077915522,-107.46175111262,-9.92453123330941));
#32285=CARTESIAN_POINT('Ctrl Pts',(-8.59489616871553,-107.28675111262,-4.96226561664451));
#32286=CARTESIAN_POINT('Ctrl Pts',(-11.4598615582757,-107.11175111262,1.98232879091624E-11));
#32287=CARTESIAN_POINT('Ctrl Pts',(-8.59489616869808,-106.93675111262,4.96226561667474));
#32288=CARTESIAN_POINT('Ctrl Pts',(-5.72993077912033,-106.76175111262,9.92453123332955));
#32289=CARTESIAN_POINT('Ctrl Pts',(1.76781189726874E-11,-106.58675111262,
9.92453123331945));
#32290=CARTESIAN_POINT('Ctrl Pts',(5.72993077915512,-106.41175111262,9.92453123330947));
#32291=CARTESIAN_POINT('Ctrl Pts',(8.59489616871548,-106.23675111262,4.96226561664461));
#32292=CARTESIAN_POINT('Ctrl Pts',(11.4598615582757,-106.06175111262,-2.0351161370783E-11));
#32293=CARTESIAN_POINT('Ctrl Pts',(8.59489616869813,-105.88675111262,-4.96226561667465));
#32294=CARTESIAN_POINT('Ctrl Pts',(5.72993077912043,-105.71175111262,-9.92453123332949));
#32295=CARTESIAN_POINT('Ctrl Pts',(-1.75711265145418E-11,-105.53675111262,
-9.92453123331945));
#32296=CARTESIAN_POINT('Ctrl Pts',(-5.72993077915501,-105.36175111262,-9.92453123330953));
#32297=CARTESIAN_POINT('Ctrl Pts',(-8.59489616871542,-105.18675111262,-4.9622656166447));
#32298=CARTESIAN_POINT('Ctrl Pts',(-11.4598615582757,-105.01175111262,2.02276171217596E-11));
#32299=CARTESIAN_POINT('Ctrl Pts',(-8.5948961686979,-104.83675111262,4.96226561667504));
#32300=CARTESIAN_POINT('Ctrl Pts',(-5.72993077912054,-104.66175111262,9.92453123332943));
#32301=CARTESIAN_POINT('Ctrl Pts',(1.74641340563961E-11,-104.48675111262,
9.92453123331945));
#32302=CARTESIAN_POINT('Ctrl Pts',(5.72993077915547,-104.31175111262,9.92453123330927));
#32303=CARTESIAN_POINT('Ctrl Pts',(8.59489616871537,-104.13675111262,4.96226561664479));
#32304=CARTESIAN_POINT('Ctrl Pts',(11.4598615582757,-103.96175111262,-2.01040728727363E-11));
#32305=CARTESIAN_POINT('Ctrl Pts',(8.59489616869796,-103.78675111262,-4.96226561667495));
#32306=CARTESIAN_POINT('Ctrl Pts',(5.72993077912064,-103.61175111262,-9.92453123332937));
#32307=CARTESIAN_POINT('Ctrl Pts',(-1.73571415982504E-11,-103.43675111262,
-9.92453123331945));
#32308=CARTESIAN_POINT('Ctrl Pts',(-5.72993077915536,-103.26175111262,-9.92453123330933));
#32309=CARTESIAN_POINT('Ctrl Pts',(-8.59489616871532,-103.08675111262,-4.96226561664489));
#32310=CARTESIAN_POINT('Ctrl Pts',(-11.4598615582757,-102.91175111262,1.9980528623713E-11));
#32311=CARTESIAN_POINT('Ctrl Pts',(-8.59489616869801,-102.73675111262,4.96226561667486));
#32312=CARTESIAN_POINT('Ctrl Pts',(-5.72993077912019,-102.56175111262,9.92453123332963));
#32313=CARTESIAN_POINT('Ctrl Pts',(1.72501491401047E-11,-102.38675111262,
9.92453123331945));
#32314=CARTESIAN_POINT('Ctrl Pts',(5.72993077915525,-102.21175111262,9.92453123330939));
#32315=CARTESIAN_POINT('Ctrl Pts',(8.59489616871554,-102.03675111262,4.96226561664449));
#32316=CARTESIAN_POINT('Ctrl Pts',(11.4598615582757,-101.86175111262,-1.98569843746896E-11));
#32317=CARTESIAN_POINT('Ctrl Pts',(8.59489616869806,-101.68675111262,-4.96226561667476));
#32318=CARTESIAN_POINT('Ctrl Pts',(5.7299307791203,-101.51175111262,-9.92453123332957));
#32319=CARTESIAN_POINT('Ctrl Pts',(-1.7143156681959E-11,-101.33675111262,
-9.92453123331945));
#32320=CARTESIAN_POINT('Ctrl Pts',(-5.72993077915514,-101.16175111262,-9.92453123330945));
#32321=CARTESIAN_POINT('Ctrl Pts',(-8.59489616871549,-100.98675111262,-4.96226561664458));
#32322=CARTESIAN_POINT('Ctrl Pts',(-11.4598615582757,-100.81175111262,2.03848578363102E-11));
#32323=CARTESIAN_POINT('Ctrl Pts',(-8.59489616869812,-100.63675111262,4.96226561667467));
#32324=CARTESIAN_POINT('Ctrl Pts',(-5.7299307791204,-100.46175111262,9.92453123332951));
#32325=CARTESIAN_POINT('Ctrl Pts',(1.76003085097061E-11,-100.28675111262,
9.92453123331945));
#32326=CARTESIAN_POINT('Ctrl Pts',(5.72993077915504,-100.11175111262,9.92453123330951));
#32327=CARTESIAN_POINT('Ctrl Pts',(8.59489616871544,-99.9367511126202,4.96226561664468));
#32328=CARTESIAN_POINT('Ctrl Pts',(11.4598615582757,-99.7617511126202,-2.02613135872869E-11));
#32329=CARTESIAN_POINT('Ctrl Pts',(8.59489616869817,-99.5867511126202,-4.96226561667458));
#32330=CARTESIAN_POINT('Ctrl Pts',(5.72993077912051,-99.4117511126202,-9.92453123332945));
#32331=CARTESIAN_POINT('Ctrl Pts',(-1.74933160515604E-11,-99.2367511126202,
-9.92453123331945));
#32332=CARTESIAN_POINT('Ctrl Pts',(-5.72993077915549,-99.0617511126202,
-9.92453123330925));
#32333=CARTESIAN_POINT('Ctrl Pts',(-8.59489616871538,-98.8867511126202,
-4.96226561664477));
#32334=CARTESIAN_POINT('Ctrl Pts',(-11.4598615582757,-98.7117511126202,
2.01377693382635E-11));
#32335=CARTESIAN_POINT('Ctrl Pts',(-8.59489616869794,-98.5367511126202,
4.96226561667497));
#32336=CARTESIAN_POINT('Ctrl Pts',(-5.72993077912062,-98.3617511126202,
9.92453123332939));
#32337=CARTESIAN_POINT('Ctrl Pts',(1.73863235934147E-11,-98.1867511126202,
9.92453123331945));
#32338=CARTESIAN_POINT('Ctrl Pts',(5.72993077915539,-98.0117511126202,9.92453123330931));
#32339=CARTESIAN_POINT('Ctrl Pts',(8.59489616871533,-97.8367511126202,4.96226561664486));
#32340=CARTESIAN_POINT('Ctrl Pts',(11.4598615582757,-97.6617511126202,-2.00142250892402E-11));
#32341=CARTESIAN_POINT('Ctrl Pts',(8.59489616869799,-97.4867511126202,-4.96226561667488));
#32342=CARTESIAN_POINT('Ctrl Pts',(5.72993077912072,-97.3117511126202,-9.92453123332933));
#32343=CARTESIAN_POINT('Ctrl Pts',(-1.7279331135269E-11,-97.1367511126202,
-9.92453123331945));
#32344=CARTESIAN_POINT('Ctrl Pts',(-5.72993077915528,-96.9617511126202,
-9.92453123330937));
#32345=CARTESIAN_POINT('Ctrl Pts',(-8.59489616871556,-96.7867511126202,
-4.96226561664446));
#32346=CARTESIAN_POINT('Ctrl Pts',(-11.4598615582757,-96.6117511126202,
1.98906808402169E-11));
#32347=CARTESIAN_POINT('Ctrl Pts',(-8.59489616869805,-96.4367511126202,
4.96226561667479));
#32348=CARTESIAN_POINT('Ctrl Pts',(-5.72993077912026,-96.2617511126202,
9.92453123332959));
#32349=CARTESIAN_POINT('Ctrl Pts',(1.71723386771234E-11,-96.0867511126202,
9.92453123331945));
#32350=CARTESIAN_POINT('Ctrl Pts',(5.72993077915517,-95.9117511126202,9.92453123330943));
#32351=CARTESIAN_POINT('Ctrl Pts',(8.5948961687155,-95.7367511126202,4.96226561664456));
#32352=CARTESIAN_POINT('Ctrl Pts',(11.4598615582757,-95.5617511126202,-1.97671365911935E-11));
#32353=CARTESIAN_POINT('Ctrl Pts',(8.5948961686981,-95.3867511126202,-4.9622656166747));
#32354=CARTESIAN_POINT('Ctrl Pts',(5.72993077912037,-95.2117511126202,-9.92453123332953));
#32355=CARTESIAN_POINT('Ctrl Pts',(-1.76294905048704E-11,-95.0367511126202,
-9.92453123331945));
#32356=CARTESIAN_POINT('Ctrl Pts',(-5.72993077915507,-94.8617511126203,
-9.9245312333095));
#32357=CARTESIAN_POINT('Ctrl Pts',(-8.59489616871545,-94.6867511126202,
-4.96226561664465));
#32358=CARTESIAN_POINT('Ctrl Pts',(-11.4598615582757,-94.5117511126202,
2.02950100528141E-11));
#32359=CARTESIAN_POINT('Ctrl Pts',(-8.59489616869816,-94.3367511126202,
4.9622656166746));
#32360=CARTESIAN_POINT('Ctrl Pts',(-5.72993077912048,-94.1617511126202,
9.92453123332946));
#32361=CARTESIAN_POINT('Ctrl Pts',(1.75224980467247E-11,-93.9867511126202,
9.92453123331945));
#32362=CARTESIAN_POINT('Ctrl Pts',(5.72993077915496,-93.8117511126202,9.92453123330956));
#32363=CARTESIAN_POINT('Ctrl Pts',(8.5948961687154,-93.6367511126202,4.96226561664474));
#32364=CARTESIAN_POINT('Ctrl Pts',(11.4598615582757,-93.4617511126202,-2.01714658037908E-11));
#32365=CARTESIAN_POINT('Ctrl Pts',(8.59489616869793,-93.2867511126202,-4.962265616675));
#32366=CARTESIAN_POINT('Ctrl Pts',(5.72993077912059,-93.1117511126202,-9.9245312333294));
#32367=CARTESIAN_POINT('Ctrl Pts',(-1.74155055885791E-11,-92.9367511126202,
-9.92453123331945));
#32368=CARTESIAN_POINT('Ctrl Pts',(-5.72993077915542,-92.7617511126202,
-9.92453123330929));
#32369=CARTESIAN_POINT('Ctrl Pts',(-8.59489616871534,-92.5867511126202,
-4.96226561664484));
#32370=CARTESIAN_POINT('Ctrl Pts',(-11.4598615582757,-92.4117511126203,
2.00479215547674E-11));
#32371=CARTESIAN_POINT('Ctrl Pts',(-8.59489616869798,-92.2367511126202,
4.96226561667491));
#32372=CARTESIAN_POINT('Ctrl Pts',(-5.72993077912069,-92.0617511126202,
9.92453123332934));
#32373=CARTESIAN_POINT('Ctrl Pts',(1.73085131304334E-11,-91.8867511126202,
9.92453123331945));
#32374=CARTESIAN_POINT('Ctrl Pts',(5.72993077915531,-91.7117511126202,9.92453123330936));
#32375=CARTESIAN_POINT('Ctrl Pts',(8.59489616871557,-91.5367511126202,4.96226561664444));
#32376=CARTESIAN_POINT('Ctrl Pts',(11.4598615582757,-91.3617511126203,-1.99243773057441E-11));
#32377=CARTESIAN_POINT('Ctrl Pts',(8.59489616869803,-91.1867511126202,-4.96226561667481));
#32378=CARTESIAN_POINT('Ctrl Pts',(5.72993077912024,-91.0117511126202,-9.92453123332961));
#32379=CARTESIAN_POINT('Ctrl Pts',(-1.72015206722877E-11,-90.8367511126202,
-9.92453123331945));
#32380=CARTESIAN_POINT('Ctrl Pts',(-5.7299307791552,-90.6617511126203,-9.92453123330942));
#32381=CARTESIAN_POINT('Ctrl Pts',(-8.59489616871552,-90.4867511126203,
-4.96226561664453));
#32382=CARTESIAN_POINT('Ctrl Pts',(-11.4598615582757,-90.3117511126203,
1.98008330567208E-11));
#32383=CARTESIAN_POINT('Ctrl Pts',(-8.59489616869809,-90.1367511126202,
4.96226561667472));
#32384=CARTESIAN_POINT('Ctrl Pts',(-5.72993077912034,-89.9617511126202,
9.92453123332955));
#32385=CARTESIAN_POINT('Ctrl Pts',(1.7094528214142E-11,-89.7867511126202,
9.92453123331945));
#32386=CARTESIAN_POINT('Ctrl Pts',(5.7299307791551,-89.6117511126202,9.92453123330948));
#32387=CARTESIAN_POINT('Ctrl Pts',(8.59489616871547,-89.4367511126202,4.96226561664462));
#32388=CARTESIAN_POINT('Ctrl Pts',(11.4598615582757,-89.2617511126203,-2.03287065183413E-11));
#32389=CARTESIAN_POINT('Ctrl Pts',(8.59489616869814,-89.0867511126202,-4.96226561667463));
#32390=CARTESIAN_POINT('Ctrl Pts',(5.72993077912045,-88.9117511126202,-9.92453123332948));
#32391=CARTESIAN_POINT('Ctrl Pts',(-1.75516800418891E-11,-88.7367511126203,
-9.92453123331945));
#32392=CARTESIAN_POINT('Ctrl Pts',(-5.72993077915499,-88.5617511126202,
-9.92453123330954));
#32393=CARTESIAN_POINT('Ctrl Pts',(-8.59489616871541,-88.3867511126203,
-4.96226561664472));
#32394=CARTESIAN_POINT('Ctrl Pts',(-11.4598615582757,-88.2117511126202,
2.0205162269318E-11));
#32395=CARTESIAN_POINT('Ctrl Pts',(-8.5948961686982,-88.0367511126202,4.96226561667454));
#32396=CARTESIAN_POINT('Ctrl Pts',(-5.72993077912056,-87.8617511126203,
9.92453123332942));
#32397=CARTESIAN_POINT('Ctrl Pts',(1.74446875837434E-11,-87.6867511126203,
9.92453123331945));
#32398=CARTESIAN_POINT('Ctrl Pts',(5.72993077915545,-87.5117511126203,9.92453123330928));
#32399=CARTESIAN_POINT('Ctrl Pts',(8.59489616871536,-87.3367511126202,4.96226561664481));
#32400=CARTESIAN_POINT('Ctrl Pts',(11.4598615582757,-87.1617511126203,-2.00816180202947E-11));
#32401=CARTESIAN_POINT('Ctrl Pts',(8.59489616869797,-86.9867511126203,-4.96226561667493));
#32402=CARTESIAN_POINT('Ctrl Pts',(5.72993077912066,-86.8117511126202,-9.92453123332936));
#32403=CARTESIAN_POINT('Ctrl Pts',(-1.73376951255977E-11,-86.6367511126203,
-9.92453123331945));
#32404=CARTESIAN_POINT('Ctrl Pts',(-5.72993077915534,-86.4617511126202,
-9.92453123330934));
#32405=CARTESIAN_POINT('Ctrl Pts',(-8.59489616871531,-86.2867511126203,
-4.9622656166449));
#32406=CARTESIAN_POINT('Ctrl Pts',(-11.4598615582757,-86.1117511126203,
1.99580737712713E-11));
#32407=CARTESIAN_POINT('Ctrl Pts',(-8.59489616869802,-85.9367511126203,
4.96226561667484));
#32408=CARTESIAN_POINT('Ctrl Pts',(-5.72993077912021,-85.7617511126202,
9.92453123332962));
#32409=CARTESIAN_POINT('Ctrl Pts',(1.7230702667452E-11,-85.5867511126203,
9.92453123331945));
#32410=CARTESIAN_POINT('Ctrl Pts',(5.72993077915523,-85.4117511126203,9.9245312333094));
#32411=CARTESIAN_POINT('Ctrl Pts',(8.59489616871553,-85.2367511126202,4.96226561664451));
#32412=CARTESIAN_POINT('Ctrl Pts',(11.4598615582757,-85.0617511126203,-1.9834529522248E-11));
#32413=CARTESIAN_POINT('Ctrl Pts',(8.59489616869807,-84.8867511126203,-4.96226561667475));
#32414=CARTESIAN_POINT('Ctrl Pts',(5.72993077912031,-84.7117511126203,-9.92453123332956));
#32415=CARTESIAN_POINT('Ctrl Pts',(-1.71237102093063E-11,-84.5367511126202,
-9.92453123331945));
#32416=CARTESIAN_POINT('Ctrl Pts',(-5.72993077915512,-84.3617511126203,
-9.92453123330946));
#32417=CARTESIAN_POINT('Ctrl Pts',(-8.59489616871548,-84.1867511126203,
-4.9622656166446));
#32418=CARTESIAN_POINT('Ctrl Pts',(-11.4598615582757,-84.0117511126203,
1.97109852732247E-11));
#32419=CARTESIAN_POINT('Ctrl Pts',(-8.59489616869813,-83.8367511126203,
4.96226561667465));
#32420=CARTESIAN_POINT('Ctrl Pts',(-5.72993077912042,-83.6617511126203,
9.9245312333295));
#32421=CARTESIAN_POINT('Ctrl Pts',(1.75808620370534E-11,-83.4867511126202,
9.92453123331945));
#32422=CARTESIAN_POINT('Ctrl Pts',(5.72993077915502,-83.3117511126203,9.92453123330952));
#32423=CARTESIAN_POINT('Ctrl Pts',(8.59489616871543,-83.1367511126203,4.96226561664469));
#32424=CARTESIAN_POINT('Ctrl Pts',(11.4598615582757,-82.9617511126202,-2.02388587348453E-11));
#32425=CARTESIAN_POINT('Ctrl Pts',(8.59489616869818,-82.7867511126203,-4.96226561667456));
#32426=CARTESIAN_POINT('Ctrl Pts',(5.72993077912053,-82.6117511126203,-9.92453123332944));
#32427=CARTESIAN_POINT('Ctrl Pts',(-1.74738695789077E-11,-82.4367511126202,
-9.92453123331945));
#32428=CARTESIAN_POINT('Ctrl Pts',(-5.72993077915491,-82.2617511126203,
-9.92453123330959));
#32429=CARTESIAN_POINT('Ctrl Pts',(-8.59489616871537,-82.0867511126203,
-4.96226561664478));
#32430=CARTESIAN_POINT('Ctrl Pts',(-11.4598615582757,-81.9117511126203,
2.01153144858219E-11));
#32431=CARTESIAN_POINT('Ctrl Pts',(-8.59489616869795,-81.7367511126203,
4.96226561667496));
#32432=CARTESIAN_POINT('Ctrl Pts',(-5.72993077912063,-81.5617511126202,
9.92453123332938));
#32433=CARTESIAN_POINT('Ctrl Pts',(1.7366877120762E-11,-81.3867511126203,
9.92453123331945));
#32434=CARTESIAN_POINT('Ctrl Pts',(5.72993077915537,-81.2117511126203,9.92453123330932));
#32435=CARTESIAN_POINT('Ctrl Pts',(8.59489616871532,-81.0367511126203,4.96226561664488));
#32436=CARTESIAN_POINT('Ctrl Pts',(11.4598615582757,-80.8617511126203,-1.99917702367986E-11));
#32437=CARTESIAN_POINT('Ctrl Pts',(8.59489616869801,-80.6867511126203,-4.96226561667487));
#32438=CARTESIAN_POINT('Ctrl Pts',(5.72993077912074,-80.5117511126203,-9.92453123332931));
#32439=CARTESIAN_POINT('Ctrl Pts',(-1.72598846626164E-11,-80.3367511126203,
-9.92453123331945));
#32440=CARTESIAN_POINT('Ctrl Pts',(-5.72993077915526,-80.1617511126203,
-9.92453123330938));
#32441=CARTESIAN_POINT('Ctrl Pts',(-8.59489616871555,-79.9867511126203,
-4.96226561664448));
#32442=CARTESIAN_POINT('Ctrl Pts',(-11.4598615582757,-79.8117511126203,
1.98682259877752E-11));
#32443=CARTESIAN_POINT('Ctrl Pts',(-8.59489616869806,-79.6367511126202,
4.96226561667477));
#32444=CARTESIAN_POINT('Ctrl Pts',(-5.72993077912029,-79.4617511126203,
9.92453123332958));
#32445=CARTESIAN_POINT('Ctrl Pts',(1.71528922044707E-11,-79.2867511126203,
9.92453123331945));
#32446=CARTESIAN_POINT('Ctrl Pts',(5.72993077915515,-79.1117511126203,9.92453123330944));
#32447=CARTESIAN_POINT('Ctrl Pts',(8.59489616871549,-78.9367511126203,4.96226561664457));
#32448=CARTESIAN_POINT('Ctrl Pts',(11.4598615582757,-78.7617511126203,-1.97446817387519E-11));
#32449=CARTESIAN_POINT('Ctrl Pts',(8.59489616869811,-78.5867511126203,-4.96226561667468));
#32450=CARTESIAN_POINT('Ctrl Pts',(5.72993077912039,-78.4117511126203,-9.92453123332952));
#32451=CARTESIAN_POINT('Ctrl Pts',(-1.76100440322177E-11,-78.2367511126203,
-9.92453123331945));
#32452=CARTESIAN_POINT('Ctrl Pts',(-5.72993077915505,-78.0617511126203,
-9.92453123330951));
#32453=CARTESIAN_POINT('Ctrl Pts',(-8.59489616871544,-77.8867511126203,
-4.96226561664467));
#32454=CARTESIAN_POINT('Ctrl Pts',(-11.4598615582757,-77.7117511126203,
2.02725552003725E-11));
#32455=CARTESIAN_POINT('Ctrl Pts',(-8.59489616869817,-77.5367511126203,
4.96226561667459));
#32456=CARTESIAN_POINT('Ctrl Pts',(-5.7299307791205,-77.3617511126203,9.92453123332946));
#32457=CARTESIAN_POINT('Ctrl Pts',(1.75030515740721E-11,-77.1867511126203,
9.92453123331945));
#32458=CARTESIAN_POINT('Ctrl Pts',(5.72993077915494,-77.0117511126203,9.92453123330957));
#32459=CARTESIAN_POINT('Ctrl Pts',(8.59489616871539,-76.8367511126203,4.96226561664476));
#32460=CARTESIAN_POINT('Ctrl Pts',(11.4598615582757,-76.6617511126203,-2.01490109513492E-11));
#32461=CARTESIAN_POINT('Ctrl Pts',(8.59489616869822,-76.4867511126203,-4.96226561667449));
#32462=CARTESIAN_POINT('Ctrl Pts',(5.72993077912061,-76.3117511126203,-9.92453123332939));
#32463=CARTESIAN_POINT('Ctrl Pts',(-1.73960591159264E-11,-76.1367511126203,
-9.92453123331945));
#32464=CARTESIAN_POINT('Ctrl Pts',(-5.7299307791554,-75.9617511126203,-9.92453123330931));
#32465=CARTESIAN_POINT('Ctrl Pts',(-8.59489616871534,-75.7867511126203,
-4.96226561664485));
#32466=CARTESIAN_POINT('Ctrl Pts',(-11.4598615582757,-75.6117511126203,
2.00254667023258E-11));
#32467=CARTESIAN_POINT('Ctrl Pts',(-8.59489616869799,-75.4367511126203,
4.96226561667489));
#32468=CARTESIAN_POINT('Ctrl Pts',(-5.72993077912071,-75.2617511126203,
9.92453123332933));
#32469=CARTESIAN_POINT('Ctrl Pts',(1.72890666577807E-11,-75.0867511126203,
9.92453123331945));
#32470=CARTESIAN_POINT('Ctrl Pts',(5.72993077915529,-74.9117511126203,9.92453123330937));
#32471=CARTESIAN_POINT('Ctrl Pts',(8.59489616871528,-74.7367511126203,4.96226561664494));
#32472=CARTESIAN_POINT('Ctrl Pts',(11.4598615582757,-74.5617511126203,-1.99019224533025E-11));
#32473=CARTESIAN_POINT('Ctrl Pts',(8.59489616869805,-74.3867511126203,-4.9622656166748));
#32474=CARTESIAN_POINT('Ctrl Pts',(5.72993077912025,-74.2117511126203,-9.9245312333296));
#32475=CARTESIAN_POINT('Ctrl Pts',(-1.7182074199635E-11,-74.0367511126203,
-9.92453123331945));
#32476=CARTESIAN_POINT('Ctrl Pts',(-5.72993077915518,-73.8617511126203,
-9.92453123330943));
#32477=CARTESIAN_POINT('Ctrl Pts',(-8.59489616871551,-73.6867511126203,
-4.96226561664455));
#32478=CARTESIAN_POINT('Ctrl Pts',(-11.4598615582757,-73.5117511126203,
1.97783782042791E-11));
#32479=CARTESIAN_POINT('Ctrl Pts',(-8.5948961686981,-73.3367511126203,4.9622656166747));
#32480=CARTESIAN_POINT('Ctrl Pts',(-5.72993077912036,-73.1617511126203,
9.92453123332954));
#32481=CARTESIAN_POINT('Ctrl Pts',(1.70750817414893E-11,-72.9867511126203,
9.92453123331945));
#32482=CARTESIAN_POINT('Ctrl Pts',(5.72993077915508,-72.8117511126203,9.92453123330949));
#32483=CARTESIAN_POINT('Ctrl Pts',(8.59489616871546,-72.6367511126203,4.96226561664464));
#32484=CARTESIAN_POINT('Ctrl Pts',(11.4598615582757,-72.4617511126203,-2.03062516658997E-11));
#32485=CARTESIAN_POINT('Ctrl Pts',(8.59489616869815,-72.2867511126203,-4.96226561667461));
#32486=CARTESIAN_POINT('Ctrl Pts',(5.72993077912047,-72.1117511126203,-9.92453123332947));
#32487=CARTESIAN_POINT('Ctrl Pts',(-1.75322335692364E-11,-71.9367511126203,
-9.92453123331945));
#32488=CARTESIAN_POINT('Ctrl Pts',(-5.72993077915497,-71.7617511126203,
-9.92453123330955));
#32489=CARTESIAN_POINT('Ctrl Pts',(-8.5948961687154,-71.5867511126203,-4.96226561664473));
#32490=CARTESIAN_POINT('Ctrl Pts',(-11.4598615582757,-71.4117511126203,
2.01827074168764E-11));
#32491=CARTESIAN_POINT('Ctrl Pts',(-8.59489616869821,-71.2367511126203,
4.96226561667452));
#32492=CARTESIAN_POINT('Ctrl Pts',(-5.72993077912058,-71.0617511126203,
9.92453123332941));
#32493=CARTESIAN_POINT('Ctrl Pts',(1.74252411110907E-11,-70.8867511126203,
9.92453123331945));
#32494=CARTESIAN_POINT('Ctrl Pts',(5.72993077915486,-70.7117511126203,9.92453123330961));
#32495=CARTESIAN_POINT('Ctrl Pts',(8.59489616871535,-70.5367511126203,4.96226561664483));
#32496=CARTESIAN_POINT('Ctrl Pts',(11.4598615582757,-70.3617511126203,-2.0059163167853E-11));
#32497=CARTESIAN_POINT('Ctrl Pts',(8.59489616869798,-70.1867511126203,-4.96226561667492));
#32498=CARTESIAN_POINT('Ctrl Pts',(5.72993077912068,-70.0117511126203,-9.92453123332935));
#32499=CARTESIAN_POINT('Ctrl Pts',(-1.7318248652945E-11,-69.8367511126203,
-9.92453123331945));
#32500=CARTESIAN_POINT('Ctrl Pts',(-5.72993077915532,-69.6617511126203,
-9.92453123330935));
#32501=CARTESIAN_POINT('Ctrl Pts',(-8.59489616871529,-69.4867511126203,
-4.96226561664492));
#32502=CARTESIAN_POINT('Ctrl Pts',(-11.4598615582757,-69.3117511126203,
1.99356189188297E-11));
#32503=CARTESIAN_POINT('Ctrl Pts',(-8.59489616869803,-69.1367511126203,
4.96226561667482));
#32504=CARTESIAN_POINT('Ctrl Pts',(-5.72993077912079,-68.9617511126203,
9.92453123332929));
#32505=CARTESIAN_POINT('Ctrl Pts',(1.72112561947994E-11,-68.7867511126203,
9.92453123331945));
#32506=CARTESIAN_POINT('Ctrl Pts',(5.72993077915521,-68.6117511126203,9.92453123330941));
#32507=CARTESIAN_POINT('Ctrl Pts',(8.59489616871553,-68.4367511126203,4.96226561664452));
#32508=CARTESIAN_POINT('Ctrl Pts',(11.4598615582757,-68.2617511126203,-1.98120746698064E-11));
#32509=CARTESIAN_POINT('Ctrl Pts',(8.59489616869808,-68.0867511126203,-4.96226561667473));
#32510=CARTESIAN_POINT('Ctrl Pts',(5.72993077912033,-67.9117511126203,-9.92453123332955));
#32511=CARTESIAN_POINT('Ctrl Pts',(-1.71042637366537E-11,-67.7367511126203,
-9.92453123331945));
#32512=CARTESIAN_POINT('Ctrl Pts',(-5.72993077915511,-67.5617511126203,
-9.92453123330947));
#32513=CARTESIAN_POINT('Ctrl Pts',(-8.59489616871547,-67.3867511126203,
-4.96226561664462));
#32514=CARTESIAN_POINT('Ctrl Pts',(-11.4598615582757,-67.2117511126203,
1.9688530420783E-11));
#32515=CARTESIAN_POINT('Ctrl Pts',(-8.59489616869814,-67.0367511126203,
4.96226561667464));
#32516=CARTESIAN_POINT('Ctrl Pts',(-5.72993077912044,-66.8617511126203,
9.92453123332949));
#32517=CARTESIAN_POINT('Ctrl Pts',(1.75614155644007E-11,-66.6867511126203,
9.92453123331945));
#32518=CARTESIAN_POINT('Ctrl Pts',(5.729930779155,-66.5117511126203,9.92453123330953));
#32519=CARTESIAN_POINT('Ctrl Pts',(8.59489616871542,-66.3367511126203,4.96226561664471));
#32520=CARTESIAN_POINT('Ctrl Pts',(11.4598615582757,-66.1617511126203,-2.02164038824036E-11));
#32521=CARTESIAN_POINT('Ctrl Pts',(8.59489616869819,-65.9867511126203,-4.96226561667455));
#32522=CARTESIAN_POINT('Ctrl Pts',(5.72993077912055,-65.8117511126203,-9.92453123332943));
#32523=CARTESIAN_POINT('Ctrl Pts',(-1.74544231062551E-11,-65.6367511126203,
-9.92453123331945));
#32524=CARTESIAN_POINT('Ctrl Pts',(-5.72993077915489,-65.4617511126203,
-9.9245312333096));
#32525=CARTESIAN_POINT('Ctrl Pts',(-8.59489616871537,-65.2867511126203,
-4.9622656166448));
#32526=CARTESIAN_POINT('Ctrl Pts',(-11.4598615582757,-65.1117511126203,
2.00928596333803E-11));
#32527=CARTESIAN_POINT('Ctrl Pts',(-8.59489616869824,-64.9367511126203,
4.96226561667445));
#32528=CARTESIAN_POINT('Ctrl Pts',(-5.72993077912065,-64.7617511126203,
9.92453123332936));
#32529=CARTESIAN_POINT('Ctrl Pts',(1.73474306481094E-11,-64.5867511126203,
9.92453123331945));
#32530=CARTESIAN_POINT('Ctrl Pts',(5.72993077915535,-64.4117511126203,9.92453123330933));
#32531=CARTESIAN_POINT('Ctrl Pts',(8.59489616871531,-64.2367511126203,4.96226561664489));
#32532=CARTESIAN_POINT('Ctrl Pts',(11.4598615582757,-64.0617511126203,-1.9969315384357E-11));
#32533=CARTESIAN_POINT('Ctrl Pts',(8.59489616869802,-63.8867511126203,-4.96226561667485));
#32534=CARTESIAN_POINT('Ctrl Pts',(5.72993077912076,-63.7117511126203,-9.9245312333293));
#32535=CARTESIAN_POINT('Ctrl Pts',(-1.72404381899637E-11,-63.5367511126203,
-9.92453123331945));
#32536=CARTESIAN_POINT('Ctrl Pts',(-5.72993077915524,-63.3617511126203,
-9.92453123330939));
#32537=CARTESIAN_POINT('Ctrl Pts',(-8.59489616871526,-63.1867511126203,
-4.96226561664499));
#32538=CARTESIAN_POINT('Ctrl Pts',(-11.4598615582757,-63.0117511126203,
1.98457711353336E-11));
#32539=CARTESIAN_POINT('Ctrl Pts',(-8.59489616869807,-62.8367511126203,
4.96226561667476));
#32540=CARTESIAN_POINT('Ctrl Pts',(-5.7299307791203,-62.6617511126203,9.92453123332957));
#32541=CARTESIAN_POINT('Ctrl Pts',(1.7133445731818E-11,-62.4867511126203,
9.92453123331945));
#32542=CARTESIAN_POINT('Ctrl Pts',(5.72993077915513,-62.3117511126203,9.92453123330946));
#32543=CARTESIAN_POINT('Ctrl Pts',(8.59489616871549,-62.1367511126203,4.96226561664459));
#32544=CARTESIAN_POINT('Ctrl Pts',(11.4598615582757,-61.9617511126203,-1.97222268863103E-11));
#32545=CARTESIAN_POINT('Ctrl Pts',(8.59489616869812,-61.7867511126203,-4.96226561667466));
#32546=CARTESIAN_POINT('Ctrl Pts',(5.72993077912041,-61.6117511126203,-9.92453123332951));
#32547=CARTESIAN_POINT('Ctrl Pts',(-1.70264532736723E-11,-61.4367511126203,
-9.92453123331945));
#32548=CARTESIAN_POINT('Ctrl Pts',(-5.72993077915503,-61.2617511126203,
-9.92453123330952));
#32549=CARTESIAN_POINT('Ctrl Pts',(-8.59489616871543,-61.0867511126203,
-4.96226561664468));
#32550=CARTESIAN_POINT('Ctrl Pts',(-11.4598615582757,-60.9117511126203,
2.02501003479309E-11));
#32551=CARTESIAN_POINT('Ctrl Pts',(-8.59489616869817,-60.7367511126203,
4.96226561667457));
#32552=CARTESIAN_POINT('Ctrl Pts',(-5.72993077912052,-60.5617511126203,
9.92453123332944));
#32553=CARTESIAN_POINT('Ctrl Pts',(1.74836051014194E-11,-60.3867511126203,
9.92453123331945));
#32554=CARTESIAN_POINT('Ctrl Pts',(5.72993077915492,-60.2117511126203,9.92453123330958));
#32555=CARTESIAN_POINT('Ctrl Pts',(8.59489616871538,-60.0367511126203,4.96226561664478));
#32556=CARTESIAN_POINT('Ctrl Pts',(11.4598615582757,-59.8617511126203,-2.01265560989075E-11));
#32557=CARTESIAN_POINT('Ctrl Pts',(8.59489616869823,-59.6867511126203,-4.96226561667448));
#32558=CARTESIAN_POINT('Ctrl Pts',(5.72993077912063,-59.5117511126203,-9.92453123332938));
#32559=CARTESIAN_POINT('Ctrl Pts',(-1.73766126432737E-11,-59.3367511126203,
-9.92453123331945));
#32560=CARTESIAN_POINT('Ctrl Pts',(-5.72993077915538,-59.1617511126203,
-9.92453123330931));
#32561=CARTESIAN_POINT('Ctrl Pts',(-8.59489616871532,-58.9867511126203,
-4.96226561664487));
#32562=CARTESIAN_POINT('Ctrl Pts',(-11.4598615582757,-58.8117511126203,
2.00030118498842E-11));
#32563=CARTESIAN_POINT('Ctrl Pts',(-8.594896168698,-58.6367511126203,4.96226561667487));
#32564=CARTESIAN_POINT('Ctrl Pts',(-5.72993077912073,-58.4617511126203,
9.92453123332932));
#32565=CARTESIAN_POINT('Ctrl Pts',(1.7269620185128E-11,-58.2867511126203,
9.92453123331945));
#32566=CARTESIAN_POINT('Ctrl Pts',(5.72993077915527,-58.1117511126203,9.92453123330938));
#32567=CARTESIAN_POINT('Ctrl Pts',(8.59489616871527,-57.9367511126203,4.96226561664496));
#32568=CARTESIAN_POINT('Ctrl Pts',(11.4598615582757,-57.7617511126203,-1.98794676008609E-11));
#32569=CARTESIAN_POINT('Ctrl Pts',(8.59489616869805,-57.5867511126203,-4.96226561667478));
#32570=CARTESIAN_POINT('Ctrl Pts',(5.72993077912084,-57.4117511126203,-9.92453123332926));
#32571=CARTESIAN_POINT('Ctrl Pts',(-1.71626277269823E-11,-57.2367511126203,
-9.92453123331945));
#32572=CARTESIAN_POINT('Ctrl Pts',(-5.72993077915516,-57.0617511126203,
-9.92453123330944));
#32573=CARTESIAN_POINT('Ctrl Pts',(-8.5948961687155,-56.8867511126203,-4.96226561664457));
#32574=CARTESIAN_POINT('Ctrl Pts',(-11.4598615582757,-56.7117511126203,
1.97559233518375E-11));
#32575=CARTESIAN_POINT('Ctrl Pts',(-8.59489616869811,-56.5367511126203,
4.96226561667469));
#32576=CARTESIAN_POINT('Ctrl Pts',(-5.72993077912038,-56.3617511126203,
9.92453123332952));
#32577=CARTESIAN_POINT('Ctrl Pts',(1.70556352688367E-11,-56.1867511126203,
9.92453123331945));
#32578=CARTESIAN_POINT('Ctrl Pts',(5.72993077915506,-56.0117511126203,9.9245312333095));
#32579=CARTESIAN_POINT('Ctrl Pts',(8.59489616871545,-55.8367511126203,4.96226561664466));
#32580=CARTESIAN_POINT('Ctrl Pts',(11.4598615582757,-55.6617511126203,-1.96323791028142E-11));
#32581=CARTESIAN_POINT('Ctrl Pts',(8.59489616869816,-55.4867511126203,-4.96226561667459));
#32582=CARTESIAN_POINT('Ctrl Pts',(5.72993077912049,-55.3117511126203,-9.92453123332946));
#32583=CARTESIAN_POINT('Ctrl Pts',(-1.75127870965837E-11,-55.1367511126203,
-9.92453123331945));
#32584=CARTESIAN_POINT('Ctrl Pts',(-5.72993077915495,-54.9617511126203,
-9.92453123330957));
#32585=CARTESIAN_POINT('Ctrl Pts',(-8.59489616871539,-54.7867511126203,
-4.96226561664475));
#32586=CARTESIAN_POINT('Ctrl Pts',(-11.4598615582757,-54.6117511126203,
2.01602525644348E-11));
#32587=CARTESIAN_POINT('Ctrl Pts',(-8.59489616869821,-54.4367511126203,
4.9622656166745));
#32588=CARTESIAN_POINT('Ctrl Pts',(-5.7299307791206,-54.2617511126203,9.9245312333294));
#32589=CARTESIAN_POINT('Ctrl Pts',(1.7405794638438E-11,-54.0867511126203,
9.92453123331945));
#32590=CARTESIAN_POINT('Ctrl Pts',(5.72993077915484,-53.9117511126203,9.92453123330963));
#32591=CARTESIAN_POINT('Ctrl Pts',(8.59489616871534,-53.7367511126203,4.96226561664484));
#32592=CARTESIAN_POINT('Ctrl Pts',(11.4598615582757,-53.5617511126203,-2.00367083154114E-11));
#32593=CARTESIAN_POINT('Ctrl Pts',(8.59489616869799,-53.3867511126203,-4.9622656166749));
#32594=CARTESIAN_POINT('Ctrl Pts',(5.7299307791207,-53.2117511126203,-9.92453123332934));
#32595=CARTESIAN_POINT('Ctrl Pts',(-1.72988021802924E-11,-53.0367511126203,
-9.92453123331945));
#32596=CARTESIAN_POINT('Ctrl Pts',(-5.7299307791553,-52.8617511126203,-9.92453123330936));
#32597=CARTESIAN_POINT('Ctrl Pts',(-8.59489616871529,-52.6867511126203,
-4.96226561664494));
#32598=CARTESIAN_POINT('Ctrl Pts',(-11.4598615582757,-52.5117511126203,
1.99131640663881E-11));
#32599=CARTESIAN_POINT('Ctrl Pts',(-8.59489616869804,-52.3367511126203,
4.96226561667481));
#32600=CARTESIAN_POINT('Ctrl Pts',(-5.72993077912081,-52.1617511126203,
9.92453123332928));
#32601=CARTESIAN_POINT('Ctrl Pts',(1.71918097221467E-11,-51.9867511126203,
9.92453123331945));
#32602=CARTESIAN_POINT('Ctrl Pts',(5.72993077915519,-51.8117511126203,9.92453123330942));
#32603=CARTESIAN_POINT('Ctrl Pts',(8.59489616871523,-51.6367511126203,4.96226561664503));
#32604=CARTESIAN_POINT('Ctrl Pts',(11.4598615582757,-51.4617511126203,-1.97896198173647E-11));
#32605=CARTESIAN_POINT('Ctrl Pts',(8.59489616869809,-51.2867511126203,-4.96226561667471));
#32606=CARTESIAN_POINT('Ctrl Pts',(5.72993077912035,-51.1117511126203,-9.92453123332954));
#32607=CARTESIAN_POINT('Ctrl Pts',(-1.7084817264001E-11,-50.9367511126203,
-9.92453123331945));
#32608=CARTESIAN_POINT('Ctrl Pts',(-5.72993077915509,-50.7617511126203,
-9.92453123330948));
#32609=CARTESIAN_POINT('Ctrl Pts',(-8.59489616871546,-50.5867511126203,
-4.96226561664463));
#32610=CARTESIAN_POINT('Ctrl Pts',(-11.4598615582757,-50.4117511126204,
1.96660755683414E-11));
#32611=CARTESIAN_POINT('Ctrl Pts',(-8.59489616869815,-50.2367511126203,
4.96226561667462));
#32612=CARTESIAN_POINT('Ctrl Pts',(-5.72993077912046,-50.0617511126203,
9.92453123332948));
#32613=CARTESIAN_POINT('Ctrl Pts',(1.69778248058553E-11,-49.8867511126203,
9.92453123331945));
#32614=CARTESIAN_POINT('Ctrl Pts',(5.72993077915498,-49.7117511126203,9.92453123330955));
#32615=CARTESIAN_POINT('Ctrl Pts',(8.59489616871541,-49.5367511126204,4.96226561664473));
#32616=CARTESIAN_POINT('Ctrl Pts',(11.4598615582757,-49.3617511126203,-2.0193949029962E-11));
#32617=CARTESIAN_POINT('Ctrl Pts',(8.5948961686982,-49.1867511126203,-4.96226561667453));
#32618=CARTESIAN_POINT('Ctrl Pts',(5.72993077912057,-49.0117511126203,-9.92453123332941));
#32619=CARTESIAN_POINT('Ctrl Pts',(-1.74349766336024E-11,-48.8367511126203,
-9.92453123331945));
#32620=CARTESIAN_POINT('Ctrl Pts',(-5.72993077915487,-48.6617511126203,
-9.92453123330961));
#32621=CARTESIAN_POINT('Ctrl Pts',(-8.59489616871535,-48.4867511126203,
-4.96226561664482));
#32622=CARTESIAN_POINT('Ctrl Pts',(-11.4598615582757,-48.3117511126203,
2.00704047809387E-11));
#32623=CARTESIAN_POINT('Ctrl Pts',(-8.59489616869825,-48.1367511126203,
4.96226561667444));
#32624=CARTESIAN_POINT('Ctrl Pts',(-5.72993077912067,-47.9617511126203,
9.92453123332935));
#32625=CARTESIAN_POINT('Ctrl Pts',(1.73279841754567E-11,-47.7867511126204,
9.92453123331945));
#32626=CARTESIAN_POINT('Ctrl Pts',(2.38370069761474,-47.7139496010212,9.92453123331524));
#32627=CARTESIAN_POINT('Ctrl Pts',(4.50738083181344,-47.63,8.84193633985987));
#32628=CARTESIAN_POINT('Ctrl Pts',(-1.51301075899711E-11,-213.943984254242,
-8.40164026751963));
#32629=CARTESIAN_POINT('Ctrl Pts',(-4.85068927010199,-213.768984254242,
-8.4016402675109));
#32630=CARTESIAN_POINT('Ctrl Pts',(-7.27603390513785,-213.593984254242,
-4.20082013374671));
#32631=CARTESIAN_POINT('Ctrl Pts',(-9.70137854017372,-213.418984254242,
1.74701493417668E-11));
#32632=CARTESIAN_POINT('Ctrl Pts',(-7.27603390512272,-213.243984254242,
4.20082013377292));
#32633=CARTESIAN_POINT('Ctrl Pts',(-4.85068927007173,-213.068984254242,
8.40164026752836));
#32634=CARTESIAN_POINT('Ctrl Pts',(1.5129078685785E-11,-212.893984254242,
8.40164026751963));
#32635=CARTESIAN_POINT('Ctrl Pts',(4.85068927010198,-212.718984254242,8.4016402675109));
#32636=CARTESIAN_POINT('Ctrl Pts',(7.27603390513785,-212.543984254242,4.20082013374672));
#32637=CARTESIAN_POINT('Ctrl Pts',(9.70137854017372,-212.368984254242,-1.74689612655491E-11));
#32638=CARTESIAN_POINT('Ctrl Pts',(7.27603390512273,-212.193984254242,-4.20082013377291));
#32639=CARTESIAN_POINT('Ctrl Pts',(4.85068927007173,-212.018984254242,-8.40164026752836));
#32640=CARTESIAN_POINT('Ctrl Pts',(-1.51301075899711E-11,-211.843984254242,
-8.40164026751963));
#32641=CARTESIAN_POINT('Ctrl Pts',(-4.85068927010199,-211.668984254242,
-8.4016402675109));
#32642=CARTESIAN_POINT('Ctrl Pts',(-7.27603390513785,-211.493984254242,
-4.20082013374671));
#32643=CARTESIAN_POINT('Ctrl Pts',(-9.70137854017372,-211.318984254242,
1.74701493417668E-11));
#32644=CARTESIAN_POINT('Ctrl Pts',(-7.27603390512272,-211.143984254242,
4.20082013377292));
#32645=CARTESIAN_POINT('Ctrl Pts',(-4.85068927007173,-210.968984254242,
8.40164026752836));
#32646=CARTESIAN_POINT('Ctrl Pts',(1.5129078685785E-11,-210.793984254242,
8.40164026751963));
#32647=CARTESIAN_POINT('Ctrl Pts',(4.85068927010198,-210.618984254242,8.4016402675109));
#32648=CARTESIAN_POINT('Ctrl Pts',(7.27603390513785,-210.443984254242,4.20082013374672));
#32649=CARTESIAN_POINT('Ctrl Pts',(9.70137854017372,-210.268984254242,-1.74689612655491E-11));
#32650=CARTESIAN_POINT('Ctrl Pts',(7.27603390512273,-210.093984254242,-4.20082013377291));
#32651=CARTESIAN_POINT('Ctrl Pts',(4.85068927007173,-209.918984254242,-8.40164026752836));
#32652=CARTESIAN_POINT('Ctrl Pts',(-1.51301075899711E-11,-209.743984254242,
-8.40164026751963));
#32653=CARTESIAN_POINT('Ctrl Pts',(-4.85068927010199,-209.568984254242,
-8.4016402675109));
#32654=CARTESIAN_POINT('Ctrl Pts',(-7.27603390513785,-209.393984254242,
-4.20082013374671));
#32655=CARTESIAN_POINT('Ctrl Pts',(-9.70137854017372,-209.218984254242,
1.74701493417668E-11));
#32656=CARTESIAN_POINT('Ctrl Pts',(-7.27603390512272,-209.043984254242,
4.20082013377292));
#32657=CARTESIAN_POINT('Ctrl Pts',(-4.85068927007173,-208.868984254242,
8.40164026752836));
#32658=CARTESIAN_POINT('Ctrl Pts',(1.5129078685785E-11,-208.693984254242,
8.40164026751963));
#32659=CARTESIAN_POINT('Ctrl Pts',(4.85068927010198,-208.518984254242,8.4016402675109));
#32660=CARTESIAN_POINT('Ctrl Pts',(7.27603390513785,-208.343984254242,4.20082013374672));
#32661=CARTESIAN_POINT('Ctrl Pts',(9.70137854017372,-208.168984254242,-1.74689612655491E-11));
#32662=CARTESIAN_POINT('Ctrl Pts',(7.27603390512273,-207.993984254242,-4.20082013377291));
#32663=CARTESIAN_POINT('Ctrl Pts',(4.85068927007173,-207.818984254242,-8.40164026752836));
#32664=CARTESIAN_POINT('Ctrl Pts',(-1.51301075899711E-11,-207.643984254242,
-8.40164026751963));
#32665=CARTESIAN_POINT('Ctrl Pts',(-4.85068927010199,-207.468984254242,
-8.4016402675109));
#32666=CARTESIAN_POINT('Ctrl Pts',(-7.27603390513785,-207.293984254242,
-4.20082013374671));
#32667=CARTESIAN_POINT('Ctrl Pts',(-9.70137854017372,-207.118984254242,
1.74701493417668E-11));
#32668=CARTESIAN_POINT('Ctrl Pts',(-7.27603390512272,-206.943984254242,
4.20082013377292));
#32669=CARTESIAN_POINT('Ctrl Pts',(-4.85068927007173,-206.768984254242,
8.40164026752836));
#32670=CARTESIAN_POINT('Ctrl Pts',(1.5129078685785E-11,-206.593984254242,
8.40164026751963));
#32671=CARTESIAN_POINT('Ctrl Pts',(4.85068927010198,-206.418984254242,8.4016402675109));
#32672=CARTESIAN_POINT('Ctrl Pts',(7.27603390513785,-206.243984254242,4.20082013374672));
#32673=CARTESIAN_POINT('Ctrl Pts',(9.70137854017372,-206.068984254242,-1.74689612655491E-11));
#32674=CARTESIAN_POINT('Ctrl Pts',(7.27603390512273,-205.893984254242,-4.20082013377291));
#32675=CARTESIAN_POINT('Ctrl Pts',(4.85068927007173,-205.718984254242,-8.40164026752836));
#32676=CARTESIAN_POINT('Ctrl Pts',(-1.51301075899711E-11,-205.543984254242,
-8.40164026751963));
#32677=CARTESIAN_POINT('Ctrl Pts',(-4.85068927010199,-205.368984254242,
-8.4016402675109));
#32678=CARTESIAN_POINT('Ctrl Pts',(-7.27603390513785,-205.193984254242,
-4.20082013374671));
#32679=CARTESIAN_POINT('Ctrl Pts',(-9.70137854017372,-205.018984254242,
1.74701493417668E-11));
#32680=CARTESIAN_POINT('Ctrl Pts',(-7.27603390512272,-204.843984254242,
4.20082013377292));
#32681=CARTESIAN_POINT('Ctrl Pts',(-4.85068927007173,-204.668984254242,
8.40164026752836));
#32682=CARTESIAN_POINT('Ctrl Pts',(1.5129078685785E-11,-204.493984254242,
8.40164026751963));
#32683=CARTESIAN_POINT('Ctrl Pts',(4.85068927010198,-204.318984254242,8.4016402675109));
#32684=CARTESIAN_POINT('Ctrl Pts',(7.27603390513785,-204.143984254242,4.20082013374672));
#32685=CARTESIAN_POINT('Ctrl Pts',(9.70137854017372,-203.968984254242,-1.74689612655491E-11));
#32686=CARTESIAN_POINT('Ctrl Pts',(7.27603390512273,-203.793984254242,-4.20082013377291));
#32687=CARTESIAN_POINT('Ctrl Pts',(4.85068927007173,-203.618984254242,-8.40164026752836));
#32688=CARTESIAN_POINT('Ctrl Pts',(-1.51301075899711E-11,-203.443984254242,
-8.40164026751963));
#32689=CARTESIAN_POINT('Ctrl Pts',(-4.85068927010199,-203.268984254242,
-8.4016402675109));
#32690=CARTESIAN_POINT('Ctrl Pts',(-7.27603390513785,-203.093984254242,
-4.20082013374671));
#32691=CARTESIAN_POINT('Ctrl Pts',(-9.70137854017372,-202.918984254242,
1.74701493417668E-11));
#32692=CARTESIAN_POINT('Ctrl Pts',(-7.27603390512272,-202.743984254242,
4.20082013377292));
#32693=CARTESIAN_POINT('Ctrl Pts',(-4.85068927007173,-202.568984254242,
8.40164026752836));
#32694=CARTESIAN_POINT('Ctrl Pts',(1.5129078685785E-11,-202.393984254242,
8.40164026751963));
#32695=CARTESIAN_POINT('Ctrl Pts',(4.85068927010198,-202.218984254242,8.4016402675109));
#32696=CARTESIAN_POINT('Ctrl Pts',(7.27603390513785,-202.043984254242,4.20082013374672));
#32697=CARTESIAN_POINT('Ctrl Pts',(9.70137854017372,-201.868984254242,-1.74689612655491E-11));
#32698=CARTESIAN_POINT('Ctrl Pts',(7.27603390512273,-201.693984254242,-4.20082013377291));
#32699=CARTESIAN_POINT('Ctrl Pts',(4.85068927007173,-201.518984254242,-8.40164026752836));
#32700=CARTESIAN_POINT('Ctrl Pts',(-1.51301075899711E-11,-201.343984254242,
-8.40164026751963));
#32701=CARTESIAN_POINT('Ctrl Pts',(-4.85068927010199,-201.168984254242,
-8.4016402675109));
#32702=CARTESIAN_POINT('Ctrl Pts',(-7.27603390513785,-200.993984254242,
-4.20082013374671));
#32703=CARTESIAN_POINT('Ctrl Pts',(-9.70137854017372,-200.818984254242,
1.74701493417668E-11));
#32704=CARTESIAN_POINT('Ctrl Pts',(-7.27603390512272,-200.643984254242,
4.20082013377292));
#32705=CARTESIAN_POINT('Ctrl Pts',(-4.85068927007173,-200.468984254242,
8.40164026752836));
#32706=CARTESIAN_POINT('Ctrl Pts',(1.5129078685785E-11,-200.293984254242,
8.40164026751963));
#32707=CARTESIAN_POINT('Ctrl Pts',(4.85068927010198,-200.118984254242,8.4016402675109));
#32708=CARTESIAN_POINT('Ctrl Pts',(7.27603390513785,-199.943984254242,4.20082013374672));
#32709=CARTESIAN_POINT('Ctrl Pts',(9.70137854017372,-199.768984254242,-1.74689612655491E-11));
#32710=CARTESIAN_POINT('Ctrl Pts',(7.27603390512273,-199.593984254242,-4.20082013377291));
#32711=CARTESIAN_POINT('Ctrl Pts',(4.85068927007173,-199.418984254242,-8.40164026752836));
#32712=CARTESIAN_POINT('Ctrl Pts',(-1.51301075899711E-11,-199.243984254242,
-8.40164026751963));
#32713=CARTESIAN_POINT('Ctrl Pts',(-4.85068927010199,-199.068984254242,
-8.4016402675109));
#32714=CARTESIAN_POINT('Ctrl Pts',(-7.27603390513785,-198.893984254242,
-4.20082013374671));
#32715=CARTESIAN_POINT('Ctrl Pts',(-9.70137854017372,-198.718984254242,
1.74701493417668E-11));
#32716=CARTESIAN_POINT('Ctrl Pts',(-7.27603390512272,-198.543984254242,
4.20082013377292));
#32717=CARTESIAN_POINT('Ctrl Pts',(-4.85068927007173,-198.368984254242,
8.40164026752836));
#32718=CARTESIAN_POINT('Ctrl Pts',(1.5129078685785E-11,-198.193984254242,
8.40164026751963));
#32719=CARTESIAN_POINT('Ctrl Pts',(4.85068927010198,-198.018984254242,8.4016402675109));
#32720=CARTESIAN_POINT('Ctrl Pts',(7.27603390513785,-197.843984254242,4.20082013374672));
#32721=CARTESIAN_POINT('Ctrl Pts',(9.70137854017372,-197.668984254242,-1.74689612655491E-11));
#32722=CARTESIAN_POINT('Ctrl Pts',(7.27603390512273,-197.493984254242,-4.20082013377291));
#32723=CARTESIAN_POINT('Ctrl Pts',(4.85068927007173,-197.318984254242,-8.40164026752836));
#32724=CARTESIAN_POINT('Ctrl Pts',(-1.51301075899711E-11,-197.143984254242,
-8.40164026751963));
#32725=CARTESIAN_POINT('Ctrl Pts',(-4.85068927010199,-196.968984254242,
-8.4016402675109));
#32726=CARTESIAN_POINT('Ctrl Pts',(-7.27603390513785,-196.793984254242,
-4.20082013374671));
#32727=CARTESIAN_POINT('Ctrl Pts',(-9.70137854017372,-196.618984254242,
1.74701493417668E-11));
#32728=CARTESIAN_POINT('Ctrl Pts',(-7.27603390512272,-196.443984254242,
4.20082013377292));
#32729=CARTESIAN_POINT('Ctrl Pts',(-4.85068927007173,-196.268984254242,
8.40164026752836));
#32730=CARTESIAN_POINT('Ctrl Pts',(1.5129078685785E-11,-196.093984254242,
8.40164026751963));
#32731=CARTESIAN_POINT('Ctrl Pts',(4.85068927010198,-195.918984254242,8.4016402675109));
#32732=CARTESIAN_POINT('Ctrl Pts',(7.27603390513785,-195.743984254242,4.20082013374672));
#32733=CARTESIAN_POINT('Ctrl Pts',(9.70137854017372,-195.568984254242,-1.74689612655491E-11));
#32734=CARTESIAN_POINT('Ctrl Pts',(7.27603390512273,-195.393984254242,-4.20082013377291));
#32735=CARTESIAN_POINT('Ctrl Pts',(4.85068927007173,-195.218984254242,-8.40164026752836));
#32736=CARTESIAN_POINT('Ctrl Pts',(-1.51301075899711E-11,-195.043984254242,
-8.40164026751963));
#32737=CARTESIAN_POINT('Ctrl Pts',(-4.85068927010199,-194.868984254242,
-8.4016402675109));
#32738=CARTESIAN_POINT('Ctrl Pts',(-7.27603390513785,-194.693984254242,
-4.20082013374671));
#32739=CARTESIAN_POINT('Ctrl Pts',(-9.70137854017372,-194.518984254242,
1.74701493417668E-11));
#32740=CARTESIAN_POINT('Ctrl Pts',(-7.27603390512272,-194.343984254242,
4.20082013377292));
#32741=CARTESIAN_POINT('Ctrl Pts',(-4.85068927007173,-194.168984254242,
8.40164026752836));
#32742=CARTESIAN_POINT('Ctrl Pts',(1.5129078685785E-11,-193.993984254242,
8.40164026751963));
#32743=CARTESIAN_POINT('Ctrl Pts',(4.85068927010198,-193.818984254242,8.4016402675109));
#32744=CARTESIAN_POINT('Ctrl Pts',(7.27603390513785,-193.643984254242,4.20082013374672));
#32745=CARTESIAN_POINT('Ctrl Pts',(9.70137854017372,-193.468984254242,-1.74689612655491E-11));
#32746=CARTESIAN_POINT('Ctrl Pts',(7.27603390512273,-193.293984254242,-4.20082013377291));
#32747=CARTESIAN_POINT('Ctrl Pts',(4.85068927007173,-193.118984254242,-8.40164026752836));
#32748=CARTESIAN_POINT('Ctrl Pts',(-1.51301075899711E-11,-192.943984254242,
-8.40164026751963));
#32749=CARTESIAN_POINT('Ctrl Pts',(-4.85068927010199,-192.768984254242,
-8.4016402675109));
#32750=CARTESIAN_POINT('Ctrl Pts',(-7.27603390513785,-192.593984254242,
-4.20082013374671));
#32751=CARTESIAN_POINT('Ctrl Pts',(-9.70137854017372,-192.418984254242,
1.74701493417668E-11));
#32752=CARTESIAN_POINT('Ctrl Pts',(-7.27603390512272,-192.243984254242,
4.20082013377292));
#32753=CARTESIAN_POINT('Ctrl Pts',(-4.85068927007173,-192.068984254242,
8.40164026752836));
#32754=CARTESIAN_POINT('Ctrl Pts',(1.5129078685785E-11,-191.893984254242,
8.40164026751963));
#32755=CARTESIAN_POINT('Ctrl Pts',(4.85068927010198,-191.718984254242,8.4016402675109));
#32756=CARTESIAN_POINT('Ctrl Pts',(7.27603390513785,-191.543984254242,4.20082013374672));
#32757=CARTESIAN_POINT('Ctrl Pts',(9.70137854017372,-191.368984254242,-1.74689612655491E-11));
#32758=CARTESIAN_POINT('Ctrl Pts',(7.27603390512273,-191.193984254242,-4.20082013377291));
#32759=CARTESIAN_POINT('Ctrl Pts',(4.85068927007173,-191.018984254242,-8.40164026752836));
#32760=CARTESIAN_POINT('Ctrl Pts',(-1.51301075899711E-11,-190.843984254242,
-8.40164026751963));
#32761=CARTESIAN_POINT('Ctrl Pts',(-4.85068927010199,-190.668984254242,
-8.4016402675109));
#32762=CARTESIAN_POINT('Ctrl Pts',(-7.27603390513785,-190.493984254242,
-4.20082013374671));
#32763=CARTESIAN_POINT('Ctrl Pts',(-9.70137854017372,-190.318984254242,
1.74701493417668E-11));
#32764=CARTESIAN_POINT('Ctrl Pts',(-7.27603390512272,-190.143984254242,
4.20082013377292));
#32765=CARTESIAN_POINT('Ctrl Pts',(-4.85068927007173,-189.968984254242,
8.40164026752836));
#32766=CARTESIAN_POINT('Ctrl Pts',(1.5129078685785E-11,-189.793984254242,
8.40164026751963));
#32767=CARTESIAN_POINT('Ctrl Pts',(4.85068927010198,-189.618984254242,8.4016402675109));
#32768=CARTESIAN_POINT('Ctrl Pts',(7.27603390513785,-189.443984254242,4.20082013374672));
#32769=CARTESIAN_POINT('Ctrl Pts',(9.70137854017372,-189.268984254242,-1.74689612655491E-11));
#32770=CARTESIAN_POINT('Ctrl Pts',(7.27603390512273,-189.093984254242,-4.20082013377291));
#32771=CARTESIAN_POINT('Ctrl Pts',(4.85068927007173,-188.918984254242,-8.40164026752836));
#32772=CARTESIAN_POINT('Ctrl Pts',(-1.51301075899711E-11,-188.743984254242,
-8.40164026751963));
#32773=CARTESIAN_POINT('Ctrl Pts',(-4.85068927010199,-188.568984254242,
-8.4016402675109));
#32774=CARTESIAN_POINT('Ctrl Pts',(-7.27603390513785,-188.393984254242,
-4.20082013374671));
#32775=CARTESIAN_POINT('Ctrl Pts',(-9.70137854017372,-188.218984254242,
1.74701493417668E-11));
#32776=CARTESIAN_POINT('Ctrl Pts',(-7.27603390512272,-188.043984254242,
4.20082013377292));
#32777=CARTESIAN_POINT('Ctrl Pts',(-4.85068927007173,-187.868984254242,
8.40164026752836));
#32778=CARTESIAN_POINT('Ctrl Pts',(1.5129078685785E-11,-187.693984254242,
8.40164026751963));
#32779=CARTESIAN_POINT('Ctrl Pts',(4.85068927010198,-187.518984254242,8.4016402675109));
#32780=CARTESIAN_POINT('Ctrl Pts',(7.27603390513785,-187.343984254242,4.20082013374672));
#32781=CARTESIAN_POINT('Ctrl Pts',(9.70137854017372,-187.168984254242,-1.74689612655491E-11));
#32782=CARTESIAN_POINT('Ctrl Pts',(7.27603390512273,-186.993984254242,-4.20082013377291));
#32783=CARTESIAN_POINT('Ctrl Pts',(4.85068927007173,-186.818984254242,-8.40164026752836));
#32784=CARTESIAN_POINT('Ctrl Pts',(-1.51301075899711E-11,-186.643984254242,
-8.40164026751963));
#32785=CARTESIAN_POINT('Ctrl Pts',(-4.85068927010199,-186.468984254242,
-8.4016402675109));
#32786=CARTESIAN_POINT('Ctrl Pts',(-7.27603390513785,-186.293984254242,
-4.20082013374671));
#32787=CARTESIAN_POINT('Ctrl Pts',(-9.70137854017372,-186.118984254242,
1.74701493417668E-11));
#32788=CARTESIAN_POINT('Ctrl Pts',(-7.27603390512272,-185.943984254242,
4.20082013377292));
#32789=CARTESIAN_POINT('Ctrl Pts',(-4.85068927007173,-185.768984254242,
8.40164026752836));
#32790=CARTESIAN_POINT('Ctrl Pts',(1.5129078685785E-11,-185.593984254242,
8.40164026751963));
#32791=CARTESIAN_POINT('Ctrl Pts',(4.85068927010198,-185.418984254242,8.4016402675109));
#32792=CARTESIAN_POINT('Ctrl Pts',(7.27603390513785,-185.243984254242,4.20082013374672));
#32793=CARTESIAN_POINT('Ctrl Pts',(9.70137854017372,-185.068984254242,-1.74689612655491E-11));
#32794=CARTESIAN_POINT('Ctrl Pts',(7.27603390512273,-184.893984254242,-4.20082013377291));
#32795=CARTESIAN_POINT('Ctrl Pts',(4.85068927007173,-184.718984254242,-8.40164026752836));
#32796=CARTESIAN_POINT('Ctrl Pts',(-1.51301075899711E-11,-184.543984254242,
-8.40164026751963));
#32797=CARTESIAN_POINT('Ctrl Pts',(-4.85068927010199,-184.368984254242,
-8.4016402675109));
#32798=CARTESIAN_POINT('Ctrl Pts',(-7.27603390513785,-184.193984254242,
-4.20082013374671));
#32799=CARTESIAN_POINT('Ctrl Pts',(-9.70137854017372,-184.018984254242,
1.74701493417668E-11));
#32800=CARTESIAN_POINT('Ctrl Pts',(-7.27603390512272,-183.843984254242,
4.20082013377292));
#32801=CARTESIAN_POINT('Ctrl Pts',(-4.85068927007173,-183.668984254242,
8.40164026752836));
#32802=CARTESIAN_POINT('Ctrl Pts',(1.5129078685785E-11,-183.493984254242,
8.40164026751963));
#32803=CARTESIAN_POINT('Ctrl Pts',(4.85068927010198,-183.318984254242,8.4016402675109));
#32804=CARTESIAN_POINT('Ctrl Pts',(7.27603390513785,-183.143984254242,4.20082013374672));
#32805=CARTESIAN_POINT('Ctrl Pts',(9.70137854017372,-182.968984254242,-1.74689612655491E-11));
#32806=CARTESIAN_POINT('Ctrl Pts',(7.27603390512273,-182.793984254242,-4.20082013377291));
#32807=CARTESIAN_POINT('Ctrl Pts',(4.85068927007173,-182.618984254242,-8.40164026752836));
#32808=CARTESIAN_POINT('Ctrl Pts',(-1.51301075899711E-11,-182.443984254242,
-8.40164026751963));
#32809=CARTESIAN_POINT('Ctrl Pts',(-4.85068927010199,-182.268984254242,
-8.4016402675109));
#32810=CARTESIAN_POINT('Ctrl Pts',(-7.27603390513785,-182.093984254242,
-4.20082013374671));
#32811=CARTESIAN_POINT('Ctrl Pts',(-9.70137854017372,-181.918984254242,
1.74701493417668E-11));
#32812=CARTESIAN_POINT('Ctrl Pts',(-7.27603390512272,-181.743984254242,
4.20082013377292));
#32813=CARTESIAN_POINT('Ctrl Pts',(-4.85068927007173,-181.568984254242,
8.40164026752836));
#32814=CARTESIAN_POINT('Ctrl Pts',(1.5129078685785E-11,-181.393984254242,
8.40164026751963));
#32815=CARTESIAN_POINT('Ctrl Pts',(4.85068927010198,-181.218984254242,8.4016402675109));
#32816=CARTESIAN_POINT('Ctrl Pts',(7.27603390513785,-181.043984254242,4.20082013374672));
#32817=CARTESIAN_POINT('Ctrl Pts',(9.70137854017372,-180.868984254242,-1.74689612655491E-11));
#32818=CARTESIAN_POINT('Ctrl Pts',(7.27603390512273,-180.693984254242,-4.20082013377291));
#32819=CARTESIAN_POINT('Ctrl Pts',(4.85068927007173,-180.518984254242,-8.40164026752836));
#32820=CARTESIAN_POINT('Ctrl Pts',(-1.51301075899711E-11,-180.343984254242,
-8.40164026751963));
#32821=CARTESIAN_POINT('Ctrl Pts',(-4.85068927010199,-180.168984254242,
-8.4016402675109));
#32822=CARTESIAN_POINT('Ctrl Pts',(-7.27603390513785,-179.993984254242,
-4.20082013374671));
#32823=CARTESIAN_POINT('Ctrl Pts',(-9.70137854017372,-179.818984254242,
1.74701493417668E-11));
#32824=CARTESIAN_POINT('Ctrl Pts',(-7.27603390512272,-179.643984254242,
4.20082013377292));
#32825=CARTESIAN_POINT('Ctrl Pts',(-4.85068927007173,-179.468984254242,
8.40164026752836));
#32826=CARTESIAN_POINT('Ctrl Pts',(1.5129078685785E-11,-179.293984254242,
8.40164026751963));
#32827=CARTESIAN_POINT('Ctrl Pts',(4.85068927010198,-179.118984254242,8.4016402675109));
#32828=CARTESIAN_POINT('Ctrl Pts',(7.27603390513785,-178.943984254242,4.20082013374672));
#32829=CARTESIAN_POINT('Ctrl Pts',(9.70137854017372,-178.768984254242,-1.74689612655491E-11));
#32830=CARTESIAN_POINT('Ctrl Pts',(7.27603390512273,-178.593984254242,-4.20082013377291));
#32831=CARTESIAN_POINT('Ctrl Pts',(4.85068927007173,-178.418984254242,-8.40164026752836));
#32832=CARTESIAN_POINT('Ctrl Pts',(-1.51301075899711E-11,-178.243984254242,
-8.40164026751963));
#32833=CARTESIAN_POINT('Ctrl Pts',(-4.85068927010199,-178.068984254242,
-8.4016402675109));
#32834=CARTESIAN_POINT('Ctrl Pts',(-7.27603390513785,-177.893984254242,
-4.20082013374671));
#32835=CARTESIAN_POINT('Ctrl Pts',(-9.70137854017372,-177.718984254242,
1.74701493417668E-11));
#32836=CARTESIAN_POINT('Ctrl Pts',(-7.27603390512272,-177.543984254242,
4.20082013377292));
#32837=CARTESIAN_POINT('Ctrl Pts',(-4.85068927007173,-177.368984254242,
8.40164026752836));
#32838=CARTESIAN_POINT('Ctrl Pts',(1.5129078685785E-11,-177.193984254242,
8.40164026751963));
#32839=CARTESIAN_POINT('Ctrl Pts',(4.85068927010198,-177.018984254242,8.4016402675109));
#32840=CARTESIAN_POINT('Ctrl Pts',(7.27603390513785,-176.843984254242,4.20082013374672));
#32841=CARTESIAN_POINT('Ctrl Pts',(9.70137854017372,-176.668984254242,-1.74689612655491E-11));
#32842=CARTESIAN_POINT('Ctrl Pts',(7.27603390512273,-176.493984254242,-4.20082013377291));
#32843=CARTESIAN_POINT('Ctrl Pts',(4.85068927007173,-176.318984254242,-8.40164026752836));
#32844=CARTESIAN_POINT('Ctrl Pts',(-1.51301075899711E-11,-176.143984254242,
-8.40164026751963));
#32845=CARTESIAN_POINT('Ctrl Pts',(-4.85068927010199,-175.968984254242,
-8.4016402675109));
#32846=CARTESIAN_POINT('Ctrl Pts',(-7.27603390513785,-175.793984254242,
-4.20082013374671));
#32847=CARTESIAN_POINT('Ctrl Pts',(-9.70137854017372,-175.618984254242,
1.74701493417668E-11));
#32848=CARTESIAN_POINT('Ctrl Pts',(-7.27603390512272,-175.443984254242,
4.20082013377292));
#32849=CARTESIAN_POINT('Ctrl Pts',(-4.85068927007173,-175.268984254242,
8.40164026752836));
#32850=CARTESIAN_POINT('Ctrl Pts',(1.5129078685785E-11,-175.093984254242,
8.40164026751963));
#32851=CARTESIAN_POINT('Ctrl Pts',(4.85068927010198,-174.918984254242,8.4016402675109));
#32852=CARTESIAN_POINT('Ctrl Pts',(7.27603390513785,-174.743984254242,4.20082013374672));
#32853=CARTESIAN_POINT('Ctrl Pts',(9.70137854017372,-174.568984254242,-1.74689612655491E-11));
#32854=CARTESIAN_POINT('Ctrl Pts',(7.27603390512273,-174.393984254242,-4.20082013377291));
#32855=CARTESIAN_POINT('Ctrl Pts',(4.85068927007173,-174.218984254242,-8.40164026752836));
#32856=CARTESIAN_POINT('Ctrl Pts',(-1.51301075899711E-11,-174.043984254242,
-8.40164026751963));
#32857=CARTESIAN_POINT('Ctrl Pts',(-4.85068927010199,-173.868984254242,
-8.4016402675109));
#32858=CARTESIAN_POINT('Ctrl Pts',(-7.27603390513785,-173.693984254242,
-4.20082013374671));
#32859=CARTESIAN_POINT('Ctrl Pts',(-9.70137854017372,-173.518984254242,
1.74701493417668E-11));
#32860=CARTESIAN_POINT('Ctrl Pts',(-7.27603390512272,-173.343984254242,
4.20082013377292));
#32861=CARTESIAN_POINT('Ctrl Pts',(-4.85068927007173,-173.168984254242,
8.40164026752836));
#32862=CARTESIAN_POINT('Ctrl Pts',(1.5129078685785E-11,-172.993984254242,
8.40164026751963));
#32863=CARTESIAN_POINT('Ctrl Pts',(4.85068927010198,-172.818984254242,8.4016402675109));
#32864=CARTESIAN_POINT('Ctrl Pts',(7.27603390513785,-172.643984254242,4.20082013374672));
#32865=CARTESIAN_POINT('Ctrl Pts',(9.70137854017372,-172.468984254242,-1.74689612655491E-11));
#32866=CARTESIAN_POINT('Ctrl Pts',(7.27603390512273,-172.293984254242,-4.20082013377291));
#32867=CARTESIAN_POINT('Ctrl Pts',(4.85068927007173,-172.118984254242,-8.40164026752836));
#32868=CARTESIAN_POINT('Ctrl Pts',(-1.51301075899711E-11,-171.943984254242,
-8.40164026751963));
#32869=CARTESIAN_POINT('Ctrl Pts',(-4.85068927010199,-171.768984254242,
-8.4016402675109));
#32870=CARTESIAN_POINT('Ctrl Pts',(-7.27603390513785,-171.593984254242,
-4.20082013374671));
#32871=CARTESIAN_POINT('Ctrl Pts',(-9.70137854017372,-171.418984254242,
1.74701493417668E-11));
#32872=CARTESIAN_POINT('Ctrl Pts',(-7.27603390512272,-171.243984254242,
4.20082013377292));
#32873=CARTESIAN_POINT('Ctrl Pts',(-4.85068927007173,-171.068984254242,
8.40164026752836));
#32874=CARTESIAN_POINT('Ctrl Pts',(1.5129078685785E-11,-170.893984254242,
8.40164026751963));
#32875=CARTESIAN_POINT('Ctrl Pts',(4.85068927010198,-170.718984254242,8.4016402675109));
#32876=CARTESIAN_POINT('Ctrl Pts',(7.27603390513785,-170.543984254242,4.20082013374672));
#32877=CARTESIAN_POINT('Ctrl Pts',(9.70137854017372,-170.368984254242,-1.74689612655491E-11));
#32878=CARTESIAN_POINT('Ctrl Pts',(7.27603390512273,-170.193984254242,-4.20082013377291));
#32879=CARTESIAN_POINT('Ctrl Pts',(4.85068927007173,-170.018984254242,-8.40164026752836));
#32880=CARTESIAN_POINT('Ctrl Pts',(-1.51301075899711E-11,-169.843984254242,
-8.40164026751963));
#32881=CARTESIAN_POINT('Ctrl Pts',(-4.85068927010199,-169.668984254242,
-8.4016402675109));
#32882=CARTESIAN_POINT('Ctrl Pts',(-7.27603390513785,-169.493984254242,
-4.20082013374671));
#32883=CARTESIAN_POINT('Ctrl Pts',(-9.70137854017372,-169.318984254242,
1.74701493417668E-11));
#32884=CARTESIAN_POINT('Ctrl Pts',(-7.27603390512272,-169.143984254242,
4.20082013377292));
#32885=CARTESIAN_POINT('Ctrl Pts',(-4.85068927007173,-168.968984254242,
8.40164026752836));
#32886=CARTESIAN_POINT('Ctrl Pts',(1.5129078685785E-11,-168.793984254242,
8.40164026751963));
#32887=CARTESIAN_POINT('Ctrl Pts',(4.85068927010198,-168.618984254242,8.4016402675109));
#32888=CARTESIAN_POINT('Ctrl Pts',(7.27603390513785,-168.443984254242,4.20082013374672));
#32889=CARTESIAN_POINT('Ctrl Pts',(9.70137854017372,-168.268984254242,-1.74689612655491E-11));
#32890=CARTESIAN_POINT('Ctrl Pts',(7.27603390512273,-168.093984254242,-4.20082013377291));
#32891=CARTESIAN_POINT('Ctrl Pts',(4.85068927007173,-167.918984254242,-8.40164026752836));
#32892=CARTESIAN_POINT('Ctrl Pts',(-1.51301075899711E-11,-167.743984254242,
-8.40164026751963));
#32893=CARTESIAN_POINT('Ctrl Pts',(-4.85068927010199,-167.568984254242,
-8.4016402675109));
#32894=CARTESIAN_POINT('Ctrl Pts',(-7.27603390513785,-167.393984254242,
-4.20082013374671));
#32895=CARTESIAN_POINT('Ctrl Pts',(-9.70137854017372,-167.218984254242,
1.74701493417668E-11));
#32896=CARTESIAN_POINT('Ctrl Pts',(-7.27603390512272,-167.043984254242,
4.20082013377292));
#32897=CARTESIAN_POINT('Ctrl Pts',(-4.85068927007173,-166.868984254242,
8.40164026752836));
#32898=CARTESIAN_POINT('Ctrl Pts',(1.5129078685785E-11,-166.693984254242,
8.40164026751963));
#32899=CARTESIAN_POINT('Ctrl Pts',(4.85068927010198,-166.518984254242,8.4016402675109));
#32900=CARTESIAN_POINT('Ctrl Pts',(7.27603390513785,-166.343984254242,4.20082013374672));
#32901=CARTESIAN_POINT('Ctrl Pts',(9.70137854017372,-166.168984254242,-1.74689612655491E-11));
#32902=CARTESIAN_POINT('Ctrl Pts',(7.27603390512273,-165.993984254242,-4.20082013377291));
#32903=CARTESIAN_POINT('Ctrl Pts',(4.85068927007173,-165.818984254242,-8.40164026752836));
#32904=CARTESIAN_POINT('Ctrl Pts',(-1.51301075899711E-11,-165.643984254242,
-8.40164026751963));
#32905=CARTESIAN_POINT('Ctrl Pts',(-4.85068927010199,-165.468984254242,
-8.4016402675109));
#32906=CARTESIAN_POINT('Ctrl Pts',(-7.27603390513785,-165.293984254242,
-4.20082013374671));
#32907=CARTESIAN_POINT('Ctrl Pts',(-9.70137854017372,-165.118984254242,
1.74701493417668E-11));
#32908=CARTESIAN_POINT('Ctrl Pts',(-7.27603390512272,-164.943984254242,
4.20082013377292));
#32909=CARTESIAN_POINT('Ctrl Pts',(-4.85068927007173,-164.768984254242,
8.40164026752836));
#32910=CARTESIAN_POINT('Ctrl Pts',(1.5129078685785E-11,-164.593984254242,
8.40164026751963));
#32911=CARTESIAN_POINT('Ctrl Pts',(4.85068927010198,-164.418984254242,8.4016402675109));
#32912=CARTESIAN_POINT('Ctrl Pts',(7.27603390513785,-164.243984254242,4.20082013374672));
#32913=CARTESIAN_POINT('Ctrl Pts',(9.70137854017372,-164.068984254242,-1.74689612655491E-11));
#32914=CARTESIAN_POINT('Ctrl Pts',(7.27603390512273,-163.893984254242,-4.20082013377291));
#32915=CARTESIAN_POINT('Ctrl Pts',(4.85068927007173,-163.718984254242,-8.40164026752836));
#32916=CARTESIAN_POINT('Ctrl Pts',(-1.51301075899711E-11,-163.543984254242,
-8.40164026751963));
#32917=CARTESIAN_POINT('Ctrl Pts',(-4.85068927010199,-163.368984254242,
-8.4016402675109));
#32918=CARTESIAN_POINT('Ctrl Pts',(-7.27603390513785,-163.193984254242,
-4.20082013374671));
#32919=CARTESIAN_POINT('Ctrl Pts',(-9.70137854017372,-163.018984254242,
1.74701493417668E-11));
#32920=CARTESIAN_POINT('Ctrl Pts',(-7.27603390512272,-162.843984254242,
4.20082013377292));
#32921=CARTESIAN_POINT('Ctrl Pts',(-4.85068927007173,-162.668984254242,
8.40164026752836));
#32922=CARTESIAN_POINT('Ctrl Pts',(1.5129078685785E-11,-162.493984254242,
8.40164026751963));
#32923=CARTESIAN_POINT('Ctrl Pts',(4.85068927010198,-162.318984254242,8.4016402675109));
#32924=CARTESIAN_POINT('Ctrl Pts',(7.27603390513785,-162.143984254242,4.20082013374672));
#32925=CARTESIAN_POINT('Ctrl Pts',(9.70137854017372,-161.968984254242,-1.74689612655491E-11));
#32926=CARTESIAN_POINT('Ctrl Pts',(7.27603390512273,-161.793984254242,-4.20082013377291));
#32927=CARTESIAN_POINT('Ctrl Pts',(4.85068927007173,-161.618984254242,-8.40164026752836));
#32928=CARTESIAN_POINT('Ctrl Pts',(-1.51301075899711E-11,-161.443984254242,
-8.40164026751963));
#32929=CARTESIAN_POINT('Ctrl Pts',(-4.85068927010199,-161.268984254242,
-8.4016402675109));
#32930=CARTESIAN_POINT('Ctrl Pts',(-7.27603390513785,-161.093984254242,
-4.20082013374671));
#32931=CARTESIAN_POINT('Ctrl Pts',(-9.70137854017372,-160.918984254242,
1.74701493417668E-11));
#32932=CARTESIAN_POINT('Ctrl Pts',(-7.27603390512272,-160.743984254242,
4.20082013377292));
#32933=CARTESIAN_POINT('Ctrl Pts',(-4.85068927007173,-160.568984254242,
8.40164026752836));
#32934=CARTESIAN_POINT('Ctrl Pts',(1.5129078685785E-11,-160.393984254242,
8.40164026751963));
#32935=CARTESIAN_POINT('Ctrl Pts',(4.85068927010198,-160.218984254242,8.4016402675109));
#32936=CARTESIAN_POINT('Ctrl Pts',(7.27603390513785,-160.043984254242,4.20082013374672));
#32937=CARTESIAN_POINT('Ctrl Pts',(9.70137854017372,-159.868984254242,-1.74689612655491E-11));
#32938=CARTESIAN_POINT('Ctrl Pts',(7.27603390512273,-159.693984254242,-4.20082013377291));
#32939=CARTESIAN_POINT('Ctrl Pts',(4.85068927007173,-159.518984254242,-8.40164026752836));
#32940=CARTESIAN_POINT('Ctrl Pts',(-1.51301075899711E-11,-159.343984254242,
-8.40164026751963));
#32941=CARTESIAN_POINT('Ctrl Pts',(-4.85068927010199,-159.168984254242,
-8.4016402675109));
#32942=CARTESIAN_POINT('Ctrl Pts',(-7.27603390513785,-158.993984254242,
-4.20082013374671));
#32943=CARTESIAN_POINT('Ctrl Pts',(-9.70137854017372,-158.818984254242,
1.74701493417668E-11));
#32944=CARTESIAN_POINT('Ctrl Pts',(-7.27603390512272,-158.643984254242,
4.20082013377292));
#32945=CARTESIAN_POINT('Ctrl Pts',(-4.85068927007173,-158.468984254242,
8.40164026752836));
#32946=CARTESIAN_POINT('Ctrl Pts',(1.5129078685785E-11,-158.293984254242,
8.40164026751963));
#32947=CARTESIAN_POINT('Ctrl Pts',(4.85068927010198,-158.118984254242,8.4016402675109));
#32948=CARTESIAN_POINT('Ctrl Pts',(7.27603390513785,-157.943984254242,4.20082013374672));
#32949=CARTESIAN_POINT('Ctrl Pts',(9.70137854017372,-157.768984254242,-1.74689612655491E-11));
#32950=CARTESIAN_POINT('Ctrl Pts',(7.27603390512273,-157.593984254242,-4.20082013377291));
#32951=CARTESIAN_POINT('Ctrl Pts',(4.85068927007173,-157.418984254242,-8.40164026752836));
#32952=CARTESIAN_POINT('Ctrl Pts',(-1.51301075899711E-11,-157.243984254242,
-8.40164026751963));
#32953=CARTESIAN_POINT('Ctrl Pts',(-4.85068927010199,-157.068984254242,
-8.4016402675109));
#32954=CARTESIAN_POINT('Ctrl Pts',(-7.27603390513785,-156.893984254242,
-4.20082013374671));
#32955=CARTESIAN_POINT('Ctrl Pts',(-9.70137854017372,-156.718984254242,
1.74701493417668E-11));
#32956=CARTESIAN_POINT('Ctrl Pts',(-7.27603390512272,-156.543984254242,
4.20082013377292));
#32957=CARTESIAN_POINT('Ctrl Pts',(-4.85068927007173,-156.368984254242,
8.40164026752836));
#32958=CARTESIAN_POINT('Ctrl Pts',(1.5129078685785E-11,-156.193984254242,
8.40164026751963));
#32959=CARTESIAN_POINT('Ctrl Pts',(4.85068927010198,-156.018984254242,8.4016402675109));
#32960=CARTESIAN_POINT('Ctrl Pts',(7.27603390513785,-155.843984254242,4.20082013374672));
#32961=CARTESIAN_POINT('Ctrl Pts',(9.70137854017372,-155.668984254242,-1.74689612655491E-11));
#32962=CARTESIAN_POINT('Ctrl Pts',(7.27603390512273,-155.493984254242,-4.20082013377291));
#32963=CARTESIAN_POINT('Ctrl Pts',(4.85068927007173,-155.318984254242,-8.40164026752836));
#32964=CARTESIAN_POINT('Ctrl Pts',(-1.51301075899711E-11,-155.143984254242,
-8.40164026751963));
#32965=CARTESIAN_POINT('Ctrl Pts',(-4.85068927010199,-154.968984254242,
-8.4016402675109));
#32966=CARTESIAN_POINT('Ctrl Pts',(-7.27603390513785,-154.793984254242,
-4.20082013374671));
#32967=CARTESIAN_POINT('Ctrl Pts',(-9.70137854017372,-154.618984254242,
1.74701493417668E-11));
#32968=CARTESIAN_POINT('Ctrl Pts',(-7.27603390512272,-154.443984254242,
4.20082013377292));
#32969=CARTESIAN_POINT('Ctrl Pts',(-4.85068927007173,-154.268984254242,
8.40164026752836));
#32970=CARTESIAN_POINT('Ctrl Pts',(1.5129078685785E-11,-154.093984254242,
8.40164026751963));
#32971=CARTESIAN_POINT('Ctrl Pts',(4.85068927010198,-153.918984254242,8.4016402675109));
#32972=CARTESIAN_POINT('Ctrl Pts',(7.27603390513785,-153.743984254242,4.20082013374672));
#32973=CARTESIAN_POINT('Ctrl Pts',(9.70137854017372,-153.568984254242,-1.74689612655491E-11));
#32974=CARTESIAN_POINT('Ctrl Pts',(7.27603390512273,-153.393984254242,-4.20082013377291));
#32975=CARTESIAN_POINT('Ctrl Pts',(4.85068927007173,-153.218984254242,-8.40164026752836));
#32976=CARTESIAN_POINT('Ctrl Pts',(-1.51301075899711E-11,-153.043984254242,
-8.40164026751963));
#32977=CARTESIAN_POINT('Ctrl Pts',(-4.85068927010199,-152.868984254242,
-8.4016402675109));
#32978=CARTESIAN_POINT('Ctrl Pts',(-7.27603390513785,-152.693984254242,
-4.20082013374671));
#32979=CARTESIAN_POINT('Ctrl Pts',(-9.70137854017372,-152.518984254242,
1.74701493417668E-11));
#32980=CARTESIAN_POINT('Ctrl Pts',(-7.27603390512272,-152.343984254242,
4.20082013377292));
#32981=CARTESIAN_POINT('Ctrl Pts',(-4.85068927007173,-152.168984254242,
8.40164026752836));
#32982=CARTESIAN_POINT('Ctrl Pts',(1.5129078685785E-11,-151.993984254242,
8.40164026751963));
#32983=CARTESIAN_POINT('Ctrl Pts',(4.85068927010198,-151.818984254242,8.4016402675109));
#32984=CARTESIAN_POINT('Ctrl Pts',(7.27603390513785,-151.643984254242,4.20082013374672));
#32985=CARTESIAN_POINT('Ctrl Pts',(9.70137854017372,-151.468984254242,-1.74689612655491E-11));
#32986=CARTESIAN_POINT('Ctrl Pts',(7.27603390512273,-151.293984254242,-4.20082013377291));
#32987=CARTESIAN_POINT('Ctrl Pts',(4.85068927007173,-151.118984254242,-8.40164026752836));
#32988=CARTESIAN_POINT('Ctrl Pts',(-1.51301075899711E-11,-150.943984254242,
-8.40164026751963));
#32989=CARTESIAN_POINT('Ctrl Pts',(-4.85068927010199,-150.768984254242,
-8.4016402675109));
#32990=CARTESIAN_POINT('Ctrl Pts',(-7.27603390513785,-150.593984254242,
-4.20082013374671));
#32991=CARTESIAN_POINT('Ctrl Pts',(-9.70137854017372,-150.418984254242,
1.74701493417668E-11));
#32992=CARTESIAN_POINT('Ctrl Pts',(-7.27603390512272,-150.243984254242,
4.20082013377292));
#32993=CARTESIAN_POINT('Ctrl Pts',(-4.85068927007173,-150.068984254242,
8.40164026752836));
#32994=CARTESIAN_POINT('Ctrl Pts',(1.5129078685785E-11,-149.893984254242,
8.40164026751963));
#32995=CARTESIAN_POINT('Ctrl Pts',(4.85068927010198,-149.718984254242,8.4016402675109));
#32996=CARTESIAN_POINT('Ctrl Pts',(7.27603390513785,-149.543984254242,4.20082013374672));
#32997=CARTESIAN_POINT('Ctrl Pts',(9.70137854017372,-149.368984254242,-1.74689612655491E-11));
#32998=CARTESIAN_POINT('Ctrl Pts',(7.27603390512273,-149.193984254242,-4.20082013377291));
#32999=CARTESIAN_POINT('Ctrl Pts',(4.85068927007173,-149.018984254242,-8.40164026752836));
#33000=CARTESIAN_POINT('Ctrl Pts',(-1.51301075899711E-11,-148.843984254242,
-8.40164026751963));
#33001=CARTESIAN_POINT('Ctrl Pts',(-4.85068927010199,-148.668984254242,
-8.4016402675109));
#33002=CARTESIAN_POINT('Ctrl Pts',(-7.27603390513785,-148.493984254242,
-4.20082013374671));
#33003=CARTESIAN_POINT('Ctrl Pts',(-9.70137854017372,-148.318984254242,
1.74701493417668E-11));
#33004=CARTESIAN_POINT('Ctrl Pts',(-7.27603390512272,-148.143984254242,
4.20082013377292));
#33005=CARTESIAN_POINT('Ctrl Pts',(-4.85068927007173,-147.968984254242,
8.40164026752836));
#33006=CARTESIAN_POINT('Ctrl Pts',(1.5129078685785E-11,-147.793984254242,
8.40164026751963));
#33007=CARTESIAN_POINT('Ctrl Pts',(4.85068927010198,-147.618984254242,8.4016402675109));
#33008=CARTESIAN_POINT('Ctrl Pts',(7.27603390513785,-147.443984254242,4.20082013374672));
#33009=CARTESIAN_POINT('Ctrl Pts',(9.70137854017372,-147.268984254242,-1.74689612655491E-11));
#33010=CARTESIAN_POINT('Ctrl Pts',(7.27603390512273,-147.093984254242,-4.20082013377291));
#33011=CARTESIAN_POINT('Ctrl Pts',(4.85068927007173,-146.918984254242,-8.40164026752836));
#33012=CARTESIAN_POINT('Ctrl Pts',(-1.51301075899711E-11,-146.743984254242,
-8.40164026751963));
#33013=CARTESIAN_POINT('Ctrl Pts',(-4.85068927010199,-146.568984254242,
-8.4016402675109));
#33014=CARTESIAN_POINT('Ctrl Pts',(-7.27603390513785,-146.393984254242,
-4.20082013374671));
#33015=CARTESIAN_POINT('Ctrl Pts',(-9.70137854017372,-146.218984254242,
1.74701493417668E-11));
#33016=CARTESIAN_POINT('Ctrl Pts',(-7.27603390512272,-146.043984254242,
4.20082013377292));
#33017=CARTESIAN_POINT('Ctrl Pts',(-4.85068927007173,-145.868984254242,
8.40164026752836));
#33018=CARTESIAN_POINT('Ctrl Pts',(1.5129078685785E-11,-145.693984254242,
8.40164026751963));
#33019=CARTESIAN_POINT('Ctrl Pts',(4.85068927010198,-145.518984254242,8.4016402675109));
#33020=CARTESIAN_POINT('Ctrl Pts',(7.27603390513785,-145.343984254242,4.20082013374672));
#33021=CARTESIAN_POINT('Ctrl Pts',(9.70137854017372,-145.168984254242,-1.74689612655491E-11));
#33022=CARTESIAN_POINT('Ctrl Pts',(7.27603390512273,-144.993984254242,-4.20082013377291));
#33023=CARTESIAN_POINT('Ctrl Pts',(4.85068927007173,-144.818984254242,-8.40164026752836));
#33024=CARTESIAN_POINT('Ctrl Pts',(-1.51301075899711E-11,-144.643984254242,
-8.40164026751963));
#33025=CARTESIAN_POINT('Ctrl Pts',(-4.85068927010199,-144.468984254242,
-8.4016402675109));
#33026=CARTESIAN_POINT('Ctrl Pts',(-7.27603390513785,-144.293984254242,
-4.20082013374671));
#33027=CARTESIAN_POINT('Ctrl Pts',(-9.70137854017372,-144.118984254242,
1.74701493417668E-11));
#33028=CARTESIAN_POINT('Ctrl Pts',(-7.27603390512272,-143.943984254242,
4.20082013377292));
#33029=CARTESIAN_POINT('Ctrl Pts',(-4.85068927007173,-143.768984254242,
8.40164026752836));
#33030=CARTESIAN_POINT('Ctrl Pts',(1.5129078685785E-11,-143.593984254242,
8.40164026751963));
#33031=CARTESIAN_POINT('Ctrl Pts',(4.85068927010198,-143.418984254242,8.4016402675109));
#33032=CARTESIAN_POINT('Ctrl Pts',(7.27603390513785,-143.243984254242,4.20082013374672));
#33033=CARTESIAN_POINT('Ctrl Pts',(9.70137854017372,-143.068984254242,-1.74689612655491E-11));
#33034=CARTESIAN_POINT('Ctrl Pts',(7.27603390512273,-142.893984254242,-4.20082013377291));
#33035=CARTESIAN_POINT('Ctrl Pts',(4.85068927007173,-142.718984254242,-8.40164026752836));
#33036=CARTESIAN_POINT('Ctrl Pts',(-1.51301075899711E-11,-142.543984254242,
-8.40164026751963));
#33037=CARTESIAN_POINT('Ctrl Pts',(-4.85068927010199,-142.368984254242,
-8.4016402675109));
#33038=CARTESIAN_POINT('Ctrl Pts',(-7.27603390513785,-142.193984254242,
-4.20082013374671));
#33039=CARTESIAN_POINT('Ctrl Pts',(-9.70137854017372,-142.018984254242,
1.74701493417668E-11));
#33040=CARTESIAN_POINT('Ctrl Pts',(-7.27603390512272,-141.843984254242,
4.20082013377292));
#33041=CARTESIAN_POINT('Ctrl Pts',(-4.85068927007173,-141.668984254242,
8.40164026752836));
#33042=CARTESIAN_POINT('Ctrl Pts',(1.5129078685785E-11,-141.493984254242,
8.40164026751963));
#33043=CARTESIAN_POINT('Ctrl Pts',(4.85068927010198,-141.318984254242,8.4016402675109));
#33044=CARTESIAN_POINT('Ctrl Pts',(7.27603390513785,-141.143984254242,4.20082013374672));
#33045=CARTESIAN_POINT('Ctrl Pts',(9.70137854017372,-140.968984254242,-1.74689612655491E-11));
#33046=CARTESIAN_POINT('Ctrl Pts',(7.27603390512273,-140.793984254242,-4.20082013377291));
#33047=CARTESIAN_POINT('Ctrl Pts',(4.85068927007173,-140.618984254242,-8.40164026752836));
#33048=CARTESIAN_POINT('Ctrl Pts',(-1.51301075899711E-11,-140.443984254242,
-8.40164026751963));
#33049=CARTESIAN_POINT('Ctrl Pts',(-4.85068927010199,-140.268984254242,
-8.4016402675109));
#33050=CARTESIAN_POINT('Ctrl Pts',(-7.27603390513785,-140.093984254242,
-4.20082013374671));
#33051=CARTESIAN_POINT('Ctrl Pts',(-9.70137854017372,-139.918984254242,
1.74701493417668E-11));
#33052=CARTESIAN_POINT('Ctrl Pts',(-7.27603390512272,-139.743984254242,
4.20082013377292));
#33053=CARTESIAN_POINT('Ctrl Pts',(-4.85068927007173,-139.568984254242,
8.40164026752836));
#33054=CARTESIAN_POINT('Ctrl Pts',(1.5129078685785E-11,-139.393984254242,
8.40164026751963));
#33055=CARTESIAN_POINT('Ctrl Pts',(4.85068927010198,-139.218984254242,8.4016402675109));
#33056=CARTESIAN_POINT('Ctrl Pts',(7.27603390513785,-139.043984254242,4.20082013374672));
#33057=CARTESIAN_POINT('Ctrl Pts',(9.70137854017372,-138.868984254242,-1.74689612655491E-11));
#33058=CARTESIAN_POINT('Ctrl Pts',(7.27603390512273,-138.693984254242,-4.20082013377291));
#33059=CARTESIAN_POINT('Ctrl Pts',(4.85068927007173,-138.518984254242,-8.40164026752836));
#33060=CARTESIAN_POINT('Ctrl Pts',(-1.51301075899711E-11,-138.343984254242,
-8.40164026751963));
#33061=CARTESIAN_POINT('Ctrl Pts',(-4.85068927010199,-138.168984254242,
-8.4016402675109));
#33062=CARTESIAN_POINT('Ctrl Pts',(-7.27603390513785,-137.993984254242,
-4.20082013374671));
#33063=CARTESIAN_POINT('Ctrl Pts',(-9.70137854017372,-137.818984254242,
1.74701493417668E-11));
#33064=CARTESIAN_POINT('Ctrl Pts',(-7.27603390512272,-137.643984254242,
4.20082013377292));
#33065=CARTESIAN_POINT('Ctrl Pts',(-4.85068927007173,-137.468984254242,
8.40164026752836));
#33066=CARTESIAN_POINT('Ctrl Pts',(1.5129078685785E-11,-137.293984254242,
8.40164026751963));
#33067=CARTESIAN_POINT('Ctrl Pts',(4.85068927010198,-137.118984254242,8.4016402675109));
#33068=CARTESIAN_POINT('Ctrl Pts',(7.27603390513785,-136.943984254242,4.20082013374672));
#33069=CARTESIAN_POINT('Ctrl Pts',(9.70137854017372,-136.768984254242,-1.74689612655491E-11));
#33070=CARTESIAN_POINT('Ctrl Pts',(7.27603390512273,-136.593984254242,-4.20082013377291));
#33071=CARTESIAN_POINT('Ctrl Pts',(4.85068927007173,-136.418984254242,-8.40164026752836));
#33072=CARTESIAN_POINT('Ctrl Pts',(-1.51301075899711E-11,-136.243984254242,
-8.40164026751963));
#33073=CARTESIAN_POINT('Ctrl Pts',(-4.85068927010199,-136.068984254242,
-8.4016402675109));
#33074=CARTESIAN_POINT('Ctrl Pts',(-7.27603390513785,-135.893984254242,
-4.20082013374671));
#33075=CARTESIAN_POINT('Ctrl Pts',(-9.70137854017372,-135.718984254242,
1.74701493417668E-11));
#33076=CARTESIAN_POINT('Ctrl Pts',(-7.27603390512272,-135.543984254242,
4.20082013377292));
#33077=CARTESIAN_POINT('Ctrl Pts',(-4.85068927007173,-135.368984254242,
8.40164026752836));
#33078=CARTESIAN_POINT('Ctrl Pts',(1.5129078685785E-11,-135.193984254242,
8.40164026751963));
#33079=CARTESIAN_POINT('Ctrl Pts',(4.85068927010198,-135.018984254242,8.4016402675109));
#33080=CARTESIAN_POINT('Ctrl Pts',(7.27603390513785,-134.843984254242,4.20082013374672));
#33081=CARTESIAN_POINT('Ctrl Pts',(9.70137854017372,-134.668984254242,-1.74689612655491E-11));
#33082=CARTESIAN_POINT('Ctrl Pts',(7.27603390512273,-134.493984254242,-4.20082013377291));
#33083=CARTESIAN_POINT('Ctrl Pts',(4.85068927007173,-134.318984254242,-8.40164026752836));
#33084=CARTESIAN_POINT('Ctrl Pts',(-1.51301075899711E-11,-134.143984254242,
-8.40164026751963));
#33085=CARTESIAN_POINT('Ctrl Pts',(-4.85068927010199,-133.968984254242,
-8.4016402675109));
#33086=CARTESIAN_POINT('Ctrl Pts',(-7.27603390513785,-133.793984254242,
-4.20082013374671));
#33087=CARTESIAN_POINT('Ctrl Pts',(-9.70137854017372,-133.618984254242,
1.74701493417668E-11));
#33088=CARTESIAN_POINT('Ctrl Pts',(-7.27603390512272,-133.443984254242,
4.20082013377292));
#33089=CARTESIAN_POINT('Ctrl Pts',(-4.85068927007173,-133.268984254242,
8.40164026752836));
#33090=CARTESIAN_POINT('Ctrl Pts',(1.5129078685785E-11,-133.093984254242,
8.40164026751963));
#33091=CARTESIAN_POINT('Ctrl Pts',(4.85068927010198,-132.918984254242,8.4016402675109));
#33092=CARTESIAN_POINT('Ctrl Pts',(7.27603390513785,-132.743984254242,4.20082013374672));
#33093=CARTESIAN_POINT('Ctrl Pts',(9.70137854017372,-132.568984254242,-1.74689612655491E-11));
#33094=CARTESIAN_POINT('Ctrl Pts',(7.27603390512273,-132.393984254242,-4.20082013377291));
#33095=CARTESIAN_POINT('Ctrl Pts',(4.85068927007173,-132.218984254242,-8.40164026752836));
#33096=CARTESIAN_POINT('Ctrl Pts',(-1.51301075899711E-11,-132.043984254242,
-8.40164026751963));
#33097=CARTESIAN_POINT('Ctrl Pts',(-4.85068927010199,-131.868984254242,
-8.4016402675109));
#33098=CARTESIAN_POINT('Ctrl Pts',(-7.27603390513785,-131.693984254242,
-4.20082013374671));
#33099=CARTESIAN_POINT('Ctrl Pts',(-9.70137854017372,-131.518984254242,
1.74701493417668E-11));
#33100=CARTESIAN_POINT('Ctrl Pts',(-7.27603390512272,-131.343984254242,
4.20082013377292));
#33101=CARTESIAN_POINT('Ctrl Pts',(-4.85068927007173,-131.168984254242,
8.40164026752836));
#33102=CARTESIAN_POINT('Ctrl Pts',(1.5129078685785E-11,-130.993984254242,
8.40164026751963));
#33103=CARTESIAN_POINT('Ctrl Pts',(4.85068927010198,-130.818984254242,8.4016402675109));
#33104=CARTESIAN_POINT('Ctrl Pts',(7.27603390513785,-130.643984254242,4.20082013374672));
#33105=CARTESIAN_POINT('Ctrl Pts',(9.70137854017372,-130.468984254242,-1.74689612655491E-11));
#33106=CARTESIAN_POINT('Ctrl Pts',(7.27603390512273,-130.293984254242,-4.20082013377291));
#33107=CARTESIAN_POINT('Ctrl Pts',(4.85068927007173,-130.118984254242,-8.40164026752836));
#33108=CARTESIAN_POINT('Ctrl Pts',(-1.51301075899711E-11,-129.943984254242,
-8.40164026751963));
#33109=CARTESIAN_POINT('Ctrl Pts',(-4.85068927010199,-129.768984254242,
-8.4016402675109));
#33110=CARTESIAN_POINT('Ctrl Pts',(-7.27603390513785,-129.593984254242,
-4.20082013374671));
#33111=CARTESIAN_POINT('Ctrl Pts',(-9.70137854017372,-129.418984254242,
1.74701493417668E-11));
#33112=CARTESIAN_POINT('Ctrl Pts',(-7.27603390512272,-129.243984254242,
4.20082013377292));
#33113=CARTESIAN_POINT('Ctrl Pts',(-4.85068927007173,-129.068984254242,
8.40164026752836));
#33114=CARTESIAN_POINT('Ctrl Pts',(1.5129078685785E-11,-128.893984254242,
8.40164026751963));
#33115=CARTESIAN_POINT('Ctrl Pts',(4.85068927010198,-128.718984254242,8.4016402675109));
#33116=CARTESIAN_POINT('Ctrl Pts',(7.27603390513785,-128.543984254242,4.20082013374672));
#33117=CARTESIAN_POINT('Ctrl Pts',(9.70137854017372,-128.368984254242,-1.74689612655491E-11));
#33118=CARTESIAN_POINT('Ctrl Pts',(7.27603390512273,-128.193984254242,-4.20082013377291));
#33119=CARTESIAN_POINT('Ctrl Pts',(4.85068927007173,-128.018984254242,-8.40164026752836));
#33120=CARTESIAN_POINT('Ctrl Pts',(-1.51301075899711E-11,-127.843984254242,
-8.40164026751963));
#33121=CARTESIAN_POINT('Ctrl Pts',(-4.85068927010199,-127.668984254242,
-8.4016402675109));
#33122=CARTESIAN_POINT('Ctrl Pts',(-7.27603390513785,-127.493984254242,
-4.20082013374671));
#33123=CARTESIAN_POINT('Ctrl Pts',(-9.70137854017372,-127.318984254242,
1.74701493417668E-11));
#33124=CARTESIAN_POINT('Ctrl Pts',(-7.27603390512272,-127.143984254242,
4.20082013377292));
#33125=CARTESIAN_POINT('Ctrl Pts',(-4.85068927007173,-126.968984254242,
8.40164026752836));
#33126=CARTESIAN_POINT('Ctrl Pts',(1.5129078685785E-11,-126.793984254242,
8.40164026751963));
#33127=CARTESIAN_POINT('Ctrl Pts',(4.85068927010198,-126.618984254242,8.4016402675109));
#33128=CARTESIAN_POINT('Ctrl Pts',(7.27603390513785,-126.443984254242,4.20082013374672));
#33129=CARTESIAN_POINT('Ctrl Pts',(9.70137854017372,-126.268984254242,-1.74689612655491E-11));
#33130=CARTESIAN_POINT('Ctrl Pts',(7.27603390512273,-126.093984254242,-4.20082013377291));
#33131=CARTESIAN_POINT('Ctrl Pts',(4.85068927007173,-125.918984254242,-8.40164026752836));
#33132=CARTESIAN_POINT('Ctrl Pts',(-1.51301075899711E-11,-125.743984254242,
-8.40164026751963));
#33133=CARTESIAN_POINT('Ctrl Pts',(-4.85068927010199,-125.568984254242,
-8.4016402675109));
#33134=CARTESIAN_POINT('Ctrl Pts',(-7.27603390513785,-125.393984254242,
-4.20082013374671));
#33135=CARTESIAN_POINT('Ctrl Pts',(-9.70137854017372,-125.218984254242,
1.74701493417668E-11));
#33136=CARTESIAN_POINT('Ctrl Pts',(-7.27603390512272,-125.043984254242,
4.20082013377292));
#33137=CARTESIAN_POINT('Ctrl Pts',(-4.85068927007173,-124.868984254242,
8.40164026752836));
#33138=CARTESIAN_POINT('Ctrl Pts',(1.5129078685785E-11,-124.693984254242,
8.40164026751963));
#33139=CARTESIAN_POINT('Ctrl Pts',(4.85068927010198,-124.518984254242,8.4016402675109));
#33140=CARTESIAN_POINT('Ctrl Pts',(7.27603390513785,-124.343984254242,4.20082013374672));
#33141=CARTESIAN_POINT('Ctrl Pts',(9.70137854017372,-124.168984254242,-1.74689612655491E-11));
#33142=CARTESIAN_POINT('Ctrl Pts',(7.27603390512273,-123.993984254242,-4.20082013377291));
#33143=CARTESIAN_POINT('Ctrl Pts',(4.85068927007173,-123.818984254242,-8.40164026752836));
#33144=CARTESIAN_POINT('Ctrl Pts',(-1.51301075899711E-11,-123.643984254242,
-8.40164026751963));
#33145=CARTESIAN_POINT('Ctrl Pts',(-4.85068927010199,-123.468984254242,
-8.4016402675109));
#33146=CARTESIAN_POINT('Ctrl Pts',(-7.27603390513785,-123.293984254242,
-4.20082013374671));
#33147=CARTESIAN_POINT('Ctrl Pts',(-9.70137854017372,-123.118984254242,
1.74701493417668E-11));
#33148=CARTESIAN_POINT('Ctrl Pts',(-7.27603390512272,-122.943984254242,
4.20082013377292));
#33149=CARTESIAN_POINT('Ctrl Pts',(-4.85068927007173,-122.768984254242,
8.40164026752836));
#33150=CARTESIAN_POINT('Ctrl Pts',(1.5129078685785E-11,-122.593984254242,
8.40164026751963));
#33151=CARTESIAN_POINT('Ctrl Pts',(4.85068927010198,-122.418984254242,8.4016402675109));
#33152=CARTESIAN_POINT('Ctrl Pts',(7.27603390513785,-122.243984254242,4.20082013374672));
#33153=CARTESIAN_POINT('Ctrl Pts',(9.70137854017372,-122.068984254242,-1.74689612655491E-11));
#33154=CARTESIAN_POINT('Ctrl Pts',(7.27603390512273,-121.893984254242,-4.20082013377291));
#33155=CARTESIAN_POINT('Ctrl Pts',(4.85068927007173,-121.718984254242,-8.40164026752836));
#33156=CARTESIAN_POINT('Ctrl Pts',(-1.51301075899711E-11,-121.543984254242,
-8.40164026751963));
#33157=CARTESIAN_POINT('Ctrl Pts',(-4.85068927010199,-121.368984254242,
-8.4016402675109));
#33158=CARTESIAN_POINT('Ctrl Pts',(-7.27603390513785,-121.193984254242,
-4.20082013374671));
#33159=CARTESIAN_POINT('Ctrl Pts',(-9.70137854017372,-121.018984254242,
1.74701493417668E-11));
#33160=CARTESIAN_POINT('Ctrl Pts',(-7.27603390512272,-120.843984254242,
4.20082013377292));
#33161=CARTESIAN_POINT('Ctrl Pts',(-4.85068927007173,-120.668984254242,
8.40164026752836));
#33162=CARTESIAN_POINT('Ctrl Pts',(1.5129078685785E-11,-120.493984254242,
8.40164026751963));
#33163=CARTESIAN_POINT('Ctrl Pts',(4.85068927010198,-120.318984254242,8.4016402675109));
#33164=CARTESIAN_POINT('Ctrl Pts',(7.27603390513785,-120.143984254242,4.20082013374672));
#33165=CARTESIAN_POINT('Ctrl Pts',(9.70137854017372,-119.968984254242,-1.74689612655491E-11));
#33166=CARTESIAN_POINT('Ctrl Pts',(7.27603390512273,-119.793984254242,-4.20082013377291));
#33167=CARTESIAN_POINT('Ctrl Pts',(4.85068927007173,-119.618984254242,-8.40164026752836));
#33168=CARTESIAN_POINT('Ctrl Pts',(-1.51301075899711E-11,-119.443984254242,
-8.40164026751963));
#33169=CARTESIAN_POINT('Ctrl Pts',(-4.85068927010199,-119.268984254242,
-8.4016402675109));
#33170=CARTESIAN_POINT('Ctrl Pts',(-7.27603390513785,-119.093984254242,
-4.20082013374671));
#33171=CARTESIAN_POINT('Ctrl Pts',(-9.70137854017372,-118.918984254242,
1.74701493417668E-11));
#33172=CARTESIAN_POINT('Ctrl Pts',(-7.27603390512272,-118.743984254242,
4.20082013377292));
#33173=CARTESIAN_POINT('Ctrl Pts',(-4.85068927007173,-118.568984254242,
8.40164026752836));
#33174=CARTESIAN_POINT('Ctrl Pts',(1.5129078685785E-11,-118.393984254242,
8.40164026751963));
#33175=CARTESIAN_POINT('Ctrl Pts',(4.85068927010198,-118.218984254242,8.4016402675109));
#33176=CARTESIAN_POINT('Ctrl Pts',(7.27603390513785,-118.043984254242,4.20082013374672));
#33177=CARTESIAN_POINT('Ctrl Pts',(9.70137854017372,-117.868984254242,-1.74689612655491E-11));
#33178=CARTESIAN_POINT('Ctrl Pts',(7.27603390512273,-117.693984254242,-4.20082013377291));
#33179=CARTESIAN_POINT('Ctrl Pts',(4.85068927007173,-117.518984254242,-8.40164026752836));
#33180=CARTESIAN_POINT('Ctrl Pts',(-1.51301075899711E-11,-117.343984254242,
-8.40164026751963));
#33181=CARTESIAN_POINT('Ctrl Pts',(-4.85068927010199,-117.168984254242,
-8.4016402675109));
#33182=CARTESIAN_POINT('Ctrl Pts',(-7.27603390513785,-116.993984254242,
-4.20082013374671));
#33183=CARTESIAN_POINT('Ctrl Pts',(-9.70137854017372,-116.818984254242,
1.74701493417668E-11));
#33184=CARTESIAN_POINT('Ctrl Pts',(-7.27603390512272,-116.643984254242,
4.20082013377292));
#33185=CARTESIAN_POINT('Ctrl Pts',(-4.85068927007173,-116.468984254242,
8.40164026752836));
#33186=CARTESIAN_POINT('Ctrl Pts',(1.5129078685785E-11,-116.293984254242,
8.40164026751963));
#33187=CARTESIAN_POINT('Ctrl Pts',(4.85068927010198,-116.118984254242,8.4016402675109));
#33188=CARTESIAN_POINT('Ctrl Pts',(7.27603390513785,-115.943984254242,4.20082013374672));
#33189=CARTESIAN_POINT('Ctrl Pts',(9.70137854017372,-115.768984254242,-1.74689612655491E-11));
#33190=CARTESIAN_POINT('Ctrl Pts',(7.27603390512273,-115.593984254242,-4.20082013377291));
#33191=CARTESIAN_POINT('Ctrl Pts',(4.85068927007173,-115.418984254242,-8.40164026752836));
#33192=CARTESIAN_POINT('Ctrl Pts',(-1.51301075899711E-11,-115.243984254242,
-8.40164026751963));
#33193=CARTESIAN_POINT('Ctrl Pts',(-4.85068927010199,-115.068984254242,
-8.4016402675109));
#33194=CARTESIAN_POINT('Ctrl Pts',(-7.27603390513785,-114.893984254242,
-4.20082013374671));
#33195=CARTESIAN_POINT('Ctrl Pts',(-9.70137854017372,-114.718984254242,
1.74701493417668E-11));
#33196=CARTESIAN_POINT('Ctrl Pts',(-7.27603390512272,-114.543984254242,
4.20082013377292));
#33197=CARTESIAN_POINT('Ctrl Pts',(-4.85068927007173,-114.368984254242,
8.40164026752836));
#33198=CARTESIAN_POINT('Ctrl Pts',(1.5129078685785E-11,-114.193984254242,
8.40164026751963));
#33199=CARTESIAN_POINT('Ctrl Pts',(4.85068927010198,-114.018984254242,8.4016402675109));
#33200=CARTESIAN_POINT('Ctrl Pts',(7.27603390513785,-113.843984254242,4.20082013374672));
#33201=CARTESIAN_POINT('Ctrl Pts',(9.70137854017372,-113.668984254242,-1.74689612655491E-11));
#33202=CARTESIAN_POINT('Ctrl Pts',(7.27603390512273,-113.493984254242,-4.20082013377291));
#33203=CARTESIAN_POINT('Ctrl Pts',(4.85068927007173,-113.318984254242,-8.40164026752836));
#33204=CARTESIAN_POINT('Ctrl Pts',(-1.51301075899711E-11,-113.143984254242,
-8.40164026751963));
#33205=CARTESIAN_POINT('Ctrl Pts',(-4.85068927010199,-112.968984254242,
-8.4016402675109));
#33206=CARTESIAN_POINT('Ctrl Pts',(-7.27603390513785,-112.793984254242,
-4.20082013374671));
#33207=CARTESIAN_POINT('Ctrl Pts',(-9.70137854017372,-112.618984254242,
1.74701493417668E-11));
#33208=CARTESIAN_POINT('Ctrl Pts',(-7.27603390512272,-112.443984254242,
4.20082013377292));
#33209=CARTESIAN_POINT('Ctrl Pts',(-4.85068927007173,-112.268984254242,
8.40164026752836));
#33210=CARTESIAN_POINT('Ctrl Pts',(1.5129078685785E-11,-112.093984254242,
8.40164026751963));
#33211=CARTESIAN_POINT('Ctrl Pts',(4.85068927010198,-111.918984254242,8.4016402675109));
#33212=CARTESIAN_POINT('Ctrl Pts',(7.27603390513785,-111.743984254242,4.20082013374672));
#33213=CARTESIAN_POINT('Ctrl Pts',(9.70137854017372,-111.568984254242,-1.74689612655491E-11));
#33214=CARTESIAN_POINT('Ctrl Pts',(7.27603390512273,-111.393984254242,-4.20082013377291));
#33215=CARTESIAN_POINT('Ctrl Pts',(4.85068927007173,-111.218984254242,-8.40164026752836));
#33216=CARTESIAN_POINT('Ctrl Pts',(-1.51301075899711E-11,-111.043984254242,
-8.40164026751963));
#33217=CARTESIAN_POINT('Ctrl Pts',(-4.85068927010199,-110.868984254242,
-8.4016402675109));
#33218=CARTESIAN_POINT('Ctrl Pts',(-7.27603390513785,-110.693984254242,
-4.20082013374671));
#33219=CARTESIAN_POINT('Ctrl Pts',(-9.70137854017372,-110.518984254242,
1.74701493417668E-11));
#33220=CARTESIAN_POINT('Ctrl Pts',(-7.27603390512272,-110.343984254242,
4.20082013377292));
#33221=CARTESIAN_POINT('Ctrl Pts',(-4.85068927007173,-110.168984254242,
8.40164026752836));
#33222=CARTESIAN_POINT('Ctrl Pts',(1.5129078685785E-11,-109.993984254242,
8.40164026751963));
#33223=CARTESIAN_POINT('Ctrl Pts',(4.85068927010198,-109.818984254242,8.4016402675109));
#33224=CARTESIAN_POINT('Ctrl Pts',(7.27603390513785,-109.643984254242,4.20082013374672));
#33225=CARTESIAN_POINT('Ctrl Pts',(9.70137854017372,-109.468984254242,-1.74689612655491E-11));
#33226=CARTESIAN_POINT('Ctrl Pts',(7.27603390512273,-109.293984254242,-4.20082013377291));
#33227=CARTESIAN_POINT('Ctrl Pts',(4.85068927007173,-109.118984254242,-8.40164026752836));
#33228=CARTESIAN_POINT('Ctrl Pts',(-1.51301075899711E-11,-108.943984254242,
-8.40164026751963));
#33229=CARTESIAN_POINT('Ctrl Pts',(-4.85068927010199,-108.768984254242,
-8.4016402675109));
#33230=CARTESIAN_POINT('Ctrl Pts',(-7.27603390513785,-108.593984254242,
-4.20082013374671));
#33231=CARTESIAN_POINT('Ctrl Pts',(-9.70137854017372,-108.418984254242,
1.74701493417668E-11));
#33232=CARTESIAN_POINT('Ctrl Pts',(-7.27603390512272,-108.243984254242,
4.20082013377292));
#33233=CARTESIAN_POINT('Ctrl Pts',(-4.85068927007173,-108.068984254242,
8.40164026752836));
#33234=CARTESIAN_POINT('Ctrl Pts',(1.5129078685785E-11,-107.893984254242,
8.40164026751963));
#33235=CARTESIAN_POINT('Ctrl Pts',(4.85068927010198,-107.718984254242,8.4016402675109));
#33236=CARTESIAN_POINT('Ctrl Pts',(7.27603390513785,-107.543984254242,4.20082013374672));
#33237=CARTESIAN_POINT('Ctrl Pts',(9.70137854017372,-107.368984254242,-1.74689612655491E-11));
#33238=CARTESIAN_POINT('Ctrl Pts',(7.27603390512273,-107.193984254242,-4.20082013377291));
#33239=CARTESIAN_POINT('Ctrl Pts',(4.85068927007173,-107.018984254242,-8.40164026752836));
#33240=CARTESIAN_POINT('Ctrl Pts',(-1.51301075899711E-11,-106.843984254242,
-8.40164026751963));
#33241=CARTESIAN_POINT('Ctrl Pts',(-4.85068927010199,-106.668984254242,
-8.4016402675109));
#33242=CARTESIAN_POINT('Ctrl Pts',(-7.27603390513785,-106.493984254242,
-4.20082013374671));
#33243=CARTESIAN_POINT('Ctrl Pts',(-9.70137854017372,-106.318984254242,
1.74701493417668E-11));
#33244=CARTESIAN_POINT('Ctrl Pts',(-7.27603390512272,-106.143984254242,
4.20082013377292));
#33245=CARTESIAN_POINT('Ctrl Pts',(-4.85068927007173,-105.968984254242,
8.40164026752836));
#33246=CARTESIAN_POINT('Ctrl Pts',(1.5129078685785E-11,-105.793984254242,
8.40164026751963));
#33247=CARTESIAN_POINT('Ctrl Pts',(4.85068927010198,-105.618984254242,8.4016402675109));
#33248=CARTESIAN_POINT('Ctrl Pts',(7.27603390513785,-105.443984254242,4.20082013374672));
#33249=CARTESIAN_POINT('Ctrl Pts',(9.70137854017372,-105.268984254242,-1.74689612655491E-11));
#33250=CARTESIAN_POINT('Ctrl Pts',(7.27603390512273,-105.093984254242,-4.20082013377291));
#33251=CARTESIAN_POINT('Ctrl Pts',(4.85068927007173,-104.918984254242,-8.40164026752836));
#33252=CARTESIAN_POINT('Ctrl Pts',(-1.51301075899711E-11,-104.743984254242,
-8.40164026751963));
#33253=CARTESIAN_POINT('Ctrl Pts',(-4.85068927010199,-104.568984254242,
-8.4016402675109));
#33254=CARTESIAN_POINT('Ctrl Pts',(-7.27603390513785,-104.393984254242,
-4.20082013374671));
#33255=CARTESIAN_POINT('Ctrl Pts',(-9.70137854017372,-104.218984254242,
1.74701493417668E-11));
#33256=CARTESIAN_POINT('Ctrl Pts',(-7.27603390512272,-104.043984254242,
4.20082013377292));
#33257=CARTESIAN_POINT('Ctrl Pts',(-4.85068927007173,-103.868984254242,
8.40164026752836));
#33258=CARTESIAN_POINT('Ctrl Pts',(1.5129078685785E-11,-103.693984254242,
8.40164026751963));
#33259=CARTESIAN_POINT('Ctrl Pts',(4.85068927010198,-103.518984254242,8.4016402675109));
#33260=CARTESIAN_POINT('Ctrl Pts',(7.27603390513785,-103.343984254242,4.20082013374672));
#33261=CARTESIAN_POINT('Ctrl Pts',(9.70137854017372,-103.168984254242,-1.74689612655491E-11));
#33262=CARTESIAN_POINT('Ctrl Pts',(7.27603390512273,-102.993984254242,-4.20082013377291));
#33263=CARTESIAN_POINT('Ctrl Pts',(4.85068927007173,-102.818984254242,-8.40164026752836));
#33264=CARTESIAN_POINT('Ctrl Pts',(-1.51301075899711E-11,-102.643984254242,
-8.40164026751963));
#33265=CARTESIAN_POINT('Ctrl Pts',(-4.85068927010199,-102.468984254242,
-8.4016402675109));
#33266=CARTESIAN_POINT('Ctrl Pts',(-7.27603390513785,-102.293984254242,
-4.20082013374671));
#33267=CARTESIAN_POINT('Ctrl Pts',(-9.70137854017372,-102.118984254242,
1.74701493417668E-11));
#33268=CARTESIAN_POINT('Ctrl Pts',(-7.27603390512272,-101.943984254242,
4.20082013377292));
#33269=CARTESIAN_POINT('Ctrl Pts',(-4.85068927007173,-101.768984254242,
8.40164026752836));
#33270=CARTESIAN_POINT('Ctrl Pts',(1.5129078685785E-11,-101.593984254242,
8.40164026751963));
#33271=CARTESIAN_POINT('Ctrl Pts',(4.85068927010198,-101.418984254242,8.4016402675109));
#33272=CARTESIAN_POINT('Ctrl Pts',(7.27603390513785,-101.243984254242,4.20082013374672));
#33273=CARTESIAN_POINT('Ctrl Pts',(9.70137854017372,-101.068984254242,-1.74689612655491E-11));
#33274=CARTESIAN_POINT('Ctrl Pts',(7.27603390512273,-100.893984254242,-4.20082013377291));
#33275=CARTESIAN_POINT('Ctrl Pts',(4.85068927007173,-100.718984254242,-8.40164026752836));
#33276=CARTESIAN_POINT('Ctrl Pts',(-1.51301075899711E-11,-100.543984254242,
-8.40164026751963));
#33277=CARTESIAN_POINT('Ctrl Pts',(-4.85068927010199,-100.368984254242,
-8.4016402675109));
#33278=CARTESIAN_POINT('Ctrl Pts',(-7.27603390513785,-100.193984254242,
-4.20082013374671));
#33279=CARTESIAN_POINT('Ctrl Pts',(-9.70137854017372,-100.018984254242,
1.74701493417668E-11));
#33280=CARTESIAN_POINT('Ctrl Pts',(-7.27603390512272,-99.8439842542419,
4.20082013377292));
#33281=CARTESIAN_POINT('Ctrl Pts',(-4.85068927007173,-99.6689842542419,
8.40164026752836));
#33282=CARTESIAN_POINT('Ctrl Pts',(1.5129078685785E-11,-99.4939842542419,
8.40164026751963));
#33283=CARTESIAN_POINT('Ctrl Pts',(4.85068927010198,-99.3189842542419,8.4016402675109));
#33284=CARTESIAN_POINT('Ctrl Pts',(7.27603390513785,-99.1439842542419,4.20082013374672));
#33285=CARTESIAN_POINT('Ctrl Pts',(9.70137854017372,-98.9689842542419,-1.74689612655491E-11));
#33286=CARTESIAN_POINT('Ctrl Pts',(7.27603390512273,-98.7939842542419,-4.20082013377291));
#33287=CARTESIAN_POINT('Ctrl Pts',(4.85068927007173,-98.6189842542419,-8.40164026752836));
#33288=CARTESIAN_POINT('Ctrl Pts',(-1.51301075899711E-11,-98.4439842542419,
-8.40164026751963));
#33289=CARTESIAN_POINT('Ctrl Pts',(-4.85068927010199,-98.2689842542419,
-8.4016402675109));
#33290=CARTESIAN_POINT('Ctrl Pts',(-7.27603390513785,-98.0939842542419,
-4.20082013374671));
#33291=CARTESIAN_POINT('Ctrl Pts',(-9.70137854017372,-97.9189842542419,
1.74701493417668E-11));
#33292=CARTESIAN_POINT('Ctrl Pts',(-7.27603390512272,-97.7439842542419,
4.20082013377292));
#33293=CARTESIAN_POINT('Ctrl Pts',(-4.85068927007173,-97.5689842542419,
8.40164026752836));
#33294=CARTESIAN_POINT('Ctrl Pts',(1.5129078685785E-11,-97.3939842542419,
8.40164026751963));
#33295=CARTESIAN_POINT('Ctrl Pts',(4.85068927010198,-97.2189842542419,8.4016402675109));
#33296=CARTESIAN_POINT('Ctrl Pts',(7.27603390513785,-97.0439842542419,4.20082013374672));
#33297=CARTESIAN_POINT('Ctrl Pts',(9.70137854017372,-96.8689842542419,-1.74689612655491E-11));
#33298=CARTESIAN_POINT('Ctrl Pts',(7.27603390512273,-96.6939842542419,-4.20082013377291));
#33299=CARTESIAN_POINT('Ctrl Pts',(4.85068927007173,-96.5189842542419,-8.40164026752836));
#33300=CARTESIAN_POINT('Ctrl Pts',(-1.51301075899711E-11,-96.3439842542419,
-8.40164026751963));
#33301=CARTESIAN_POINT('Ctrl Pts',(-4.85068927010199,-96.1689842542419,
-8.4016402675109));
#33302=CARTESIAN_POINT('Ctrl Pts',(-7.27603390513785,-95.9939842542419,
-4.20082013374671));
#33303=CARTESIAN_POINT('Ctrl Pts',(-9.70137854017372,-95.8189842542419,
1.74701493417668E-11));
#33304=CARTESIAN_POINT('Ctrl Pts',(-7.27603390512272,-95.6439842542419,
4.20082013377292));
#33305=CARTESIAN_POINT('Ctrl Pts',(-4.85068927007173,-95.4689842542419,
8.40164026752836));
#33306=CARTESIAN_POINT('Ctrl Pts',(1.5129078685785E-11,-95.2939842542419,
8.40164026751963));
#33307=CARTESIAN_POINT('Ctrl Pts',(4.85068927010198,-95.1189842542419,8.4016402675109));
#33308=CARTESIAN_POINT('Ctrl Pts',(7.27603390513785,-94.9439842542419,4.20082013374672));
#33309=CARTESIAN_POINT('Ctrl Pts',(9.70137854017372,-94.7689842542419,-1.74689612655491E-11));
#33310=CARTESIAN_POINT('Ctrl Pts',(7.27603390512273,-94.5939842542419,-4.20082013377291));
#33311=CARTESIAN_POINT('Ctrl Pts',(4.85068927007173,-94.4189842542419,-8.40164026752836));
#33312=CARTESIAN_POINT('Ctrl Pts',(-1.51301075899711E-11,-94.2439842542419,
-8.40164026751963));
#33313=CARTESIAN_POINT('Ctrl Pts',(-4.85068927010199,-94.0689842542419,
-8.4016402675109));
#33314=CARTESIAN_POINT('Ctrl Pts',(-7.27603390513785,-93.8939842542419,
-4.20082013374671));
#33315=CARTESIAN_POINT('Ctrl Pts',(-9.70137854017372,-93.7189842542419,
1.74701493417668E-11));
#33316=CARTESIAN_POINT('Ctrl Pts',(-7.27603390512272,-93.5439842542419,
4.20082013377292));
#33317=CARTESIAN_POINT('Ctrl Pts',(-4.85068927007173,-93.3689842542419,
8.40164026752836));
#33318=CARTESIAN_POINT('Ctrl Pts',(1.5129078685785E-11,-93.1939842542419,
8.40164026751963));
#33319=CARTESIAN_POINT('Ctrl Pts',(4.85068927010198,-93.0189842542419,8.4016402675109));
#33320=CARTESIAN_POINT('Ctrl Pts',(7.27603390513785,-92.8439842542419,4.20082013374672));
#33321=CARTESIAN_POINT('Ctrl Pts',(9.70137854017372,-92.6689842542419,-1.74689612655491E-11));
#33322=CARTESIAN_POINT('Ctrl Pts',(7.27603390512273,-92.4939842542419,-4.20082013377291));
#33323=CARTESIAN_POINT('Ctrl Pts',(4.85068927007173,-92.3189842542419,-8.40164026752836));
#33324=CARTESIAN_POINT('Ctrl Pts',(-1.51301075899711E-11,-92.1439842542419,
-8.40164026751963));
#33325=CARTESIAN_POINT('Ctrl Pts',(-4.85068927010199,-91.9689842542419,
-8.4016402675109));
#33326=CARTESIAN_POINT('Ctrl Pts',(-7.27603390513785,-91.7939842542419,
-4.20082013374671));
#33327=CARTESIAN_POINT('Ctrl Pts',(-9.70137854017372,-91.6189842542419,
1.74701493417668E-11));
#33328=CARTESIAN_POINT('Ctrl Pts',(-7.27603390512272,-91.4439842542419,
4.20082013377292));
#33329=CARTESIAN_POINT('Ctrl Pts',(-4.85068927007173,-91.2689842542419,
8.40164026752836));
#33330=CARTESIAN_POINT('Ctrl Pts',(1.5129078685785E-11,-91.0939842542419,
8.40164026751963));
#33331=CARTESIAN_POINT('Ctrl Pts',(4.85068927010198,-90.9189842542419,8.4016402675109));
#33332=CARTESIAN_POINT('Ctrl Pts',(7.27603390513785,-90.7439842542419,4.20082013374672));
#33333=CARTESIAN_POINT('Ctrl Pts',(9.70137854017372,-90.5689842542419,-1.74689612655491E-11));
#33334=CARTESIAN_POINT('Ctrl Pts',(7.27603390512273,-90.3939842542419,-4.20082013377291));
#33335=CARTESIAN_POINT('Ctrl Pts',(4.85068927007173,-90.2189842542419,-8.40164026752836));
#33336=CARTESIAN_POINT('Ctrl Pts',(-1.51301075899711E-11,-90.0439842542419,
-8.40164026751963));
#33337=CARTESIAN_POINT('Ctrl Pts',(-4.85068927010199,-89.8689842542419,
-8.4016402675109));
#33338=CARTESIAN_POINT('Ctrl Pts',(-7.27603390513785,-89.6939842542419,
-4.20082013374671));
#33339=CARTESIAN_POINT('Ctrl Pts',(-9.70137854017372,-89.5189842542419,
1.74701493417668E-11));
#33340=CARTESIAN_POINT('Ctrl Pts',(-7.27603390512272,-89.3439842542419,
4.20082013377292));
#33341=CARTESIAN_POINT('Ctrl Pts',(-4.85068927007173,-89.1689842542419,
8.40164026752836));
#33342=CARTESIAN_POINT('Ctrl Pts',(1.5129078685785E-11,-88.9939842542419,
8.40164026751963));
#33343=CARTESIAN_POINT('Ctrl Pts',(4.85068927010198,-88.8189842542419,8.4016402675109));
#33344=CARTESIAN_POINT('Ctrl Pts',(7.27603390513785,-88.6439842542419,4.20082013374672));
#33345=CARTESIAN_POINT('Ctrl Pts',(9.70137854017372,-88.4689842542419,-1.74689612655491E-11));
#33346=CARTESIAN_POINT('Ctrl Pts',(7.27603390512273,-88.2939842542419,-4.20082013377291));
#33347=CARTESIAN_POINT('Ctrl Pts',(4.85068927007173,-88.1189842542419,-8.40164026752836));
#33348=CARTESIAN_POINT('Ctrl Pts',(-1.51301075899711E-11,-87.9439842542419,
-8.40164026751963));
#33349=CARTESIAN_POINT('Ctrl Pts',(-4.85068927010199,-87.7689842542419,
-8.4016402675109));
#33350=CARTESIAN_POINT('Ctrl Pts',(-7.27603390513785,-87.5939842542419,
-4.20082013374671));
#33351=CARTESIAN_POINT('Ctrl Pts',(-9.70137854017372,-87.4189842542419,
1.74701493417668E-11));
#33352=CARTESIAN_POINT('Ctrl Pts',(-7.27603390512272,-87.2439842542419,
4.20082013377292));
#33353=CARTESIAN_POINT('Ctrl Pts',(-4.85068927007173,-87.0689842542419,
8.40164026752836));
#33354=CARTESIAN_POINT('Ctrl Pts',(1.5129078685785E-11,-86.8939842542419,
8.40164026751963));
#33355=CARTESIAN_POINT('Ctrl Pts',(4.85068927010198,-86.7189842542419,8.4016402675109));
#33356=CARTESIAN_POINT('Ctrl Pts',(7.27603390513785,-86.5439842542419,4.20082013374672));
#33357=CARTESIAN_POINT('Ctrl Pts',(9.70137854017372,-86.3689842542419,-1.74689612655491E-11));
#33358=CARTESIAN_POINT('Ctrl Pts',(7.27603390512273,-86.1939842542419,-4.20082013377291));
#33359=CARTESIAN_POINT('Ctrl Pts',(4.85068927007173,-86.0189842542419,-8.40164026752836));
#33360=CARTESIAN_POINT('Ctrl Pts',(-1.51301075899711E-11,-85.8439842542419,
-8.40164026751963));
#33361=CARTESIAN_POINT('Ctrl Pts',(-4.85068927010199,-85.6689842542419,
-8.4016402675109));
#33362=CARTESIAN_POINT('Ctrl Pts',(-7.27603390513785,-85.4939842542419,
-4.20082013374671));
#33363=CARTESIAN_POINT('Ctrl Pts',(-9.70137854017372,-85.3189842542419,
1.74701493417668E-11));
#33364=CARTESIAN_POINT('Ctrl Pts',(-7.27603390512272,-85.143984254242,4.20082013377292));
#33365=CARTESIAN_POINT('Ctrl Pts',(-4.85068927007173,-84.9689842542419,
8.40164026752836));
#33366=CARTESIAN_POINT('Ctrl Pts',(1.5129078685785E-11,-84.7939842542419,
8.40164026751963));
#33367=CARTESIAN_POINT('Ctrl Pts',(4.85068927010198,-84.6189842542419,8.4016402675109));
#33368=CARTESIAN_POINT('Ctrl Pts',(7.27603390513785,-84.443984254242,4.20082013374672));
#33369=CARTESIAN_POINT('Ctrl Pts',(9.70137854017372,-84.2689842542419,-1.74689612655491E-11));
#33370=CARTESIAN_POINT('Ctrl Pts',(7.27603390512273,-84.0939842542419,-4.20082013377291));
#33371=CARTESIAN_POINT('Ctrl Pts',(4.85068927007173,-83.9189842542419,-8.40164026752836));
#33372=CARTESIAN_POINT('Ctrl Pts',(-1.51301075899711E-11,-83.7439842542419,
-8.40164026751963));
#33373=CARTESIAN_POINT('Ctrl Pts',(-4.85068927010199,-83.5689842542419,
-8.4016402675109));
#33374=CARTESIAN_POINT('Ctrl Pts',(-7.27603390513785,-83.3939842542419,
-4.20082013374671));
#33375=CARTESIAN_POINT('Ctrl Pts',(-9.70137854017372,-83.2189842542419,
1.74701493417668E-11));
#33376=CARTESIAN_POINT('Ctrl Pts',(-7.27603390512272,-83.0439842542419,
4.20082013377292));
#33377=CARTESIAN_POINT('Ctrl Pts',(-4.85068927007173,-82.868984254242,8.40164026752836));
#33378=CARTESIAN_POINT('Ctrl Pts',(1.5129078685785E-11,-82.6939842542419,
8.40164026751963));
#33379=CARTESIAN_POINT('Ctrl Pts',(4.85068927010198,-82.5189842542419,8.4016402675109));
#33380=CARTESIAN_POINT('Ctrl Pts',(7.27603390513785,-82.3439842542419,4.20082013374672));
#33381=CARTESIAN_POINT('Ctrl Pts',(9.70137854017372,-82.1689842542419,-1.74689612655491E-11));
#33382=CARTESIAN_POINT('Ctrl Pts',(7.27603390512273,-81.993984254242,-4.20082013377291));
#33383=CARTESIAN_POINT('Ctrl Pts',(4.85068927007173,-81.8189842542419,-8.40164026752836));
#33384=CARTESIAN_POINT('Ctrl Pts',(-1.51301075899711E-11,-81.6439842542419,
-8.40164026751963));
#33385=CARTESIAN_POINT('Ctrl Pts',(-4.85068927010199,-81.4689842542419,
-8.4016402675109));
#33386=CARTESIAN_POINT('Ctrl Pts',(-7.27603390513785,-81.293984254242,-4.20082013374671));
#33387=CARTESIAN_POINT('Ctrl Pts',(-9.70137854017372,-81.1189842542419,
1.74701493417668E-11));
#33388=CARTESIAN_POINT('Ctrl Pts',(-7.27603390512272,-80.9439842542419,
4.20082013377292));
#33389=CARTESIAN_POINT('Ctrl Pts',(-4.85068927007173,-80.768984254242,8.40164026752836));
#33390=CARTESIAN_POINT('Ctrl Pts',(1.5129078685785E-11,-80.5939842542419,
8.40164026751963));
#33391=CARTESIAN_POINT('Ctrl Pts',(4.85068927010198,-80.4189842542419,8.4016402675109));
#33392=CARTESIAN_POINT('Ctrl Pts',(7.27603390513785,-80.243984254242,4.20082013374672));
#33393=CARTESIAN_POINT('Ctrl Pts',(9.70137854017372,-80.068984254242,-1.74689612655491E-11));
#33394=CARTESIAN_POINT('Ctrl Pts',(7.27603390512273,-79.8939842542419,-4.20082013377291));
#33395=CARTESIAN_POINT('Ctrl Pts',(4.85068927007173,-79.7189842542419,-8.40164026752836));
#33396=CARTESIAN_POINT('Ctrl Pts',(-1.51301075899711E-11,-79.5439842542419,
-8.40164026751963));
#33397=CARTESIAN_POINT('Ctrl Pts',(-4.85068927010199,-79.368984254242,-8.4016402675109));
#33398=CARTESIAN_POINT('Ctrl Pts',(-7.27603390513785,-79.193984254242,-4.20082013374671));
#33399=CARTESIAN_POINT('Ctrl Pts',(-9.70137854017372,-79.0189842542419,
1.74701493417668E-11));
#33400=CARTESIAN_POINT('Ctrl Pts',(-7.27603390512272,-78.8439842542419,
4.20082013377292));
#33401=CARTESIAN_POINT('Ctrl Pts',(-4.85068927007173,-78.668984254242,8.40164026752836));
#33402=CARTESIAN_POINT('Ctrl Pts',(1.5129078685785E-11,-78.493984254242,
8.40164026751963));
#33403=CARTESIAN_POINT('Ctrl Pts',(4.85068927010198,-78.3189842542419,8.4016402675109));
#33404=CARTESIAN_POINT('Ctrl Pts',(7.27603390513785,-78.143984254242,4.20082013374672));
#33405=CARTESIAN_POINT('Ctrl Pts',(9.70137854017372,-77.968984254242,-1.74689612655491E-11));
#33406=CARTESIAN_POINT('Ctrl Pts',(7.27603390512273,-77.7939842542419,-4.20082013377291));
#33407=CARTESIAN_POINT('Ctrl Pts',(4.85068927007173,-77.618984254242,-8.40164026752836));
#33408=CARTESIAN_POINT('Ctrl Pts',(-1.51301075899711E-11,-77.443984254242,
-8.40164026751963));
#33409=CARTESIAN_POINT('Ctrl Pts',(-4.85068927010199,-77.268984254242,-8.4016402675109));
#33410=CARTESIAN_POINT('Ctrl Pts',(-7.27603390513785,-77.0939842542419,
-4.20082013374671));
#33411=CARTESIAN_POINT('Ctrl Pts',(-9.70137854017372,-76.918984254242,1.74701493417668E-11));
#33412=CARTESIAN_POINT('Ctrl Pts',(-7.27603390512272,-76.743984254242,4.20082013377292));
#33413=CARTESIAN_POINT('Ctrl Pts',(-4.85068927007173,-76.5689842542419,
8.40164026752836));
#33414=CARTESIAN_POINT('Ctrl Pts',(1.5129078685785E-11,-76.393984254242,
8.40164026751963));
#33415=CARTESIAN_POINT('Ctrl Pts',(4.85068927010198,-76.218984254242,8.4016402675109));
#33416=CARTESIAN_POINT('Ctrl Pts',(7.27603390513785,-76.0439842542419,4.20082013374672));
#33417=CARTESIAN_POINT('Ctrl Pts',(9.70137854017372,-75.868984254242,-1.74689612655491E-11));
#33418=CARTESIAN_POINT('Ctrl Pts',(7.27603390512273,-75.693984254242,-4.20082013377291));
#33419=CARTESIAN_POINT('Ctrl Pts',(4.85068927007173,-75.518984254242,-8.40164026752836));
#33420=CARTESIAN_POINT('Ctrl Pts',(-1.51301075899711E-11,-75.343984254242,
-8.40164026751963));
#33421=CARTESIAN_POINT('Ctrl Pts',(-4.85068927010199,-75.1689842542419,
-8.4016402675109));
#33422=CARTESIAN_POINT('Ctrl Pts',(-7.27603390513785,-74.993984254242,-4.20082013374671));
#33423=CARTESIAN_POINT('Ctrl Pts',(-9.70137854017372,-74.818984254242,1.74701493417668E-11));
#33424=CARTESIAN_POINT('Ctrl Pts',(-7.27603390512272,-74.643984254242,4.20082013377292));
#33425=CARTESIAN_POINT('Ctrl Pts',(-4.85068927007173,-74.4689842542419,
8.40164026752836));
#33426=CARTESIAN_POINT('Ctrl Pts',(1.5129078685785E-11,-74.293984254242,
8.40164026751963));
#33427=CARTESIAN_POINT('Ctrl Pts',(4.85068927010198,-74.118984254242,8.4016402675109));
#33428=CARTESIAN_POINT('Ctrl Pts',(7.27603390513785,-73.943984254242,4.20082013374672));
#33429=CARTESIAN_POINT('Ctrl Pts',(9.70137854017372,-73.768984254242,-1.74689612655491E-11));
#33430=CARTESIAN_POINT('Ctrl Pts',(7.27603390512273,-73.593984254242,-4.20082013377291));
#33431=CARTESIAN_POINT('Ctrl Pts',(4.85068927007173,-73.4189842542419,-8.40164026752836));
#33432=CARTESIAN_POINT('Ctrl Pts',(-1.51301075899711E-11,-73.243984254242,
-8.40164026751963));
#33433=CARTESIAN_POINT('Ctrl Pts',(-4.85068927010199,-73.068984254242,-8.4016402675109));
#33434=CARTESIAN_POINT('Ctrl Pts',(-7.27603390513785,-72.893984254242,-4.20082013374671));
#33435=CARTESIAN_POINT('Ctrl Pts',(-9.70137854017372,-72.718984254242,1.74701493417668E-11));
#33436=CARTESIAN_POINT('Ctrl Pts',(-7.27603390512272,-72.543984254242,4.20082013377292));
#33437=CARTESIAN_POINT('Ctrl Pts',(-4.85068927007173,-72.368984254242,8.40164026752836));
#33438=CARTESIAN_POINT('Ctrl Pts',(1.5129078685785E-11,-72.193984254242,
8.40164026751963));
#33439=CARTESIAN_POINT('Ctrl Pts',(4.85068927010198,-72.018984254242,8.4016402675109));
#33440=CARTESIAN_POINT('Ctrl Pts',(7.27603390513785,-71.843984254242,4.20082013374672));
#33441=CARTESIAN_POINT('Ctrl Pts',(9.70137854017372,-71.6689842542419,-1.74689612655491E-11));
#33442=CARTESIAN_POINT('Ctrl Pts',(7.27603390512273,-71.493984254242,-4.20082013377291));
#33443=CARTESIAN_POINT('Ctrl Pts',(4.85068927007173,-71.318984254242,-8.40164026752836));
#33444=CARTESIAN_POINT('Ctrl Pts',(-1.51301075899711E-11,-71.143984254242,
-8.40164026751963));
#33445=CARTESIAN_POINT('Ctrl Pts',(-4.85068927010199,-70.968984254242,-8.4016402675109));
#33446=CARTESIAN_POINT('Ctrl Pts',(-7.27603390513785,-70.793984254242,-4.20082013374671));
#33447=CARTESIAN_POINT('Ctrl Pts',(-9.70137854017372,-70.618984254242,1.74701493417668E-11));
#33448=CARTESIAN_POINT('Ctrl Pts',(-7.27603390512272,-70.443984254242,4.20082013377292));
#33449=CARTESIAN_POINT('Ctrl Pts',(-4.85068927007173,-70.268984254242,8.40164026752836));
#33450=CARTESIAN_POINT('Ctrl Pts',(1.5129078685785E-11,-70.093984254242,
8.40164026751963));
#33451=CARTESIAN_POINT('Ctrl Pts',(4.85068927010198,-69.918984254242,8.4016402675109));
#33452=CARTESIAN_POINT('Ctrl Pts',(7.27603390513785,-69.743984254242,4.20082013374672));
#33453=CARTESIAN_POINT('Ctrl Pts',(9.70137854017372,-69.568984254242,-1.74689612655491E-11));
#33454=CARTESIAN_POINT('Ctrl Pts',(7.27603390512273,-69.393984254242,-4.20082013377291));
#33455=CARTESIAN_POINT('Ctrl Pts',(4.85068927007173,-69.218984254242,-8.40164026752836));
#33456=CARTESIAN_POINT('Ctrl Pts',(-1.51301075899711E-11,-69.043984254242,
-8.40164026751963));
#33457=CARTESIAN_POINT('Ctrl Pts',(-4.85068927010199,-68.868984254242,-8.4016402675109));
#33458=CARTESIAN_POINT('Ctrl Pts',(-7.27603390513785,-68.693984254242,-4.20082013374671));
#33459=CARTESIAN_POINT('Ctrl Pts',(-9.70137854017372,-68.518984254242,1.74701493417668E-11));
#33460=CARTESIAN_POINT('Ctrl Pts',(-7.27603390512272,-68.343984254242,4.20082013377292));
#33461=CARTESIAN_POINT('Ctrl Pts',(-4.85068927007173,-68.168984254242,8.40164026752836));
#33462=CARTESIAN_POINT('Ctrl Pts',(1.5129078685785E-11,-67.993984254242,
8.40164026751963));
#33463=CARTESIAN_POINT('Ctrl Pts',(4.85068927010198,-67.818984254242,8.4016402675109));
#33464=CARTESIAN_POINT('Ctrl Pts',(7.27603390513785,-67.643984254242,4.20082013374672));
#33465=CARTESIAN_POINT('Ctrl Pts',(9.70137854017372,-67.468984254242,-1.74689612655491E-11));
#33466=CARTESIAN_POINT('Ctrl Pts',(7.27603390512273,-67.293984254242,-4.20082013377291));
#33467=CARTESIAN_POINT('Ctrl Pts',(4.85068927007173,-67.118984254242,-8.40164026752836));
#33468=CARTESIAN_POINT('Ctrl Pts',(-1.51301075899711E-11,-66.943984254242,
-8.40164026751963));
#33469=CARTESIAN_POINT('Ctrl Pts',(-4.85068927010199,-66.768984254242,-8.4016402675109));
#33470=CARTESIAN_POINT('Ctrl Pts',(-7.27603390513785,-66.593984254242,-4.20082013374671));
#33471=CARTESIAN_POINT('Ctrl Pts',(-9.70137854017372,-66.418984254242,1.74701493417668E-11));
#33472=CARTESIAN_POINT('Ctrl Pts',(-7.27603390512272,-66.243984254242,4.20082013377292));
#33473=CARTESIAN_POINT('Ctrl Pts',(-4.85068927007173,-66.068984254242,8.40164026752836));
#33474=CARTESIAN_POINT('Ctrl Pts',(1.5129078685785E-11,-65.893984254242,
8.40164026751963));
#33475=CARTESIAN_POINT('Ctrl Pts',(4.85068927010198,-65.718984254242,8.4016402675109));
#33476=CARTESIAN_POINT('Ctrl Pts',(7.27603390513785,-65.543984254242,4.20082013374672));
#33477=CARTESIAN_POINT('Ctrl Pts',(9.70137854017372,-65.368984254242,-1.74689612655491E-11));
#33478=CARTESIAN_POINT('Ctrl Pts',(7.27603390512273,-65.193984254242,-4.20082013377291));
#33479=CARTESIAN_POINT('Ctrl Pts',(4.85068927007173,-65.018984254242,-8.40164026752836));
#33480=CARTESIAN_POINT('Ctrl Pts',(-1.51301075899711E-11,-64.843984254242,
-8.40164026751963));
#33481=CARTESIAN_POINT('Ctrl Pts',(-4.85068927010199,-64.668984254242,-8.4016402675109));
#33482=CARTESIAN_POINT('Ctrl Pts',(-7.27603390513785,-64.493984254242,-4.20082013374671));
#33483=CARTESIAN_POINT('Ctrl Pts',(-9.70137854017372,-64.318984254242,1.74701493417668E-11));
#33484=CARTESIAN_POINT('Ctrl Pts',(-7.27603390512272,-64.143984254242,4.20082013377292));
#33485=CARTESIAN_POINT('Ctrl Pts',(-4.85068927007173,-63.968984254242,8.40164026752836));
#33486=CARTESIAN_POINT('Ctrl Pts',(1.5129078685785E-11,-63.793984254242,
8.40164026751963));
#33487=CARTESIAN_POINT('Ctrl Pts',(4.85068927010198,-63.618984254242,8.4016402675109));
#33488=CARTESIAN_POINT('Ctrl Pts',(7.27603390513785,-63.443984254242,4.20082013374672));
#33489=CARTESIAN_POINT('Ctrl Pts',(9.70137854017372,-63.268984254242,-1.74689612655491E-11));
#33490=CARTESIAN_POINT('Ctrl Pts',(7.27603390512273,-63.093984254242,-4.20082013377291));
#33491=CARTESIAN_POINT('Ctrl Pts',(4.85068927007173,-62.918984254242,-8.40164026752836));
#33492=CARTESIAN_POINT('Ctrl Pts',(-1.51301075899711E-11,-62.743984254242,
-8.40164026751963));
#33493=CARTESIAN_POINT('Ctrl Pts',(-4.85068927010199,-62.568984254242,-8.4016402675109));
#33494=CARTESIAN_POINT('Ctrl Pts',(-7.27603390513785,-62.393984254242,-4.20082013374671));
#33495=CARTESIAN_POINT('Ctrl Pts',(-9.70137854017372,-62.218984254242,1.74701493417668E-11));
#33496=CARTESIAN_POINT('Ctrl Pts',(-7.27603390512272,-62.043984254242,4.20082013377292));
#33497=CARTESIAN_POINT('Ctrl Pts',(-4.85068927007173,-61.868984254242,8.40164026752836));
#33498=CARTESIAN_POINT('Ctrl Pts',(1.5129078685785E-11,-61.693984254242,
8.40164026751963));
#33499=CARTESIAN_POINT('Ctrl Pts',(4.85068927010198,-61.518984254242,8.4016402675109));
#33500=CARTESIAN_POINT('Ctrl Pts',(7.27603390513785,-61.343984254242,4.20082013374672));
#33501=CARTESIAN_POINT('Ctrl Pts',(9.70137854017372,-61.168984254242,-1.74689612655491E-11));
#33502=CARTESIAN_POINT('Ctrl Pts',(7.27603390512273,-60.993984254242,-4.20082013377291));
#33503=CARTESIAN_POINT('Ctrl Pts',(4.85068927007173,-60.818984254242,-8.40164026752836));
#33504=CARTESIAN_POINT('Ctrl Pts',(-1.51301075899711E-11,-60.643984254242,
-8.40164026751963));
#33505=CARTESIAN_POINT('Ctrl Pts',(-4.85068927010199,-60.468984254242,-8.4016402675109));
#33506=CARTESIAN_POINT('Ctrl Pts',(-7.27603390513785,-60.293984254242,-4.20082013374671));
#33507=CARTESIAN_POINT('Ctrl Pts',(-9.70137854017372,-60.118984254242,1.74701493417668E-11));
#33508=CARTESIAN_POINT('Ctrl Pts',(-7.27603390512272,-59.943984254242,4.20082013377292));
#33509=CARTESIAN_POINT('Ctrl Pts',(-4.85068927007173,-59.768984254242,8.40164026752836));
#33510=CARTESIAN_POINT('Ctrl Pts',(1.5129078685785E-11,-59.593984254242,
8.40164026751963));
#33511=CARTESIAN_POINT('Ctrl Pts',(4.85068927010198,-59.418984254242,8.4016402675109));
#33512=CARTESIAN_POINT('Ctrl Pts',(7.27603390513785,-59.243984254242,4.20082013374672));
#33513=CARTESIAN_POINT('Ctrl Pts',(9.70137854017372,-59.068984254242,-1.74689612655491E-11));
#33514=CARTESIAN_POINT('Ctrl Pts',(7.27603390512273,-58.893984254242,-4.20082013377291));
#33515=CARTESIAN_POINT('Ctrl Pts',(4.85068927007173,-58.718984254242,-8.40164026752836));
#33516=CARTESIAN_POINT('Ctrl Pts',(-1.51301075899711E-11,-58.543984254242,
-8.40164026751963));
#33517=CARTESIAN_POINT('Ctrl Pts',(-4.85068927010199,-58.368984254242,-8.4016402675109));
#33518=CARTESIAN_POINT('Ctrl Pts',(-7.27603390513785,-58.193984254242,-4.20082013374671));
#33519=CARTESIAN_POINT('Ctrl Pts',(-9.70137854017372,-58.018984254242,1.74701493417668E-11));
#33520=CARTESIAN_POINT('Ctrl Pts',(-7.27603390512272,-57.843984254242,4.20082013377292));
#33521=CARTESIAN_POINT('Ctrl Pts',(-4.85068927007173,-57.668984254242,8.40164026752836));
#33522=CARTESIAN_POINT('Ctrl Pts',(1.5129078685785E-11,-57.493984254242,
8.40164026751963));
#33523=CARTESIAN_POINT('Ctrl Pts',(4.85068927010198,-57.318984254242,8.4016402675109));
#33524=CARTESIAN_POINT('Ctrl Pts',(7.27603390513785,-57.143984254242,4.20082013374672));
#33525=CARTESIAN_POINT('Ctrl Pts',(9.70137854017372,-56.968984254242,-1.74689612655491E-11));
#33526=CARTESIAN_POINT('Ctrl Pts',(7.27603390512273,-56.793984254242,-4.20082013377291));
#33527=CARTESIAN_POINT('Ctrl Pts',(4.85068927007173,-56.618984254242,-8.40164026752836));
#33528=CARTESIAN_POINT('Ctrl Pts',(-1.51301075899711E-11,-56.443984254242,
-8.40164026751963));
#33529=CARTESIAN_POINT('Ctrl Pts',(-4.85068927010199,-56.268984254242,-8.4016402675109));
#33530=CARTESIAN_POINT('Ctrl Pts',(-7.27603390513785,-56.093984254242,-4.20082013374671));
#33531=CARTESIAN_POINT('Ctrl Pts',(-9.70137854017372,-55.918984254242,1.74701493417668E-11));
#33532=CARTESIAN_POINT('Ctrl Pts',(-7.27603390512272,-55.743984254242,4.20082013377292));
#33533=CARTESIAN_POINT('Ctrl Pts',(-4.85068927007173,-55.568984254242,8.40164026752836));
#33534=CARTESIAN_POINT('Ctrl Pts',(1.5129078685785E-11,-55.393984254242,
8.40164026751963));
#33535=CARTESIAN_POINT('Ctrl Pts',(4.85068927010198,-55.218984254242,8.4016402675109));
#33536=CARTESIAN_POINT('Ctrl Pts',(7.27603390513785,-55.043984254242,4.20082013374672));
#33537=CARTESIAN_POINT('Ctrl Pts',(9.70137854017372,-54.868984254242,-1.74689612655491E-11));
#33538=CARTESIAN_POINT('Ctrl Pts',(7.27603390512273,-54.693984254242,-4.20082013377291));
#33539=CARTESIAN_POINT('Ctrl Pts',(4.85068927007173,-54.518984254242,-8.40164026752836));
#33540=CARTESIAN_POINT('Ctrl Pts',(-1.51301075899711E-11,-54.343984254242,
-8.40164026751963));
#33541=CARTESIAN_POINT('Ctrl Pts',(-4.85068927010199,-54.168984254242,-8.4016402675109));
#33542=CARTESIAN_POINT('Ctrl Pts',(-7.27603390513785,-53.993984254242,-4.20082013374671));
#33543=CARTESIAN_POINT('Ctrl Pts',(-9.70137854017372,-53.818984254242,1.74701493417668E-11));
#33544=CARTESIAN_POINT('Ctrl Pts',(-7.27603390512272,-53.643984254242,4.20082013377292));
#33545=CARTESIAN_POINT('Ctrl Pts',(-4.85068927007173,-53.468984254242,8.40164026752836));
#33546=CARTESIAN_POINT('Ctrl Pts',(1.5129078685785E-11,-53.293984254242,
8.40164026751963));
#33547=CARTESIAN_POINT('Ctrl Pts',(4.85068927010198,-53.118984254242,8.4016402675109));
#33548=CARTESIAN_POINT('Ctrl Pts',(7.27603390513785,-52.943984254242,4.20082013374672));
#33549=CARTESIAN_POINT('Ctrl Pts',(9.70137854017372,-52.768984254242,-1.74689612655491E-11));
#33550=CARTESIAN_POINT('Ctrl Pts',(7.27603390512273,-52.593984254242,-4.20082013377291));
#33551=CARTESIAN_POINT('Ctrl Pts',(4.85068927007173,-52.418984254242,-8.40164026752836));
#33552=CARTESIAN_POINT('Ctrl Pts',(-1.51301075899711E-11,-52.243984254242,
-8.40164026751963));
#33553=CARTESIAN_POINT('Ctrl Pts',(-4.85068927010199,-52.068984254242,-8.4016402675109));
#33554=CARTESIAN_POINT('Ctrl Pts',(-7.27603390513785,-51.893984254242,-4.20082013374671));
#33555=CARTESIAN_POINT('Ctrl Pts',(-9.70137854017372,-51.718984254242,1.74701493417668E-11));
#33556=CARTESIAN_POINT('Ctrl Pts',(-7.27603390512272,-51.543984254242,4.20082013377292));
#33557=CARTESIAN_POINT('Ctrl Pts',(-4.85068927007173,-51.368984254242,8.40164026752836));
#33558=CARTESIAN_POINT('Ctrl Pts',(1.5129078685785E-11,-51.193984254242,
8.40164026751963));
#33559=CARTESIAN_POINT('Ctrl Pts',(4.85068927010198,-51.018984254242,8.4016402675109));
#33560=CARTESIAN_POINT('Ctrl Pts',(7.27603390513785,-50.843984254242,4.20082013374672));
#33561=CARTESIAN_POINT('Ctrl Pts',(9.70137854017372,-50.668984254242,-1.74689612655491E-11));
#33562=CARTESIAN_POINT('Ctrl Pts',(7.27603390512273,-50.493984254242,-4.20082013377291));
#33563=CARTESIAN_POINT('Ctrl Pts',(4.85068927007173,-50.318984254242,-8.40164026752836));
#33564=CARTESIAN_POINT('Ctrl Pts',(-1.51301075899711E-11,-50.143984254242,
-8.40164026751963));
#33565=CARTESIAN_POINT('Ctrl Pts',(-4.85068927010199,-49.968984254242,-8.4016402675109));
#33566=CARTESIAN_POINT('Ctrl Pts',(-7.27603390513785,-49.793984254242,-4.20082013374671));
#33567=CARTESIAN_POINT('Ctrl Pts',(-9.70137854017372,-49.618984254242,1.74701493417668E-11));
#33568=CARTESIAN_POINT('Ctrl Pts',(-7.27603390512272,-49.443984254242,4.20082013377292));
#33569=CARTESIAN_POINT('Ctrl Pts',(-4.85068927007173,-49.268984254242,8.40164026752836));
#33570=CARTESIAN_POINT('Ctrl Pts',(1.5129078685785E-11,-49.093984254242,
8.40164026751963));
#33571=CARTESIAN_POINT('Ctrl Pts',(4.85068927010198,-48.918984254242,8.4016402675109));
#33572=CARTESIAN_POINT('Ctrl Pts',(7.27603390513785,-48.743984254242,4.20082013374672));
#33573=CARTESIAN_POINT('Ctrl Pts',(9.70137854017372,-48.568984254242,-1.74689612655491E-11));
#33574=CARTESIAN_POINT('Ctrl Pts',(7.27603390512273,-48.393984254242,-4.20082013377291));
#33575=CARTESIAN_POINT('Ctrl Pts',(4.85068927007173,-48.218984254242,-8.40164026752836));
#33576=CARTESIAN_POINT('Ctrl Pts',(-1.51301075899711E-11,-48.043984254242,
-8.40164026751963));
#33577=CARTESIAN_POINT('Ctrl Pts',(-4.85068927010199,-47.868984254242,-8.4016402675109));
#33578=CARTESIAN_POINT('Ctrl Pts',(-7.27603390513785,-47.693984254242,-4.20082013374671));
#33579=CARTESIAN_POINT('Ctrl Pts',(-9.70137854017372,-47.518984254242,1.74701493417668E-11));
#33580=CARTESIAN_POINT('Ctrl Pts',(-7.27603390512272,-47.343984254242,4.20082013377292));
#33581=CARTESIAN_POINT('Ctrl Pts',(-4.85068927007173,-47.168984254242,8.40164026752836));
#33582=CARTESIAN_POINT('Ctrl Pts',(1.5129078685785E-11,-46.993984254242,
8.40164026751963));
#33583=CARTESIAN_POINT('Ctrl Pts',(4.85068927010198,-46.818984254242,8.4016402675109));
#33584=CARTESIAN_POINT('Ctrl Pts',(7.27603390513785,-46.643984254242,4.20082013374672));
#33585=CARTESIAN_POINT('Ctrl Pts',(9.70137854017372,-46.468984254242,-1.74689612655491E-11));
#33586=CARTESIAN_POINT('Ctrl Pts',(7.27603390512273,-46.293984254242,-4.20082013377291));
#33587=CARTESIAN_POINT('Ctrl Pts',(4.85068927007173,-46.118984254242,-8.40164026752836));
#33588=CARTESIAN_POINT('Ctrl Pts',(-1.51301075899711E-11,-45.943984254242,
-8.40164026751963));
#33589=CARTESIAN_POINT('Ctrl Pts',(-4.85068927010199,-45.768984254242,-8.4016402675109));
#33590=CARTESIAN_POINT('Ctrl Pts',(-7.27603390513785,-45.593984254242,-4.20082013374671));
#33591=CARTESIAN_POINT('Ctrl Pts',(-9.70137854017372,-45.418984254242,1.74701493417668E-11));
#33592=CARTESIAN_POINT('Ctrl Pts',(-7.27603390512272,-45.243984254242,4.20082013377292));
#33593=CARTESIAN_POINT('Ctrl Pts',(-4.85068927007173,-45.068984254242,8.40164026752836));
#33594=CARTESIAN_POINT('Ctrl Pts',(1.5129078685785E-11,-44.893984254242,
8.40164026751963));
#33595=CARTESIAN_POINT('Ctrl Pts',(4.85068927010198,-44.718984254242,8.4016402675109));
#33596=CARTESIAN_POINT('Ctrl Pts',(7.27603390513785,-44.543984254242,4.20082013374672));
#33597=CARTESIAN_POINT('Ctrl Pts',(9.70137854017372,-44.368984254242,-1.74689612655491E-11));
#33598=CARTESIAN_POINT('Ctrl Pts',(7.27603390512273,-44.193984254242,-4.20082013377291));
#33599=CARTESIAN_POINT('Ctrl Pts',(4.85068927007173,-44.018984254242,-8.40164026752836));
#33600=CARTESIAN_POINT('Ctrl Pts',(-1.51301075899711E-11,-43.843984254242,
-8.40164026751963));
#33601=CARTESIAN_POINT('Ctrl Pts',(-1.4702867290402E-11,-213.820483118095,
-8.16439679232146));
#33602=CARTESIAN_POINT('Ctrl Pts',(-4.71371668583241,-213.645483118095,
-8.16439679231297));
#33603=CARTESIAN_POINT('Ctrl Pts',(-7.07057502873392,-213.470483118095,
-4.082198396148));
#33604=CARTESIAN_POINT('Ctrl Pts',(-9.42743337163542,-213.295483118095,
1.69768315121407E-11));
#33605=CARTESIAN_POINT('Ctrl Pts',(-7.07057502871922,-213.120483118095,
4.08219839617346));
#33606=CARTESIAN_POINT('Ctrl Pts',(-4.71371668580301,-212.945483118095,
8.16439679232994));
#33607=CARTESIAN_POINT('Ctrl Pts',(1.47018674401621E-11,-212.770483118095,
8.16439679232146));
#33608=CARTESIAN_POINT('Ctrl Pts',(4.71371668583241,-212.595483118095,8.16439679231297));
#33609=CARTESIAN_POINT('Ctrl Pts',(7.07057502873392,-212.420483118095,4.082198396148));
#33610=CARTESIAN_POINT('Ctrl Pts',(9.42743337163542,-212.245483118095,-1.69756769845304E-11));
#33611=CARTESIAN_POINT('Ctrl Pts',(7.07057502871922,-212.070483118095,-4.08219839617346));
#33612=CARTESIAN_POINT('Ctrl Pts',(4.71371668580301,-211.895483118095,-8.16439679232994));
#33613=CARTESIAN_POINT('Ctrl Pts',(-1.4702867290402E-11,-211.720483118095,
-8.16439679232146));
#33614=CARTESIAN_POINT('Ctrl Pts',(-4.71371668583241,-211.545483118095,
-8.16439679231297));
#33615=CARTESIAN_POINT('Ctrl Pts',(-7.07057502873392,-211.370483118095,
-4.082198396148));
#33616=CARTESIAN_POINT('Ctrl Pts',(-9.42743337163542,-211.195483118095,
1.69768315121407E-11));
#33617=CARTESIAN_POINT('Ctrl Pts',(-7.07057502871922,-211.020483118095,
4.08219839617346));
#33618=CARTESIAN_POINT('Ctrl Pts',(-4.71371668580301,-210.845483118095,
8.16439679232994));
#33619=CARTESIAN_POINT('Ctrl Pts',(1.47018674401621E-11,-210.670483118095,
8.16439679232146));
#33620=CARTESIAN_POINT('Ctrl Pts',(4.71371668583241,-210.495483118095,8.16439679231297));
#33621=CARTESIAN_POINT('Ctrl Pts',(7.07057502873392,-210.320483118095,4.082198396148));
#33622=CARTESIAN_POINT('Ctrl Pts',(9.42743337163542,-210.145483118095,-1.69756769845304E-11));
#33623=CARTESIAN_POINT('Ctrl Pts',(7.07057502871922,-209.970483118095,-4.08219839617346));
#33624=CARTESIAN_POINT('Ctrl Pts',(4.71371668580301,-209.795483118095,-8.16439679232994));
#33625=CARTESIAN_POINT('Ctrl Pts',(-1.4702867290402E-11,-209.620483118095,
-8.16439679232146));
#33626=CARTESIAN_POINT('Ctrl Pts',(-4.71371668583241,-209.445483118095,
-8.16439679231297));
#33627=CARTESIAN_POINT('Ctrl Pts',(-7.07057502873392,-209.270483118095,
-4.082198396148));
#33628=CARTESIAN_POINT('Ctrl Pts',(-9.42743337163542,-209.095483118095,
1.69768315121407E-11));
#33629=CARTESIAN_POINT('Ctrl Pts',(-7.07057502871922,-208.920483118095,
4.08219839617346));
#33630=CARTESIAN_POINT('Ctrl Pts',(-4.71371668580301,-208.745483118095,
8.16439679232994));
#33631=CARTESIAN_POINT('Ctrl Pts',(1.47018674401621E-11,-208.570483118095,
8.16439679232146));
#33632=CARTESIAN_POINT('Ctrl Pts',(4.71371668583241,-208.395483118095,8.16439679231297));
#33633=CARTESIAN_POINT('Ctrl Pts',(7.07057502873392,-208.220483118095,4.082198396148));
#33634=CARTESIAN_POINT('Ctrl Pts',(9.42743337163542,-208.045483118095,-1.69756769845304E-11));
#33635=CARTESIAN_POINT('Ctrl Pts',(7.07057502871922,-207.870483118095,-4.08219839617346));
#33636=CARTESIAN_POINT('Ctrl Pts',(4.71371668580301,-207.695483118095,-8.16439679232994));
#33637=CARTESIAN_POINT('Ctrl Pts',(-1.4702867290402E-11,-207.520483118095,
-8.16439679232146));
#33638=CARTESIAN_POINT('Ctrl Pts',(-4.71371668583241,-207.345483118095,
-8.16439679231297));
#33639=CARTESIAN_POINT('Ctrl Pts',(-7.07057502873392,-207.170483118095,
-4.082198396148));
#33640=CARTESIAN_POINT('Ctrl Pts',(-9.42743337163542,-206.995483118095,
1.69768315121407E-11));
#33641=CARTESIAN_POINT('Ctrl Pts',(-7.07057502871922,-206.820483118095,
4.08219839617346));
#33642=CARTESIAN_POINT('Ctrl Pts',(-4.71371668580301,-206.645483118095,
8.16439679232994));
#33643=CARTESIAN_POINT('Ctrl Pts',(1.47018674401621E-11,-206.470483118095,
8.16439679232146));
#33644=CARTESIAN_POINT('Ctrl Pts',(4.71371668583241,-206.295483118095,8.16439679231297));
#33645=CARTESIAN_POINT('Ctrl Pts',(7.07057502873392,-206.120483118095,4.082198396148));
#33646=CARTESIAN_POINT('Ctrl Pts',(9.42743337163542,-205.945483118095,-1.69756769845304E-11));
#33647=CARTESIAN_POINT('Ctrl Pts',(7.07057502871922,-205.770483118095,-4.08219839617346));
#33648=CARTESIAN_POINT('Ctrl Pts',(4.71371668580301,-205.595483118095,-8.16439679232994));
#33649=CARTESIAN_POINT('Ctrl Pts',(-1.4702867290402E-11,-205.420483118095,
-8.16439679232146));
#33650=CARTESIAN_POINT('Ctrl Pts',(-4.71371668583241,-205.245483118095,
-8.16439679231297));
#33651=CARTESIAN_POINT('Ctrl Pts',(-7.07057502873392,-205.070483118095,
-4.082198396148));
#33652=CARTESIAN_POINT('Ctrl Pts',(-9.42743337163542,-204.895483118095,
1.69768315121407E-11));
#33653=CARTESIAN_POINT('Ctrl Pts',(-7.07057502871922,-204.720483118095,
4.08219839617346));
#33654=CARTESIAN_POINT('Ctrl Pts',(-4.71371668580301,-204.545483118095,
8.16439679232994));
#33655=CARTESIAN_POINT('Ctrl Pts',(1.47018674401621E-11,-204.370483118095,
8.16439679232146));
#33656=CARTESIAN_POINT('Ctrl Pts',(4.71371668583241,-204.195483118095,8.16439679231297));
#33657=CARTESIAN_POINT('Ctrl Pts',(7.07057502873392,-204.020483118095,4.082198396148));
#33658=CARTESIAN_POINT('Ctrl Pts',(9.42743337163542,-203.845483118095,-1.69756769845304E-11));
#33659=CARTESIAN_POINT('Ctrl Pts',(7.07057502871922,-203.670483118095,-4.08219839617346));
#33660=CARTESIAN_POINT('Ctrl Pts',(4.71371668580301,-203.495483118095,-8.16439679232994));
#33661=CARTESIAN_POINT('Ctrl Pts',(-1.4702867290402E-11,-203.320483118095,
-8.16439679232146));
#33662=CARTESIAN_POINT('Ctrl Pts',(-4.71371668583241,-203.145483118095,
-8.16439679231297));
#33663=CARTESIAN_POINT('Ctrl Pts',(-7.07057502873392,-202.970483118095,
-4.082198396148));
#33664=CARTESIAN_POINT('Ctrl Pts',(-9.42743337163542,-202.795483118095,
1.69768315121407E-11));
#33665=CARTESIAN_POINT('Ctrl Pts',(-7.07057502871922,-202.620483118095,
4.08219839617346));
#33666=CARTESIAN_POINT('Ctrl Pts',(-4.71371668580301,-202.445483118095,
8.16439679232994));
#33667=CARTESIAN_POINT('Ctrl Pts',(1.47018674401621E-11,-202.270483118095,
8.16439679232146));
#33668=CARTESIAN_POINT('Ctrl Pts',(4.71371668583241,-202.095483118095,8.16439679231297));
#33669=CARTESIAN_POINT('Ctrl Pts',(7.07057502873392,-201.920483118095,4.082198396148));
#33670=CARTESIAN_POINT('Ctrl Pts',(9.42743337163542,-201.745483118095,-1.69756769845304E-11));
#33671=CARTESIAN_POINT('Ctrl Pts',(7.07057502871922,-201.570483118095,-4.08219839617346));
#33672=CARTESIAN_POINT('Ctrl Pts',(4.71371668580301,-201.395483118095,-8.16439679232994));
#33673=CARTESIAN_POINT('Ctrl Pts',(-1.4702867290402E-11,-201.220483118095,
-8.16439679232146));
#33674=CARTESIAN_POINT('Ctrl Pts',(-4.71371668583241,-201.045483118095,
-8.16439679231297));
#33675=CARTESIAN_POINT('Ctrl Pts',(-7.07057502873392,-200.870483118095,
-4.082198396148));
#33676=CARTESIAN_POINT('Ctrl Pts',(-9.42743337163542,-200.695483118095,
1.69768315121407E-11));
#33677=CARTESIAN_POINT('Ctrl Pts',(-7.07057502871922,-200.520483118095,
4.08219839617346));
#33678=CARTESIAN_POINT('Ctrl Pts',(-4.71371668580301,-200.345483118095,
8.16439679232994));
#33679=CARTESIAN_POINT('Ctrl Pts',(1.47018674401621E-11,-200.170483118095,
8.16439679232146));
#33680=CARTESIAN_POINT('Ctrl Pts',(4.71371668583241,-199.995483118095,8.16439679231297));
#33681=CARTESIAN_POINT('Ctrl Pts',(7.07057502873392,-199.820483118095,4.082198396148));
#33682=CARTESIAN_POINT('Ctrl Pts',(9.42743337163542,-199.645483118095,-1.69756769845304E-11));
#33683=CARTESIAN_POINT('Ctrl Pts',(7.07057502871922,-199.470483118095,-4.08219839617346));
#33684=CARTESIAN_POINT('Ctrl Pts',(4.71371668580301,-199.295483118095,-8.16439679232994));
#33685=CARTESIAN_POINT('Ctrl Pts',(-1.4702867290402E-11,-199.120483118095,
-8.16439679232146));
#33686=CARTESIAN_POINT('Ctrl Pts',(-4.71371668583241,-198.945483118095,
-8.16439679231297));
#33687=CARTESIAN_POINT('Ctrl Pts',(-7.07057502873392,-198.770483118095,
-4.082198396148));
#33688=CARTESIAN_POINT('Ctrl Pts',(-9.42743337163542,-198.595483118095,
1.69768315121407E-11));
#33689=CARTESIAN_POINT('Ctrl Pts',(-7.07057502871922,-198.420483118095,
4.08219839617346));
#33690=CARTESIAN_POINT('Ctrl Pts',(-4.71371668580301,-198.245483118095,
8.16439679232994));
#33691=CARTESIAN_POINT('Ctrl Pts',(1.47018674401621E-11,-198.070483118095,
8.16439679232146));
#33692=CARTESIAN_POINT('Ctrl Pts',(4.71371668583241,-197.895483118095,8.16439679231297));
#33693=CARTESIAN_POINT('Ctrl Pts',(7.07057502873392,-197.720483118095,4.082198396148));
#33694=CARTESIAN_POINT('Ctrl Pts',(9.42743337163542,-197.545483118095,-1.69756769845304E-11));
#33695=CARTESIAN_POINT('Ctrl Pts',(7.07057502871922,-197.370483118095,-4.08219839617346));
#33696=CARTESIAN_POINT('Ctrl Pts',(4.71371668580301,-197.195483118095,-8.16439679232994));
#33697=CARTESIAN_POINT('Ctrl Pts',(-1.4702867290402E-11,-197.020483118095,
-8.16439679232146));
#33698=CARTESIAN_POINT('Ctrl Pts',(-4.71371668583241,-196.845483118095,
-8.16439679231297));
#33699=CARTESIAN_POINT('Ctrl Pts',(-7.07057502873392,-196.670483118095,
-4.082198396148));
#33700=CARTESIAN_POINT('Ctrl Pts',(-9.42743337163542,-196.495483118095,
1.69768315121407E-11));
#33701=CARTESIAN_POINT('Ctrl Pts',(-7.07057502871922,-196.320483118095,
4.08219839617346));
#33702=CARTESIAN_POINT('Ctrl Pts',(-4.71371668580301,-196.145483118095,
8.16439679232994));
#33703=CARTESIAN_POINT('Ctrl Pts',(1.47018674401621E-11,-195.970483118095,
8.16439679232146));
#33704=CARTESIAN_POINT('Ctrl Pts',(4.71371668583241,-195.795483118095,8.16439679231297));
#33705=CARTESIAN_POINT('Ctrl Pts',(7.07057502873392,-195.620483118095,4.082198396148));
#33706=CARTESIAN_POINT('Ctrl Pts',(9.42743337163542,-195.445483118095,-1.69756769845304E-11));
#33707=CARTESIAN_POINT('Ctrl Pts',(7.07057502871922,-195.270483118095,-4.08219839617346));
#33708=CARTESIAN_POINT('Ctrl Pts',(4.71371668580301,-195.095483118095,-8.16439679232994));
#33709=CARTESIAN_POINT('Ctrl Pts',(-1.4702867290402E-11,-194.920483118095,
-8.16439679232146));
#33710=CARTESIAN_POINT('Ctrl Pts',(-4.71371668583241,-194.745483118095,
-8.16439679231297));
#33711=CARTESIAN_POINT('Ctrl Pts',(-7.07057502873392,-194.570483118095,
-4.082198396148));
#33712=CARTESIAN_POINT('Ctrl Pts',(-9.42743337163542,-194.395483118095,
1.69768315121407E-11));
#33713=CARTESIAN_POINT('Ctrl Pts',(-7.07057502871922,-194.220483118095,
4.08219839617346));
#33714=CARTESIAN_POINT('Ctrl Pts',(-4.71371668580301,-194.045483118095,
8.16439679232994));
#33715=CARTESIAN_POINT('Ctrl Pts',(1.47018674401621E-11,-193.870483118095,
8.16439679232146));
#33716=CARTESIAN_POINT('Ctrl Pts',(4.71371668583241,-193.695483118095,8.16439679231297));
#33717=CARTESIAN_POINT('Ctrl Pts',(7.07057502873392,-193.520483118095,4.082198396148));
#33718=CARTESIAN_POINT('Ctrl Pts',(9.42743337163542,-193.345483118095,-1.69756769845304E-11));
#33719=CARTESIAN_POINT('Ctrl Pts',(7.07057502871922,-193.170483118095,-4.08219839617346));
#33720=CARTESIAN_POINT('Ctrl Pts',(4.71371668580301,-192.995483118095,-8.16439679232994));
#33721=CARTESIAN_POINT('Ctrl Pts',(-1.4702867290402E-11,-192.820483118095,
-8.16439679232146));
#33722=CARTESIAN_POINT('Ctrl Pts',(-4.71371668583241,-192.645483118095,
-8.16439679231297));
#33723=CARTESIAN_POINT('Ctrl Pts',(-7.07057502873392,-192.470483118095,
-4.082198396148));
#33724=CARTESIAN_POINT('Ctrl Pts',(-9.42743337163542,-192.295483118095,
1.69768315121407E-11));
#33725=CARTESIAN_POINT('Ctrl Pts',(-7.07057502871922,-192.120483118095,
4.08219839617346));
#33726=CARTESIAN_POINT('Ctrl Pts',(-4.71371668580301,-191.945483118095,
8.16439679232994));
#33727=CARTESIAN_POINT('Ctrl Pts',(1.47018674401621E-11,-191.770483118095,
8.16439679232146));
#33728=CARTESIAN_POINT('Ctrl Pts',(4.71371668583241,-191.595483118095,8.16439679231297));
#33729=CARTESIAN_POINT('Ctrl Pts',(7.07057502873392,-191.420483118095,4.082198396148));
#33730=CARTESIAN_POINT('Ctrl Pts',(9.42743337163542,-191.245483118095,-1.69756769845304E-11));
#33731=CARTESIAN_POINT('Ctrl Pts',(7.07057502871922,-191.070483118095,-4.08219839617346));
#33732=CARTESIAN_POINT('Ctrl Pts',(4.71371668580301,-190.895483118095,-8.16439679232994));
#33733=CARTESIAN_POINT('Ctrl Pts',(-1.4702867290402E-11,-190.720483118095,
-8.16439679232146));
#33734=CARTESIAN_POINT('Ctrl Pts',(-4.71371668583241,-190.545483118095,
-8.16439679231297));
#33735=CARTESIAN_POINT('Ctrl Pts',(-7.07057502873392,-190.370483118095,
-4.082198396148));
#33736=CARTESIAN_POINT('Ctrl Pts',(-9.42743337163542,-190.195483118095,
1.69768315121407E-11));
#33737=CARTESIAN_POINT('Ctrl Pts',(-7.07057502871922,-190.020483118095,
4.08219839617346));
#33738=CARTESIAN_POINT('Ctrl Pts',(-4.71371668580301,-189.845483118095,
8.16439679232994));
#33739=CARTESIAN_POINT('Ctrl Pts',(1.47018674401621E-11,-189.670483118095,
8.16439679232146));
#33740=CARTESIAN_POINT('Ctrl Pts',(4.71371668583241,-189.495483118095,8.16439679231297));
#33741=CARTESIAN_POINT('Ctrl Pts',(7.07057502873392,-189.320483118095,4.082198396148));
#33742=CARTESIAN_POINT('Ctrl Pts',(9.42743337163542,-189.145483118095,-1.69756769845304E-11));
#33743=CARTESIAN_POINT('Ctrl Pts',(7.07057502871922,-188.970483118095,-4.08219839617346));
#33744=CARTESIAN_POINT('Ctrl Pts',(4.71371668580301,-188.795483118095,-8.16439679232994));
#33745=CARTESIAN_POINT('Ctrl Pts',(-1.4702867290402E-11,-188.620483118095,
-8.16439679232146));
#33746=CARTESIAN_POINT('Ctrl Pts',(-4.71371668583241,-188.445483118095,
-8.16439679231297));
#33747=CARTESIAN_POINT('Ctrl Pts',(-7.07057502873392,-188.270483118095,
-4.082198396148));
#33748=CARTESIAN_POINT('Ctrl Pts',(-9.42743337163542,-188.095483118095,
1.69768315121407E-11));
#33749=CARTESIAN_POINT('Ctrl Pts',(-7.07057502871922,-187.920483118095,
4.08219839617346));
#33750=CARTESIAN_POINT('Ctrl Pts',(-4.71371668580301,-187.745483118095,
8.16439679232994));
#33751=CARTESIAN_POINT('Ctrl Pts',(1.47018674401621E-11,-187.570483118095,
8.16439679232146));
#33752=CARTESIAN_POINT('Ctrl Pts',(4.71371668583241,-187.395483118095,8.16439679231297));
#33753=CARTESIAN_POINT('Ctrl Pts',(7.07057502873392,-187.220483118095,4.082198396148));
#33754=CARTESIAN_POINT('Ctrl Pts',(9.42743337163542,-187.045483118095,-1.69756769845304E-11));
#33755=CARTESIAN_POINT('Ctrl Pts',(7.07057502871922,-186.870483118095,-4.08219839617346));
#33756=CARTESIAN_POINT('Ctrl Pts',(4.71371668580301,-186.695483118095,-8.16439679232994));
#33757=CARTESIAN_POINT('Ctrl Pts',(-1.4702867290402E-11,-186.520483118095,
-8.16439679232146));
#33758=CARTESIAN_POINT('Ctrl Pts',(-4.71371668583241,-186.345483118095,
-8.16439679231297));
#33759=CARTESIAN_POINT('Ctrl Pts',(-7.07057502873392,-186.170483118095,
-4.082198396148));
#33760=CARTESIAN_POINT('Ctrl Pts',(-9.42743337163542,-185.995483118095,
1.69768315121407E-11));
#33761=CARTESIAN_POINT('Ctrl Pts',(-7.07057502871922,-185.820483118095,
4.08219839617346));
#33762=CARTESIAN_POINT('Ctrl Pts',(-4.71371668580301,-185.645483118095,
8.16439679232994));
#33763=CARTESIAN_POINT('Ctrl Pts',(1.47018674401621E-11,-185.470483118095,
8.16439679232146));
#33764=CARTESIAN_POINT('Ctrl Pts',(4.71371668583241,-185.295483118095,8.16439679231297));
#33765=CARTESIAN_POINT('Ctrl Pts',(7.07057502873392,-185.120483118095,4.082198396148));
#33766=CARTESIAN_POINT('Ctrl Pts',(9.42743337163542,-184.945483118095,-1.69756769845304E-11));
#33767=CARTESIAN_POINT('Ctrl Pts',(7.07057502871922,-184.770483118095,-4.08219839617346));
#33768=CARTESIAN_POINT('Ctrl Pts',(4.71371668580301,-184.595483118095,-8.16439679232994));
#33769=CARTESIAN_POINT('Ctrl Pts',(-1.4702867290402E-11,-184.420483118095,
-8.16439679232146));
#33770=CARTESIAN_POINT('Ctrl Pts',(-4.71371668583241,-184.245483118095,
-8.16439679231297));
#33771=CARTESIAN_POINT('Ctrl Pts',(-7.07057502873392,-184.070483118095,
-4.082198396148));
#33772=CARTESIAN_POINT('Ctrl Pts',(-9.42743337163542,-183.895483118095,
1.69768315121407E-11));
#33773=CARTESIAN_POINT('Ctrl Pts',(-7.07057502871922,-183.720483118095,
4.08219839617346));
#33774=CARTESIAN_POINT('Ctrl Pts',(-4.71371668580301,-183.545483118095,
8.16439679232994));
#33775=CARTESIAN_POINT('Ctrl Pts',(1.47018674401621E-11,-183.370483118095,
8.16439679232146));
#33776=CARTESIAN_POINT('Ctrl Pts',(4.71371668583241,-183.195483118095,8.16439679231297));
#33777=CARTESIAN_POINT('Ctrl Pts',(7.07057502873392,-183.020483118095,4.082198396148));
#33778=CARTESIAN_POINT('Ctrl Pts',(9.42743337163542,-182.845483118095,-1.69756769845304E-11));
#33779=CARTESIAN_POINT('Ctrl Pts',(7.07057502871922,-182.670483118095,-4.08219839617346));
#33780=CARTESIAN_POINT('Ctrl Pts',(4.71371668580301,-182.495483118095,-8.16439679232994));
#33781=CARTESIAN_POINT('Ctrl Pts',(-1.4702867290402E-11,-182.320483118095,
-8.16439679232146));
#33782=CARTESIAN_POINT('Ctrl Pts',(-4.71371668583241,-182.145483118095,
-8.16439679231297));
#33783=CARTESIAN_POINT('Ctrl Pts',(-7.07057502873392,-181.970483118095,
-4.082198396148));
#33784=CARTESIAN_POINT('Ctrl Pts',(-9.42743337163542,-181.795483118095,
1.69768315121407E-11));
#33785=CARTESIAN_POINT('Ctrl Pts',(-7.07057502871922,-181.620483118095,
4.08219839617346));
#33786=CARTESIAN_POINT('Ctrl Pts',(-4.71371668580301,-181.445483118095,
8.16439679232994));
#33787=CARTESIAN_POINT('Ctrl Pts',(1.47018674401621E-11,-181.270483118095,
8.16439679232146));
#33788=CARTESIAN_POINT('Ctrl Pts',(4.71371668583241,-181.095483118095,8.16439679231297));
#33789=CARTESIAN_POINT('Ctrl Pts',(7.07057502873392,-180.920483118095,4.082198396148));
#33790=CARTESIAN_POINT('Ctrl Pts',(9.42743337163542,-180.745483118095,-1.69756769845304E-11));
#33791=CARTESIAN_POINT('Ctrl Pts',(7.07057502871922,-180.570483118095,-4.08219839617346));
#33792=CARTESIAN_POINT('Ctrl Pts',(4.71371668580301,-180.395483118095,-8.16439679232994));
#33793=CARTESIAN_POINT('Ctrl Pts',(-1.4702867290402E-11,-180.220483118095,
-8.16439679232146));
#33794=CARTESIAN_POINT('Ctrl Pts',(-4.71371668583241,-180.045483118095,
-8.16439679231297));
#33795=CARTESIAN_POINT('Ctrl Pts',(-7.07057502873392,-179.870483118095,
-4.082198396148));
#33796=CARTESIAN_POINT('Ctrl Pts',(-9.42743337163542,-179.695483118095,
1.69768315121407E-11));
#33797=CARTESIAN_POINT('Ctrl Pts',(-7.07057502871922,-179.520483118095,
4.08219839617346));
#33798=CARTESIAN_POINT('Ctrl Pts',(-4.71371668580301,-179.345483118095,
8.16439679232994));
#33799=CARTESIAN_POINT('Ctrl Pts',(1.47018674401621E-11,-179.170483118095,
8.16439679232146));
#33800=CARTESIAN_POINT('Ctrl Pts',(4.71371668583241,-178.995483118095,8.16439679231297));
#33801=CARTESIAN_POINT('Ctrl Pts',(7.07057502873392,-178.820483118095,4.082198396148));
#33802=CARTESIAN_POINT('Ctrl Pts',(9.42743337163542,-178.645483118095,-1.69756769845304E-11));
#33803=CARTESIAN_POINT('Ctrl Pts',(7.07057502871922,-178.470483118095,-4.08219839617346));
#33804=CARTESIAN_POINT('Ctrl Pts',(4.71371668580301,-178.295483118095,-8.16439679232994));
#33805=CARTESIAN_POINT('Ctrl Pts',(-1.4702867290402E-11,-178.120483118095,
-8.16439679232146));
#33806=CARTESIAN_POINT('Ctrl Pts',(-4.71371668583241,-177.945483118095,
-8.16439679231297));
#33807=CARTESIAN_POINT('Ctrl Pts',(-7.07057502873392,-177.770483118095,
-4.082198396148));
#33808=CARTESIAN_POINT('Ctrl Pts',(-9.42743337163542,-177.595483118095,
1.69768315121407E-11));
#33809=CARTESIAN_POINT('Ctrl Pts',(-7.07057502871922,-177.420483118095,
4.08219839617346));
#33810=CARTESIAN_POINT('Ctrl Pts',(-4.71371668580301,-177.245483118095,
8.16439679232994));
#33811=CARTESIAN_POINT('Ctrl Pts',(1.47018674401621E-11,-177.070483118095,
8.16439679232146));
#33812=CARTESIAN_POINT('Ctrl Pts',(4.71371668583241,-176.895483118095,8.16439679231297));
#33813=CARTESIAN_POINT('Ctrl Pts',(7.07057502873392,-176.720483118095,4.082198396148));
#33814=CARTESIAN_POINT('Ctrl Pts',(9.42743337163542,-176.545483118095,-1.69756769845304E-11));
#33815=CARTESIAN_POINT('Ctrl Pts',(7.07057502871922,-176.370483118095,-4.08219839617346));
#33816=CARTESIAN_POINT('Ctrl Pts',(4.71371668580301,-176.195483118095,-8.16439679232994));
#33817=CARTESIAN_POINT('Ctrl Pts',(-1.4702867290402E-11,-176.020483118095,
-8.16439679232146));
#33818=CARTESIAN_POINT('Ctrl Pts',(-4.71371668583241,-175.845483118095,
-8.16439679231297));
#33819=CARTESIAN_POINT('Ctrl Pts',(-7.07057502873392,-175.670483118095,
-4.082198396148));
#33820=CARTESIAN_POINT('Ctrl Pts',(-9.42743337163542,-175.495483118095,
1.69768315121407E-11));
#33821=CARTESIAN_POINT('Ctrl Pts',(-7.07057502871922,-175.320483118095,
4.08219839617346));
#33822=CARTESIAN_POINT('Ctrl Pts',(-4.71371668580301,-175.145483118095,
8.16439679232994));
#33823=CARTESIAN_POINT('Ctrl Pts',(1.47018674401621E-11,-174.970483118095,
8.16439679232146));
#33824=CARTESIAN_POINT('Ctrl Pts',(4.71371668583241,-174.795483118095,8.16439679231297));
#33825=CARTESIAN_POINT('Ctrl Pts',(7.07057502873392,-174.620483118095,4.082198396148));
#33826=CARTESIAN_POINT('Ctrl Pts',(9.42743337163542,-174.445483118095,-1.69756769845304E-11));
#33827=CARTESIAN_POINT('Ctrl Pts',(7.07057502871922,-174.270483118095,-4.08219839617346));
#33828=CARTESIAN_POINT('Ctrl Pts',(4.71371668580301,-174.095483118095,-8.16439679232994));
#33829=CARTESIAN_POINT('Ctrl Pts',(-1.4702867290402E-11,-173.920483118095,
-8.16439679232146));
#33830=CARTESIAN_POINT('Ctrl Pts',(-4.71371668583241,-173.745483118095,
-8.16439679231297));
#33831=CARTESIAN_POINT('Ctrl Pts',(-7.07057502873392,-173.570483118095,
-4.082198396148));
#33832=CARTESIAN_POINT('Ctrl Pts',(-9.42743337163542,-173.395483118095,
1.69768315121407E-11));
#33833=CARTESIAN_POINT('Ctrl Pts',(-7.07057502871922,-173.220483118095,
4.08219839617346));
#33834=CARTESIAN_POINT('Ctrl Pts',(-4.71371668580301,-173.045483118095,
8.16439679232994));
#33835=CARTESIAN_POINT('Ctrl Pts',(1.47018674401621E-11,-172.870483118095,
8.16439679232146));
#33836=CARTESIAN_POINT('Ctrl Pts',(4.71371668583241,-172.695483118095,8.16439679231297));
#33837=CARTESIAN_POINT('Ctrl Pts',(7.07057502873392,-172.520483118095,4.082198396148));
#33838=CARTESIAN_POINT('Ctrl Pts',(9.42743337163542,-172.345483118095,-1.69756769845304E-11));
#33839=CARTESIAN_POINT('Ctrl Pts',(7.07057502871922,-172.170483118095,-4.08219839617346));
#33840=CARTESIAN_POINT('Ctrl Pts',(4.71371668580301,-171.995483118095,-8.16439679232994));
#33841=CARTESIAN_POINT('Ctrl Pts',(-1.4702867290402E-11,-171.820483118095,
-8.16439679232146));
#33842=CARTESIAN_POINT('Ctrl Pts',(-4.71371668583241,-171.645483118095,
-8.16439679231297));
#33843=CARTESIAN_POINT('Ctrl Pts',(-7.07057502873392,-171.470483118095,
-4.082198396148));
#33844=CARTESIAN_POINT('Ctrl Pts',(-9.42743337163542,-171.295483118095,
1.69768315121407E-11));
#33845=CARTESIAN_POINT('Ctrl Pts',(-7.07057502871922,-171.120483118095,
4.08219839617346));
#33846=CARTESIAN_POINT('Ctrl Pts',(-4.71371668580301,-170.945483118095,
8.16439679232994));
#33847=CARTESIAN_POINT('Ctrl Pts',(1.47018674401621E-11,-170.770483118095,
8.16439679232146));
#33848=CARTESIAN_POINT('Ctrl Pts',(4.71371668583241,-170.595483118095,8.16439679231297));
#33849=CARTESIAN_POINT('Ctrl Pts',(7.07057502873392,-170.420483118095,4.082198396148));
#33850=CARTESIAN_POINT('Ctrl Pts',(9.42743337163542,-170.245483118095,-1.69756769845304E-11));
#33851=CARTESIAN_POINT('Ctrl Pts',(7.07057502871922,-170.070483118095,-4.08219839617346));
#33852=CARTESIAN_POINT('Ctrl Pts',(4.71371668580301,-169.895483118095,-8.16439679232994));
#33853=CARTESIAN_POINT('Ctrl Pts',(-1.4702867290402E-11,-169.720483118095,
-8.16439679232146));
#33854=CARTESIAN_POINT('Ctrl Pts',(-4.71371668583241,-169.545483118095,
-8.16439679231297));
#33855=CARTESIAN_POINT('Ctrl Pts',(-7.07057502873392,-169.370483118095,
-4.082198396148));
#33856=CARTESIAN_POINT('Ctrl Pts',(-9.42743337163542,-169.195483118095,
1.69768315121407E-11));
#33857=CARTESIAN_POINT('Ctrl Pts',(-7.07057502871922,-169.020483118095,
4.08219839617346));
#33858=CARTESIAN_POINT('Ctrl Pts',(-4.71371668580301,-168.845483118095,
8.16439679232994));
#33859=CARTESIAN_POINT('Ctrl Pts',(1.47018674401621E-11,-168.670483118095,
8.16439679232146));
#33860=CARTESIAN_POINT('Ctrl Pts',(4.71371668583241,-168.495483118095,8.16439679231297));
#33861=CARTESIAN_POINT('Ctrl Pts',(7.07057502873392,-168.320483118095,4.082198396148));
#33862=CARTESIAN_POINT('Ctrl Pts',(9.42743337163542,-168.145483118095,-1.69756769845304E-11));
#33863=CARTESIAN_POINT('Ctrl Pts',(7.07057502871922,-167.970483118095,-4.08219839617346));
#33864=CARTESIAN_POINT('Ctrl Pts',(4.71371668580301,-167.795483118095,-8.16439679232994));
#33865=CARTESIAN_POINT('Ctrl Pts',(-1.4702867290402E-11,-167.620483118095,
-8.16439679232146));
#33866=CARTESIAN_POINT('Ctrl Pts',(-4.71371668583241,-167.445483118095,
-8.16439679231297));
#33867=CARTESIAN_POINT('Ctrl Pts',(-7.07057502873392,-167.270483118095,
-4.082198396148));
#33868=CARTESIAN_POINT('Ctrl Pts',(-9.42743337163542,-167.095483118095,
1.69768315121407E-11));
#33869=CARTESIAN_POINT('Ctrl Pts',(-7.07057502871922,-166.920483118095,
4.08219839617346));
#33870=CARTESIAN_POINT('Ctrl Pts',(-4.71371668580301,-166.745483118095,
8.16439679232994));
#33871=CARTESIAN_POINT('Ctrl Pts',(1.47018674401621E-11,-166.570483118095,
8.16439679232146));
#33872=CARTESIAN_POINT('Ctrl Pts',(4.71371668583241,-166.395483118095,8.16439679231297));
#33873=CARTESIAN_POINT('Ctrl Pts',(7.07057502873392,-166.220483118095,4.082198396148));
#33874=CARTESIAN_POINT('Ctrl Pts',(9.42743337163542,-166.045483118095,-1.69756769845304E-11));
#33875=CARTESIAN_POINT('Ctrl Pts',(7.07057502871922,-165.870483118095,-4.08219839617346));
#33876=CARTESIAN_POINT('Ctrl Pts',(4.71371668580301,-165.695483118095,-8.16439679232994));
#33877=CARTESIAN_POINT('Ctrl Pts',(-1.4702867290402E-11,-165.520483118095,
-8.16439679232146));
#33878=CARTESIAN_POINT('Ctrl Pts',(-4.71371668583241,-165.345483118095,
-8.16439679231297));
#33879=CARTESIAN_POINT('Ctrl Pts',(-7.07057502873392,-165.170483118095,
-4.082198396148));
#33880=CARTESIAN_POINT('Ctrl Pts',(-9.42743337163542,-164.995483118095,
1.69768315121407E-11));
#33881=CARTESIAN_POINT('Ctrl Pts',(-7.07057502871922,-164.820483118095,
4.08219839617346));
#33882=CARTESIAN_POINT('Ctrl Pts',(-4.71371668580301,-164.645483118095,
8.16439679232994));
#33883=CARTESIAN_POINT('Ctrl Pts',(1.47018674401621E-11,-164.470483118095,
8.16439679232146));
#33884=CARTESIAN_POINT('Ctrl Pts',(4.71371668583241,-164.295483118095,8.16439679231297));
#33885=CARTESIAN_POINT('Ctrl Pts',(7.07057502873392,-164.120483118095,4.082198396148));
#33886=CARTESIAN_POINT('Ctrl Pts',(9.42743337163542,-163.945483118095,-1.69756769845304E-11));
#33887=CARTESIAN_POINT('Ctrl Pts',(7.07057502871922,-163.770483118095,-4.08219839617346));
#33888=CARTESIAN_POINT('Ctrl Pts',(4.71371668580301,-163.595483118095,-8.16439679232994));
#33889=CARTESIAN_POINT('Ctrl Pts',(-1.4702867290402E-11,-163.420483118095,
-8.16439679232146));
#33890=CARTESIAN_POINT('Ctrl Pts',(-4.71371668583241,-163.245483118095,
-8.16439679231297));
#33891=CARTESIAN_POINT('Ctrl Pts',(-7.07057502873392,-163.070483118095,
-4.082198396148));
#33892=CARTESIAN_POINT('Ctrl Pts',(-9.42743337163542,-162.895483118095,
1.69768315121407E-11));
#33893=CARTESIAN_POINT('Ctrl Pts',(-7.07057502871922,-162.720483118095,
4.08219839617346));
#33894=CARTESIAN_POINT('Ctrl Pts',(-4.71371668580301,-162.545483118095,
8.16439679232994));
#33895=CARTESIAN_POINT('Ctrl Pts',(1.47018674401621E-11,-162.370483118095,
8.16439679232146));
#33896=CARTESIAN_POINT('Ctrl Pts',(4.71371668583241,-162.195483118095,8.16439679231297));
#33897=CARTESIAN_POINT('Ctrl Pts',(7.07057502873392,-162.020483118095,4.082198396148));
#33898=CARTESIAN_POINT('Ctrl Pts',(9.42743337163542,-161.845483118095,-1.69756769845304E-11));
#33899=CARTESIAN_POINT('Ctrl Pts',(7.07057502871922,-161.670483118095,-4.08219839617346));
#33900=CARTESIAN_POINT('Ctrl Pts',(4.71371668580301,-161.495483118095,-8.16439679232994));
#33901=CARTESIAN_POINT('Ctrl Pts',(-1.4702867290402E-11,-161.320483118095,
-8.16439679232146));
#33902=CARTESIAN_POINT('Ctrl Pts',(-4.71371668583241,-161.145483118095,
-8.16439679231297));
#33903=CARTESIAN_POINT('Ctrl Pts',(-7.07057502873392,-160.970483118095,
-4.082198396148));
#33904=CARTESIAN_POINT('Ctrl Pts',(-9.42743337163542,-160.795483118095,
1.69768315121407E-11));
#33905=CARTESIAN_POINT('Ctrl Pts',(-7.07057502871922,-160.620483118095,
4.08219839617346));
#33906=CARTESIAN_POINT('Ctrl Pts',(-4.71371668580301,-160.445483118095,
8.16439679232994));
#33907=CARTESIAN_POINT('Ctrl Pts',(1.47018674401621E-11,-160.270483118095,
8.16439679232146));
#33908=CARTESIAN_POINT('Ctrl Pts',(4.71371668583241,-160.095483118095,8.16439679231297));
#33909=CARTESIAN_POINT('Ctrl Pts',(7.07057502873392,-159.920483118095,4.082198396148));
#33910=CARTESIAN_POINT('Ctrl Pts',(9.42743337163542,-159.745483118095,-1.69756769845304E-11));
#33911=CARTESIAN_POINT('Ctrl Pts',(7.07057502871922,-159.570483118095,-4.08219839617346));
#33912=CARTESIAN_POINT('Ctrl Pts',(4.71371668580301,-159.395483118095,-8.16439679232994));
#33913=CARTESIAN_POINT('Ctrl Pts',(-1.4702867290402E-11,-159.220483118095,
-8.16439679232146));
#33914=CARTESIAN_POINT('Ctrl Pts',(-4.71371668583241,-159.045483118095,
-8.16439679231297));
#33915=CARTESIAN_POINT('Ctrl Pts',(-7.07057502873392,-158.870483118095,
-4.082198396148));
#33916=CARTESIAN_POINT('Ctrl Pts',(-9.42743337163542,-158.695483118095,
1.69768315121407E-11));
#33917=CARTESIAN_POINT('Ctrl Pts',(-7.07057502871922,-158.520483118095,
4.08219839617346));
#33918=CARTESIAN_POINT('Ctrl Pts',(-4.71371668580301,-158.345483118095,
8.16439679232994));
#33919=CARTESIAN_POINT('Ctrl Pts',(1.47018674401621E-11,-158.170483118095,
8.16439679232146));
#33920=CARTESIAN_POINT('Ctrl Pts',(4.71371668583241,-157.995483118095,8.16439679231297));
#33921=CARTESIAN_POINT('Ctrl Pts',(7.07057502873392,-157.820483118095,4.082198396148));
#33922=CARTESIAN_POINT('Ctrl Pts',(9.42743337163542,-157.645483118095,-1.69756769845304E-11));
#33923=CARTESIAN_POINT('Ctrl Pts',(7.07057502871922,-157.470483118095,-4.08219839617346));
#33924=CARTESIAN_POINT('Ctrl Pts',(4.71371668580301,-157.295483118095,-8.16439679232994));
#33925=CARTESIAN_POINT('Ctrl Pts',(-1.4702867290402E-11,-157.120483118095,
-8.16439679232146));
#33926=CARTESIAN_POINT('Ctrl Pts',(-4.71371668583241,-156.945483118095,
-8.16439679231297));
#33927=CARTESIAN_POINT('Ctrl Pts',(-7.07057502873392,-156.770483118095,
-4.082198396148));
#33928=CARTESIAN_POINT('Ctrl Pts',(-9.42743337163542,-156.595483118095,
1.69768315121407E-11));
#33929=CARTESIAN_POINT('Ctrl Pts',(-7.07057502871922,-156.420483118095,
4.08219839617346));
#33930=CARTESIAN_POINT('Ctrl Pts',(-4.71371668580301,-156.245483118095,
8.16439679232994));
#33931=CARTESIAN_POINT('Ctrl Pts',(1.47018674401621E-11,-156.070483118095,
8.16439679232146));
#33932=CARTESIAN_POINT('Ctrl Pts',(4.71371668583241,-155.895483118095,8.16439679231297));
#33933=CARTESIAN_POINT('Ctrl Pts',(7.07057502873392,-155.720483118095,4.082198396148));
#33934=CARTESIAN_POINT('Ctrl Pts',(9.42743337163542,-155.545483118095,-1.69756769845304E-11));
#33935=CARTESIAN_POINT('Ctrl Pts',(7.07057502871922,-155.370483118095,-4.08219839617346));
#33936=CARTESIAN_POINT('Ctrl Pts',(4.71371668580301,-155.195483118095,-8.16439679232994));
#33937=CARTESIAN_POINT('Ctrl Pts',(-1.4702867290402E-11,-155.020483118095,
-8.16439679232146));
#33938=CARTESIAN_POINT('Ctrl Pts',(-4.71371668583241,-154.845483118095,
-8.16439679231297));
#33939=CARTESIAN_POINT('Ctrl Pts',(-7.07057502873392,-154.670483118095,
-4.082198396148));
#33940=CARTESIAN_POINT('Ctrl Pts',(-9.42743337163542,-154.495483118095,
1.69768315121407E-11));
#33941=CARTESIAN_POINT('Ctrl Pts',(-7.07057502871922,-154.320483118095,
4.08219839617346));
#33942=CARTESIAN_POINT('Ctrl Pts',(-4.71371668580301,-154.145483118095,
8.16439679232994));
#33943=CARTESIAN_POINT('Ctrl Pts',(1.47018674401621E-11,-153.970483118095,
8.16439679232146));
#33944=CARTESIAN_POINT('Ctrl Pts',(4.71371668583241,-153.795483118095,8.16439679231297));
#33945=CARTESIAN_POINT('Ctrl Pts',(7.07057502873392,-153.620483118095,4.082198396148));
#33946=CARTESIAN_POINT('Ctrl Pts',(9.42743337163542,-153.445483118095,-1.69756769845304E-11));
#33947=CARTESIAN_POINT('Ctrl Pts',(7.07057502871922,-153.270483118095,-4.08219839617346));
#33948=CARTESIAN_POINT('Ctrl Pts',(4.71371668580301,-153.095483118095,-8.16439679232994));
#33949=CARTESIAN_POINT('Ctrl Pts',(-1.4702867290402E-11,-152.920483118095,
-8.16439679232146));
#33950=CARTESIAN_POINT('Ctrl Pts',(-4.71371668583241,-152.745483118095,
-8.16439679231297));
#33951=CARTESIAN_POINT('Ctrl Pts',(-7.07057502873392,-152.570483118095,
-4.082198396148));
#33952=CARTESIAN_POINT('Ctrl Pts',(-9.42743337163542,-152.395483118095,
1.69768315121407E-11));
#33953=CARTESIAN_POINT('Ctrl Pts',(-7.07057502871922,-152.220483118095,
4.08219839617346));
#33954=CARTESIAN_POINT('Ctrl Pts',(-4.71371668580301,-152.045483118095,
8.16439679232994));
#33955=CARTESIAN_POINT('Ctrl Pts',(1.47018674401621E-11,-151.870483118095,
8.16439679232146));
#33956=CARTESIAN_POINT('Ctrl Pts',(4.71371668583241,-151.695483118095,8.16439679231297));
#33957=CARTESIAN_POINT('Ctrl Pts',(7.07057502873392,-151.520483118095,4.082198396148));
#33958=CARTESIAN_POINT('Ctrl Pts',(9.42743337163542,-151.345483118095,-1.69756769845304E-11));
#33959=CARTESIAN_POINT('Ctrl Pts',(7.07057502871922,-151.170483118095,-4.08219839617346));
#33960=CARTESIAN_POINT('Ctrl Pts',(4.71371668580301,-150.995483118095,-8.16439679232994));
#33961=CARTESIAN_POINT('Ctrl Pts',(-1.4702867290402E-11,-150.820483118095,
-8.16439679232146));
#33962=CARTESIAN_POINT('Ctrl Pts',(-4.71371668583241,-150.645483118095,
-8.16439679231297));
#33963=CARTESIAN_POINT('Ctrl Pts',(-7.07057502873392,-150.470483118095,
-4.082198396148));
#33964=CARTESIAN_POINT('Ctrl Pts',(-9.42743337163542,-150.295483118095,
1.69768315121407E-11));
#33965=CARTESIAN_POINT('Ctrl Pts',(-7.07057502871922,-150.120483118095,
4.08219839617346));
#33966=CARTESIAN_POINT('Ctrl Pts',(-4.71371668580301,-149.945483118095,
8.16439679232994));
#33967=CARTESIAN_POINT('Ctrl Pts',(1.47018674401621E-11,-149.770483118095,
8.16439679232146));
#33968=CARTESIAN_POINT('Ctrl Pts',(4.71371668583241,-149.595483118095,8.16439679231297));
#33969=CARTESIAN_POINT('Ctrl Pts',(7.07057502873392,-149.420483118095,4.082198396148));
#33970=CARTESIAN_POINT('Ctrl Pts',(9.42743337163542,-149.245483118095,-1.69756769845304E-11));
#33971=CARTESIAN_POINT('Ctrl Pts',(7.07057502871922,-149.070483118095,-4.08219839617346));
#33972=CARTESIAN_POINT('Ctrl Pts',(4.71371668580301,-148.895483118095,-8.16439679232994));
#33973=CARTESIAN_POINT('Ctrl Pts',(-1.4702867290402E-11,-148.720483118095,
-8.16439679232146));
#33974=CARTESIAN_POINT('Ctrl Pts',(-4.71371668583241,-148.545483118095,
-8.16439679231297));
#33975=CARTESIAN_POINT('Ctrl Pts',(-7.07057502873392,-148.370483118095,
-4.082198396148));
#33976=CARTESIAN_POINT('Ctrl Pts',(-9.42743337163542,-148.195483118095,
1.69768315121407E-11));
#33977=CARTESIAN_POINT('Ctrl Pts',(-7.07057502871922,-148.020483118095,
4.08219839617346));
#33978=CARTESIAN_POINT('Ctrl Pts',(-4.71371668580301,-147.845483118095,
8.16439679232994));
#33979=CARTESIAN_POINT('Ctrl Pts',(1.47018674401621E-11,-147.670483118095,
8.16439679232146));
#33980=CARTESIAN_POINT('Ctrl Pts',(4.71371668583241,-147.495483118095,8.16439679231297));
#33981=CARTESIAN_POINT('Ctrl Pts',(7.07057502873392,-147.320483118095,4.082198396148));
#33982=CARTESIAN_POINT('Ctrl Pts',(9.42743337163542,-147.145483118095,-1.69756769845304E-11));
#33983=CARTESIAN_POINT('Ctrl Pts',(7.07057502871922,-146.970483118095,-4.08219839617346));
#33984=CARTESIAN_POINT('Ctrl Pts',(4.71371668580301,-146.795483118095,-8.16439679232994));
#33985=CARTESIAN_POINT('Ctrl Pts',(-1.4702867290402E-11,-146.620483118095,
-8.16439679232146));
#33986=CARTESIAN_POINT('Ctrl Pts',(-4.71371668583241,-146.445483118095,
-8.16439679231297));
#33987=CARTESIAN_POINT('Ctrl Pts',(-7.07057502873392,-146.270483118095,
-4.082198396148));
#33988=CARTESIAN_POINT('Ctrl Pts',(-9.42743337163542,-146.095483118095,
1.69768315121407E-11));
#33989=CARTESIAN_POINT('Ctrl Pts',(-7.07057502871922,-145.920483118095,
4.08219839617346));
#33990=CARTESIAN_POINT('Ctrl Pts',(-4.71371668580301,-145.745483118095,
8.16439679232994));
#33991=CARTESIAN_POINT('Ctrl Pts',(1.47018674401621E-11,-145.570483118095,
8.16439679232146));
#33992=CARTESIAN_POINT('Ctrl Pts',(4.71371668583241,-145.395483118095,8.16439679231297));
#33993=CARTESIAN_POINT('Ctrl Pts',(7.07057502873392,-145.220483118095,4.082198396148));
#33994=CARTESIAN_POINT('Ctrl Pts',(9.42743337163542,-145.045483118095,-1.69756769845304E-11));
#33995=CARTESIAN_POINT('Ctrl Pts',(7.07057502871922,-144.870483118095,-4.08219839617346));
#33996=CARTESIAN_POINT('Ctrl Pts',(4.71371668580301,-144.695483118095,-8.16439679232994));
#33997=CARTESIAN_POINT('Ctrl Pts',(-1.4702867290402E-11,-144.520483118095,
-8.16439679232146));
#33998=CARTESIAN_POINT('Ctrl Pts',(-4.71371668583241,-144.345483118095,
-8.16439679231297));
#33999=CARTESIAN_POINT('Ctrl Pts',(-7.07057502873392,-144.170483118095,
-4.082198396148));
#34000=CARTESIAN_POINT('Ctrl Pts',(-9.42743337163542,-143.995483118095,
1.69768315121407E-11));
#34001=CARTESIAN_POINT('Ctrl Pts',(-7.07057502871922,-143.820483118095,
4.08219839617346));
#34002=CARTESIAN_POINT('Ctrl Pts',(-4.71371668580301,-143.645483118095,
8.16439679232994));
#34003=CARTESIAN_POINT('Ctrl Pts',(1.47018674401621E-11,-143.470483118095,
8.16439679232146));
#34004=CARTESIAN_POINT('Ctrl Pts',(4.71371668583241,-143.295483118095,8.16439679231297));
#34005=CARTESIAN_POINT('Ctrl Pts',(7.07057502873392,-143.120483118095,4.082198396148));
#34006=CARTESIAN_POINT('Ctrl Pts',(9.42743337163542,-142.945483118095,-1.69756769845304E-11));
#34007=CARTESIAN_POINT('Ctrl Pts',(7.07057502871922,-142.770483118095,-4.08219839617346));
#34008=CARTESIAN_POINT('Ctrl Pts',(4.71371668580301,-142.595483118095,-8.16439679232994));
#34009=CARTESIAN_POINT('Ctrl Pts',(-1.4702867290402E-11,-142.420483118095,
-8.16439679232146));
#34010=CARTESIAN_POINT('Ctrl Pts',(-4.71371668583241,-142.245483118095,
-8.16439679231297));
#34011=CARTESIAN_POINT('Ctrl Pts',(-7.07057502873392,-142.070483118095,
-4.082198396148));
#34012=CARTESIAN_POINT('Ctrl Pts',(-9.42743337163542,-141.895483118095,
1.69768315121407E-11));
#34013=CARTESIAN_POINT('Ctrl Pts',(-7.07057502871922,-141.720483118095,
4.08219839617346));
#34014=CARTESIAN_POINT('Ctrl Pts',(-4.71371668580301,-141.545483118095,
8.16439679232994));
#34015=CARTESIAN_POINT('Ctrl Pts',(1.47018674401621E-11,-141.370483118095,
8.16439679232146));
#34016=CARTESIAN_POINT('Ctrl Pts',(4.71371668583241,-141.195483118095,8.16439679231297));
#34017=CARTESIAN_POINT('Ctrl Pts',(7.07057502873392,-141.020483118095,4.082198396148));
#34018=CARTESIAN_POINT('Ctrl Pts',(9.42743337163542,-140.845483118095,-1.69756769845304E-11));
#34019=CARTESIAN_POINT('Ctrl Pts',(7.07057502871922,-140.670483118095,-4.08219839617346));
#34020=CARTESIAN_POINT('Ctrl Pts',(4.71371668580301,-140.495483118095,-8.16439679232994));
#34021=CARTESIAN_POINT('Ctrl Pts',(-1.4702867290402E-11,-140.320483118095,
-8.16439679232146));
#34022=CARTESIAN_POINT('Ctrl Pts',(-4.71371668583241,-140.145483118095,
-8.16439679231297));
#34023=CARTESIAN_POINT('Ctrl Pts',(-7.07057502873392,-139.970483118095,
-4.082198396148));
#34024=CARTESIAN_POINT('Ctrl Pts',(-9.42743337163542,-139.795483118095,
1.69768315121407E-11));
#34025=CARTESIAN_POINT('Ctrl Pts',(-7.07057502871922,-139.620483118095,
4.08219839617346));
#34026=CARTESIAN_POINT('Ctrl Pts',(-4.71371668580301,-139.445483118095,
8.16439679232994));
#34027=CARTESIAN_POINT('Ctrl Pts',(1.47018674401621E-11,-139.270483118095,
8.16439679232146));
#34028=CARTESIAN_POINT('Ctrl Pts',(4.71371668583241,-139.095483118095,8.16439679231297));
#34029=CARTESIAN_POINT('Ctrl Pts',(7.07057502873392,-138.920483118095,4.082198396148));
#34030=CARTESIAN_POINT('Ctrl Pts',(9.42743337163542,-138.745483118095,-1.69756769845304E-11));
#34031=CARTESIAN_POINT('Ctrl Pts',(7.07057502871922,-138.570483118095,-4.08219839617346));
#34032=CARTESIAN_POINT('Ctrl Pts',(4.71371668580301,-138.395483118095,-8.16439679232994));
#34033=CARTESIAN_POINT('Ctrl Pts',(-1.4702867290402E-11,-138.220483118095,
-8.16439679232146));
#34034=CARTESIAN_POINT('Ctrl Pts',(-4.71371668583241,-138.045483118095,
-8.16439679231297));
#34035=CARTESIAN_POINT('Ctrl Pts',(-7.07057502873392,-137.870483118095,
-4.082198396148));
#34036=CARTESIAN_POINT('Ctrl Pts',(-9.42743337163542,-137.695483118095,
1.69768315121407E-11));
#34037=CARTESIAN_POINT('Ctrl Pts',(-7.07057502871922,-137.520483118095,
4.08219839617346));
#34038=CARTESIAN_POINT('Ctrl Pts',(-4.71371668580301,-137.345483118095,
8.16439679232994));
#34039=CARTESIAN_POINT('Ctrl Pts',(1.47018674401621E-11,-137.170483118095,
8.16439679232146));
#34040=CARTESIAN_POINT('Ctrl Pts',(4.71371668583241,-136.995483118095,8.16439679231297));
#34041=CARTESIAN_POINT('Ctrl Pts',(7.07057502873392,-136.820483118095,4.082198396148));
#34042=CARTESIAN_POINT('Ctrl Pts',(9.42743337163542,-136.645483118095,-1.69756769845304E-11));
#34043=CARTESIAN_POINT('Ctrl Pts',(7.07057502871922,-136.470483118095,-4.08219839617346));
#34044=CARTESIAN_POINT('Ctrl Pts',(4.71371668580301,-136.295483118095,-8.16439679232994));
#34045=CARTESIAN_POINT('Ctrl Pts',(-1.4702867290402E-11,-136.120483118095,
-8.16439679232146));
#34046=CARTESIAN_POINT('Ctrl Pts',(-4.71371668583241,-135.945483118095,
-8.16439679231297));
#34047=CARTESIAN_POINT('Ctrl Pts',(-7.07057502873392,-135.770483118095,
-4.082198396148));
#34048=CARTESIAN_POINT('Ctrl Pts',(-9.42743337163542,-135.595483118095,
1.69768315121407E-11));
#34049=CARTESIAN_POINT('Ctrl Pts',(-7.07057502871922,-135.420483118095,
4.08219839617346));
#34050=CARTESIAN_POINT('Ctrl Pts',(-4.71371668580301,-135.245483118095,
8.16439679232994));
#34051=CARTESIAN_POINT('Ctrl Pts',(1.47018674401621E-11,-135.070483118095,
8.16439679232146));
#34052=CARTESIAN_POINT('Ctrl Pts',(4.71371668583241,-134.895483118095,8.16439679231297));
#34053=CARTESIAN_POINT('Ctrl Pts',(7.07057502873392,-134.720483118095,4.082198396148));
#34054=CARTESIAN_POINT('Ctrl Pts',(9.42743337163542,-134.545483118095,-1.69756769845304E-11));
#34055=CARTESIAN_POINT('Ctrl Pts',(7.07057502871922,-134.370483118095,-4.08219839617346));
#34056=CARTESIAN_POINT('Ctrl Pts',(4.71371668580301,-134.195483118095,-8.16439679232994));
#34057=CARTESIAN_POINT('Ctrl Pts',(-1.4702867290402E-11,-134.020483118095,
-8.16439679232146));
#34058=CARTESIAN_POINT('Ctrl Pts',(-4.71371668583241,-133.845483118095,
-8.16439679231297));
#34059=CARTESIAN_POINT('Ctrl Pts',(-7.07057502873392,-133.670483118095,
-4.082198396148));
#34060=CARTESIAN_POINT('Ctrl Pts',(-9.42743337163542,-133.495483118095,
1.69768315121407E-11));
#34061=CARTESIAN_POINT('Ctrl Pts',(-7.07057502871922,-133.320483118095,
4.08219839617346));
#34062=CARTESIAN_POINT('Ctrl Pts',(-4.71371668580301,-133.145483118095,
8.16439679232994));
#34063=CARTESIAN_POINT('Ctrl Pts',(1.47018674401621E-11,-132.970483118095,
8.16439679232146));
#34064=CARTESIAN_POINT('Ctrl Pts',(4.71371668583241,-132.795483118095,8.16439679231297));
#34065=CARTESIAN_POINT('Ctrl Pts',(7.07057502873392,-132.620483118095,4.082198396148));
#34066=CARTESIAN_POINT('Ctrl Pts',(9.42743337163542,-132.445483118095,-1.69756769845304E-11));
#34067=CARTESIAN_POINT('Ctrl Pts',(7.07057502871922,-132.270483118095,-4.08219839617346));
#34068=CARTESIAN_POINT('Ctrl Pts',(4.71371668580301,-132.095483118095,-8.16439679232994));
#34069=CARTESIAN_POINT('Ctrl Pts',(-1.4702867290402E-11,-131.920483118095,
-8.16439679232146));
#34070=CARTESIAN_POINT('Ctrl Pts',(-4.71371668583241,-131.745483118095,
-8.16439679231297));
#34071=CARTESIAN_POINT('Ctrl Pts',(-7.07057502873392,-131.570483118095,
-4.082198396148));
#34072=CARTESIAN_POINT('Ctrl Pts',(-9.42743337163542,-131.395483118095,
1.69768315121407E-11));
#34073=CARTESIAN_POINT('Ctrl Pts',(-7.07057502871922,-131.220483118095,
4.08219839617346));
#34074=CARTESIAN_POINT('Ctrl Pts',(-4.71371668580301,-131.045483118095,
8.16439679232994));
#34075=CARTESIAN_POINT('Ctrl Pts',(1.47018674401621E-11,-130.870483118095,
8.16439679232146));
#34076=CARTESIAN_POINT('Ctrl Pts',(4.71371668583241,-130.695483118095,8.16439679231297));
#34077=CARTESIAN_POINT('Ctrl Pts',(7.07057502873392,-130.520483118095,4.082198396148));
#34078=CARTESIAN_POINT('Ctrl Pts',(9.42743337163542,-130.345483118095,-1.69756769845304E-11));
#34079=CARTESIAN_POINT('Ctrl Pts',(7.07057502871922,-130.170483118095,-4.08219839617346));
#34080=CARTESIAN_POINT('Ctrl Pts',(4.71371668580301,-129.995483118095,-8.16439679232994));
#34081=CARTESIAN_POINT('Ctrl Pts',(-1.4702867290402E-11,-129.820483118095,
-8.16439679232146));
#34082=CARTESIAN_POINT('Ctrl Pts',(-4.71371668583241,-129.645483118095,
-8.16439679231297));
#34083=CARTESIAN_POINT('Ctrl Pts',(-7.07057502873392,-129.470483118095,
-4.082198396148));
#34084=CARTESIAN_POINT('Ctrl Pts',(-9.42743337163542,-129.295483118095,
1.69768315121407E-11));
#34085=CARTESIAN_POINT('Ctrl Pts',(-7.07057502871922,-129.120483118095,
4.08219839617346));
#34086=CARTESIAN_POINT('Ctrl Pts',(-4.71371668580301,-128.945483118095,
8.16439679232994));
#34087=CARTESIAN_POINT('Ctrl Pts',(1.47018674401621E-11,-128.770483118095,
8.16439679232146));
#34088=CARTESIAN_POINT('Ctrl Pts',(4.71371668583241,-128.595483118095,8.16439679231297));
#34089=CARTESIAN_POINT('Ctrl Pts',(7.07057502873392,-128.420483118095,4.082198396148));
#34090=CARTESIAN_POINT('Ctrl Pts',(9.42743337163542,-128.245483118095,-1.69756769845304E-11));
#34091=CARTESIAN_POINT('Ctrl Pts',(7.07057502871922,-128.070483118095,-4.08219839617346));
#34092=CARTESIAN_POINT('Ctrl Pts',(4.71371668580301,-127.895483118095,-8.16439679232994));
#34093=CARTESIAN_POINT('Ctrl Pts',(-1.4702867290402E-11,-127.720483118095,
-8.16439679232146));
#34094=CARTESIAN_POINT('Ctrl Pts',(-4.71371668583241,-127.545483118095,
-8.16439679231297));
#34095=CARTESIAN_POINT('Ctrl Pts',(-7.07057502873392,-127.370483118095,
-4.082198396148));
#34096=CARTESIAN_POINT('Ctrl Pts',(-9.42743337163542,-127.195483118095,
1.69768315121407E-11));
#34097=CARTESIAN_POINT('Ctrl Pts',(-7.07057502871922,-127.020483118095,
4.08219839617346));
#34098=CARTESIAN_POINT('Ctrl Pts',(-4.71371668580301,-126.845483118095,
8.16439679232994));
#34099=CARTESIAN_POINT('Ctrl Pts',(1.47018674401621E-11,-126.670483118095,
8.16439679232146));
#34100=CARTESIAN_POINT('Ctrl Pts',(4.71371668583241,-126.495483118095,8.16439679231297));
#34101=CARTESIAN_POINT('Ctrl Pts',(7.07057502873392,-126.320483118095,4.082198396148));
#34102=CARTESIAN_POINT('Ctrl Pts',(9.42743337163542,-126.145483118095,-1.69756769845304E-11));
#34103=CARTESIAN_POINT('Ctrl Pts',(7.07057502871922,-125.970483118095,-4.08219839617346));
#34104=CARTESIAN_POINT('Ctrl Pts',(4.71371668580301,-125.795483118095,-8.16439679232994));
#34105=CARTESIAN_POINT('Ctrl Pts',(-1.4702867290402E-11,-125.620483118095,
-8.16439679232146));
#34106=CARTESIAN_POINT('Ctrl Pts',(-4.71371668583241,-125.445483118095,
-8.16439679231297));
#34107=CARTESIAN_POINT('Ctrl Pts',(-7.07057502873392,-125.270483118095,
-4.082198396148));
#34108=CARTESIAN_POINT('Ctrl Pts',(-9.42743337163542,-125.095483118095,
1.69768315121407E-11));
#34109=CARTESIAN_POINT('Ctrl Pts',(-7.07057502871922,-124.920483118095,
4.08219839617346));
#34110=CARTESIAN_POINT('Ctrl Pts',(-4.71371668580301,-124.745483118095,
8.16439679232994));
#34111=CARTESIAN_POINT('Ctrl Pts',(1.47018674401621E-11,-124.570483118095,
8.16439679232146));
#34112=CARTESIAN_POINT('Ctrl Pts',(4.71371668583241,-124.395483118095,8.16439679231297));
#34113=CARTESIAN_POINT('Ctrl Pts',(7.07057502873392,-124.220483118095,4.082198396148));
#34114=CARTESIAN_POINT('Ctrl Pts',(9.42743337163542,-124.045483118095,-1.69756769845304E-11));
#34115=CARTESIAN_POINT('Ctrl Pts',(7.07057502871922,-123.870483118095,-4.08219839617346));
#34116=CARTESIAN_POINT('Ctrl Pts',(4.71371668580301,-123.695483118095,-8.16439679232994));
#34117=CARTESIAN_POINT('Ctrl Pts',(-1.4702867290402E-11,-123.520483118095,
-8.16439679232146));
#34118=CARTESIAN_POINT('Ctrl Pts',(-4.71371668583241,-123.345483118095,
-8.16439679231297));
#34119=CARTESIAN_POINT('Ctrl Pts',(-7.07057502873392,-123.170483118095,
-4.082198396148));
#34120=CARTESIAN_POINT('Ctrl Pts',(-9.42743337163542,-122.995483118095,
1.69768315121407E-11));
#34121=CARTESIAN_POINT('Ctrl Pts',(-7.07057502871922,-122.820483118095,
4.08219839617346));
#34122=CARTESIAN_POINT('Ctrl Pts',(-4.71371668580301,-122.645483118095,
8.16439679232994));
#34123=CARTESIAN_POINT('Ctrl Pts',(1.47018674401621E-11,-122.470483118095,
8.16439679232146));
#34124=CARTESIAN_POINT('Ctrl Pts',(4.71371668583241,-122.295483118095,8.16439679231297));
#34125=CARTESIAN_POINT('Ctrl Pts',(7.07057502873392,-122.120483118095,4.082198396148));
#34126=CARTESIAN_POINT('Ctrl Pts',(9.42743337163542,-121.945483118095,-1.69756769845304E-11));
#34127=CARTESIAN_POINT('Ctrl Pts',(7.07057502871922,-121.770483118095,-4.08219839617346));
#34128=CARTESIAN_POINT('Ctrl Pts',(4.71371668580301,-121.595483118095,-8.16439679232994));
#34129=CARTESIAN_POINT('Ctrl Pts',(-1.4702867290402E-11,-121.420483118095,
-8.16439679232146));
#34130=CARTESIAN_POINT('Ctrl Pts',(-4.71371668583241,-121.245483118095,
-8.16439679231297));
#34131=CARTESIAN_POINT('Ctrl Pts',(-7.07057502873392,-121.070483118095,
-4.082198396148));
#34132=CARTESIAN_POINT('Ctrl Pts',(-9.42743337163542,-120.895483118095,
1.69768315121407E-11));
#34133=CARTESIAN_POINT('Ctrl Pts',(-7.07057502871922,-120.720483118095,
4.08219839617346));
#34134=CARTESIAN_POINT('Ctrl Pts',(-4.71371668580301,-120.545483118095,
8.16439679232994));
#34135=CARTESIAN_POINT('Ctrl Pts',(1.47018674401621E-11,-120.370483118095,
8.16439679232146));
#34136=CARTESIAN_POINT('Ctrl Pts',(4.71371668583241,-120.195483118095,8.16439679231297));
#34137=CARTESIAN_POINT('Ctrl Pts',(7.07057502873392,-120.020483118095,4.082198396148));
#34138=CARTESIAN_POINT('Ctrl Pts',(9.42743337163542,-119.845483118095,-1.69756769845304E-11));
#34139=CARTESIAN_POINT('Ctrl Pts',(7.07057502871922,-119.670483118095,-4.08219839617346));
#34140=CARTESIAN_POINT('Ctrl Pts',(4.71371668580301,-119.495483118095,-8.16439679232994));
#34141=CARTESIAN_POINT('Ctrl Pts',(-1.4702867290402E-11,-119.320483118095,
-8.16439679232146));
#34142=CARTESIAN_POINT('Ctrl Pts',(-4.71371668583241,-119.145483118095,
-8.16439679231297));
#34143=CARTESIAN_POINT('Ctrl Pts',(-7.07057502873392,-118.970483118095,
-4.082198396148));
#34144=CARTESIAN_POINT('Ctrl Pts',(-9.42743337163542,-118.795483118095,
1.69768315121407E-11));
#34145=CARTESIAN_POINT('Ctrl Pts',(-7.07057502871922,-118.620483118095,
4.08219839617346));
#34146=CARTESIAN_POINT('Ctrl Pts',(-4.71371668580301,-118.445483118095,
8.16439679232994));
#34147=CARTESIAN_POINT('Ctrl Pts',(1.47018674401621E-11,-118.270483118095,
8.16439679232146));
#34148=CARTESIAN_POINT('Ctrl Pts',(4.71371668583241,-118.095483118095,8.16439679231297));
#34149=CARTESIAN_POINT('Ctrl Pts',(7.07057502873392,-117.920483118095,4.082198396148));
#34150=CARTESIAN_POINT('Ctrl Pts',(9.42743337163542,-117.745483118095,-1.69756769845304E-11));
#34151=CARTESIAN_POINT('Ctrl Pts',(7.07057502871922,-117.570483118095,-4.08219839617346));
#34152=CARTESIAN_POINT('Ctrl Pts',(4.71371668580301,-117.395483118095,-8.16439679232994));
#34153=CARTESIAN_POINT('Ctrl Pts',(-1.4702867290402E-11,-117.220483118095,
-8.16439679232146));
#34154=CARTESIAN_POINT('Ctrl Pts',(-4.71371668583241,-117.045483118095,
-8.16439679231297));
#34155=CARTESIAN_POINT('Ctrl Pts',(-7.07057502873392,-116.870483118095,
-4.082198396148));
#34156=CARTESIAN_POINT('Ctrl Pts',(-9.42743337163542,-116.695483118095,
1.69768315121407E-11));
#34157=CARTESIAN_POINT('Ctrl Pts',(-7.07057502871922,-116.520483118095,
4.08219839617346));
#34158=CARTESIAN_POINT('Ctrl Pts',(-4.71371668580301,-116.345483118095,
8.16439679232994));
#34159=CARTESIAN_POINT('Ctrl Pts',(1.47018674401621E-11,-116.170483118095,
8.16439679232146));
#34160=CARTESIAN_POINT('Ctrl Pts',(4.71371668583241,-115.995483118095,8.16439679231297));
#34161=CARTESIAN_POINT('Ctrl Pts',(7.07057502873392,-115.820483118095,4.082198396148));
#34162=CARTESIAN_POINT('Ctrl Pts',(9.42743337163542,-115.645483118095,-1.69756769845304E-11));
#34163=CARTESIAN_POINT('Ctrl Pts',(7.07057502871922,-115.470483118095,-4.08219839617346));
#34164=CARTESIAN_POINT('Ctrl Pts',(4.71371668580301,-115.295483118095,-8.16439679232994));
#34165=CARTESIAN_POINT('Ctrl Pts',(-1.4702867290402E-11,-115.120483118095,
-8.16439679232146));
#34166=CARTESIAN_POINT('Ctrl Pts',(-4.71371668583241,-114.945483118095,
-8.16439679231297));
#34167=CARTESIAN_POINT('Ctrl Pts',(-7.07057502873392,-114.770483118095,
-4.082198396148));
#34168=CARTESIAN_POINT('Ctrl Pts',(-9.42743337163542,-114.595483118095,
1.69768315121407E-11));
#34169=CARTESIAN_POINT('Ctrl Pts',(-7.07057502871922,-114.420483118095,
4.08219839617346));
#34170=CARTESIAN_POINT('Ctrl Pts',(-4.71371668580301,-114.245483118095,
8.16439679232994));
#34171=CARTESIAN_POINT('Ctrl Pts',(1.47018674401621E-11,-114.070483118095,
8.16439679232146));
#34172=CARTESIAN_POINT('Ctrl Pts',(4.71371668583241,-113.895483118095,8.16439679231297));
#34173=CARTESIAN_POINT('Ctrl Pts',(7.07057502873392,-113.720483118095,4.082198396148));
#34174=CARTESIAN_POINT('Ctrl Pts',(9.42743337163542,-113.545483118095,-1.69756769845304E-11));
#34175=CARTESIAN_POINT('Ctrl Pts',(7.07057502871922,-113.370483118095,-4.08219839617346));
#34176=CARTESIAN_POINT('Ctrl Pts',(4.71371668580301,-113.195483118095,-8.16439679232994));
#34177=CARTESIAN_POINT('Ctrl Pts',(-1.4702867290402E-11,-113.020483118095,
-8.16439679232146));
#34178=CARTESIAN_POINT('Ctrl Pts',(-4.71371668583241,-112.845483118095,
-8.16439679231297));
#34179=CARTESIAN_POINT('Ctrl Pts',(-7.07057502873392,-112.670483118095,
-4.082198396148));
#34180=CARTESIAN_POINT('Ctrl Pts',(-9.42743337163542,-112.495483118095,
1.69768315121407E-11));
#34181=CARTESIAN_POINT('Ctrl Pts',(-7.07057502871922,-112.320483118095,
4.08219839617346));
#34182=CARTESIAN_POINT('Ctrl Pts',(-4.71371668580301,-112.145483118095,
8.16439679232994));
#34183=CARTESIAN_POINT('Ctrl Pts',(1.47018674401621E-11,-111.970483118095,
8.16439679232146));
#34184=CARTESIAN_POINT('Ctrl Pts',(4.71371668583241,-111.795483118095,8.16439679231297));
#34185=CARTESIAN_POINT('Ctrl Pts',(7.07057502873392,-111.620483118095,4.082198396148));
#34186=CARTESIAN_POINT('Ctrl Pts',(9.42743337163542,-111.445483118095,-1.69756769845304E-11));
#34187=CARTESIAN_POINT('Ctrl Pts',(7.07057502871922,-111.270483118095,-4.08219839617346));
#34188=CARTESIAN_POINT('Ctrl Pts',(4.71371668580301,-111.095483118095,-8.16439679232994));
#34189=CARTESIAN_POINT('Ctrl Pts',(-1.4702867290402E-11,-110.920483118095,
-8.16439679232146));
#34190=CARTESIAN_POINT('Ctrl Pts',(-4.71371668583241,-110.745483118095,
-8.16439679231297));
#34191=CARTESIAN_POINT('Ctrl Pts',(-7.07057502873392,-110.570483118095,
-4.082198396148));
#34192=CARTESIAN_POINT('Ctrl Pts',(-9.42743337163542,-110.395483118095,
1.69768315121407E-11));
#34193=CARTESIAN_POINT('Ctrl Pts',(-7.07057502871922,-110.220483118095,
4.08219839617346));
#34194=CARTESIAN_POINT('Ctrl Pts',(-4.71371668580301,-110.045483118095,
8.16439679232994));
#34195=CARTESIAN_POINT('Ctrl Pts',(1.47018674401621E-11,-109.870483118095,
8.16439679232146));
#34196=CARTESIAN_POINT('Ctrl Pts',(4.71371668583241,-109.695483118095,8.16439679231297));
#34197=CARTESIAN_POINT('Ctrl Pts',(7.07057502873392,-109.520483118095,4.082198396148));
#34198=CARTESIAN_POINT('Ctrl Pts',(9.42743337163542,-109.345483118095,-1.69756769845304E-11));
#34199=CARTESIAN_POINT('Ctrl Pts',(7.07057502871922,-109.170483118095,-4.08219839617346));
#34200=CARTESIAN_POINT('Ctrl Pts',(4.71371668580301,-108.995483118095,-8.16439679232994));
#34201=CARTESIAN_POINT('Ctrl Pts',(-1.4702867290402E-11,-108.820483118095,
-8.16439679232146));
#34202=CARTESIAN_POINT('Ctrl Pts',(-4.71371668583241,-108.645483118095,
-8.16439679231297));
#34203=CARTESIAN_POINT('Ctrl Pts',(-7.07057502873392,-108.470483118095,
-4.082198396148));
#34204=CARTESIAN_POINT('Ctrl Pts',(-9.42743337163542,-108.295483118095,
1.69768315121407E-11));
#34205=CARTESIAN_POINT('Ctrl Pts',(-7.07057502871922,-108.120483118095,
4.08219839617346));
#34206=CARTESIAN_POINT('Ctrl Pts',(-4.71371668580301,-107.945483118095,
8.16439679232994));
#34207=CARTESIAN_POINT('Ctrl Pts',(1.47018674401621E-11,-107.770483118095,
8.16439679232146));
#34208=CARTESIAN_POINT('Ctrl Pts',(4.71371668583241,-107.595483118095,8.16439679231297));
#34209=CARTESIAN_POINT('Ctrl Pts',(7.07057502873392,-107.420483118095,4.082198396148));
#34210=CARTESIAN_POINT('Ctrl Pts',(9.42743337163542,-107.245483118095,-1.69756769845304E-11));
#34211=CARTESIAN_POINT('Ctrl Pts',(7.07057502871922,-107.070483118095,-4.08219839617346));
#34212=CARTESIAN_POINT('Ctrl Pts',(4.71371668580301,-106.895483118095,-8.16439679232994));
#34213=CARTESIAN_POINT('Ctrl Pts',(-1.4702867290402E-11,-106.720483118095,
-8.16439679232146));
#34214=CARTESIAN_POINT('Ctrl Pts',(-4.71371668583241,-106.545483118095,
-8.16439679231297));
#34215=CARTESIAN_POINT('Ctrl Pts',(-7.07057502873392,-106.370483118095,
-4.082198396148));
#34216=CARTESIAN_POINT('Ctrl Pts',(-9.42743337163542,-106.195483118095,
1.69768315121407E-11));
#34217=CARTESIAN_POINT('Ctrl Pts',(-7.07057502871922,-106.020483118095,
4.08219839617346));
#34218=CARTESIAN_POINT('Ctrl Pts',(-4.71371668580301,-105.845483118095,
8.16439679232994));
#34219=CARTESIAN_POINT('Ctrl Pts',(1.47018674401621E-11,-105.670483118095,
8.16439679232146));
#34220=CARTESIAN_POINT('Ctrl Pts',(4.71371668583241,-105.495483118095,8.16439679231297));
#34221=CARTESIAN_POINT('Ctrl Pts',(7.07057502873392,-105.320483118095,4.082198396148));
#34222=CARTESIAN_POINT('Ctrl Pts',(9.42743337163542,-105.145483118095,-1.69756769845304E-11));
#34223=CARTESIAN_POINT('Ctrl Pts',(7.07057502871922,-104.970483118095,-4.08219839617346));
#34224=CARTESIAN_POINT('Ctrl Pts',(4.71371668580301,-104.795483118095,-8.16439679232994));
#34225=CARTESIAN_POINT('Ctrl Pts',(-1.4702867290402E-11,-104.620483118095,
-8.16439679232146));
#34226=CARTESIAN_POINT('Ctrl Pts',(-4.71371668583241,-104.445483118095,
-8.16439679231297));
#34227=CARTESIAN_POINT('Ctrl Pts',(-7.07057502873392,-104.270483118095,
-4.082198396148));
#34228=CARTESIAN_POINT('Ctrl Pts',(-9.42743337163542,-104.095483118095,
1.69768315121407E-11));
#34229=CARTESIAN_POINT('Ctrl Pts',(-7.07057502871922,-103.920483118095,
4.08219839617346));
#34230=CARTESIAN_POINT('Ctrl Pts',(-4.71371668580301,-103.745483118095,
8.16439679232994));
#34231=CARTESIAN_POINT('Ctrl Pts',(1.47018674401621E-11,-103.570483118095,
8.16439679232146));
#34232=CARTESIAN_POINT('Ctrl Pts',(4.71371668583241,-103.395483118095,8.16439679231297));
#34233=CARTESIAN_POINT('Ctrl Pts',(7.07057502873392,-103.220483118095,4.082198396148));
#34234=CARTESIAN_POINT('Ctrl Pts',(9.42743337163542,-103.045483118095,-1.69756769845304E-11));
#34235=CARTESIAN_POINT('Ctrl Pts',(7.07057502871922,-102.870483118095,-4.08219839617346));
#34236=CARTESIAN_POINT('Ctrl Pts',(4.71371668580301,-102.695483118095,-8.16439679232994));
#34237=CARTESIAN_POINT('Ctrl Pts',(-1.4702867290402E-11,-102.520483118095,
-8.16439679232146));
#34238=CARTESIAN_POINT('Ctrl Pts',(-4.71371668583241,-102.345483118095,
-8.16439679231297));
#34239=CARTESIAN_POINT('Ctrl Pts',(-7.07057502873392,-102.170483118095,
-4.082198396148));
#34240=CARTESIAN_POINT('Ctrl Pts',(-9.42743337163542,-101.995483118095,
1.69768315121407E-11));
#34241=CARTESIAN_POINT('Ctrl Pts',(-7.07057502871922,-101.820483118095,
4.08219839617346));
#34242=CARTESIAN_POINT('Ctrl Pts',(-4.71371668580301,-101.645483118095,
8.16439679232994));
#34243=CARTESIAN_POINT('Ctrl Pts',(1.47018674401621E-11,-101.470483118095,
8.16439679232146));
#34244=CARTESIAN_POINT('Ctrl Pts',(4.71371668583241,-101.295483118095,8.16439679231297));
#34245=CARTESIAN_POINT('Ctrl Pts',(7.07057502873392,-101.120483118095,4.082198396148));
#34246=CARTESIAN_POINT('Ctrl Pts',(9.42743337163542,-100.945483118095,-1.69756769845304E-11));
#34247=CARTESIAN_POINT('Ctrl Pts',(7.07057502871922,-100.770483118095,-4.08219839617346));
#34248=CARTESIAN_POINT('Ctrl Pts',(4.71371668580301,-100.595483118095,-8.16439679232994));
#34249=CARTESIAN_POINT('Ctrl Pts',(-1.4702867290402E-11,-100.420483118095,
-8.16439679232146));
#34250=CARTESIAN_POINT('Ctrl Pts',(-4.71371668583241,-100.245483118095,
-8.16439679231297));
#34251=CARTESIAN_POINT('Ctrl Pts',(-7.07057502873392,-100.070483118095,
-4.082198396148));
#34252=CARTESIAN_POINT('Ctrl Pts',(-9.42743337163542,-99.8954831180954,
1.69768315121407E-11));
#34253=CARTESIAN_POINT('Ctrl Pts',(-7.07057502871922,-99.7204831180953,
4.08219839617346));
#34254=CARTESIAN_POINT('Ctrl Pts',(-4.71371668580301,-99.5454831180953,
8.16439679232994));
#34255=CARTESIAN_POINT('Ctrl Pts',(1.47018674401621E-11,-99.3704831180953,
8.16439679232146));
#34256=CARTESIAN_POINT('Ctrl Pts',(4.71371668583241,-99.1954831180954,8.16439679231297));
#34257=CARTESIAN_POINT('Ctrl Pts',(7.07057502873392,-99.0204831180954,4.082198396148));
#34258=CARTESIAN_POINT('Ctrl Pts',(9.42743337163542,-98.8454831180953,-1.69756769845304E-11));
#34259=CARTESIAN_POINT('Ctrl Pts',(7.07057502871922,-98.6704831180953,-4.08219839617346));
#34260=CARTESIAN_POINT('Ctrl Pts',(4.71371668580301,-98.4954831180954,-8.16439679232994));
#34261=CARTESIAN_POINT('Ctrl Pts',(-1.4702867290402E-11,-98.3204831180954,
-8.16439679232146));
#34262=CARTESIAN_POINT('Ctrl Pts',(-4.71371668583241,-98.1454831180953,
-8.16439679231297));
#34263=CARTESIAN_POINT('Ctrl Pts',(-7.07057502873392,-97.9704831180953,
-4.082198396148));
#34264=CARTESIAN_POINT('Ctrl Pts',(-9.42743337163542,-97.7954831180953,
1.69768315121407E-11));
#34265=CARTESIAN_POINT('Ctrl Pts',(-7.07057502871922,-97.6204831180954,
4.08219839617346));
#34266=CARTESIAN_POINT('Ctrl Pts',(-4.71371668580301,-97.4454831180954,
8.16439679232994));
#34267=CARTESIAN_POINT('Ctrl Pts',(1.47018674401621E-11,-97.2704831180953,
8.16439679232146));
#34268=CARTESIAN_POINT('Ctrl Pts',(4.71371668583241,-97.0954831180953,8.16439679231297));
#34269=CARTESIAN_POINT('Ctrl Pts',(7.07057502873392,-96.9204831180953,4.082198396148));
#34270=CARTESIAN_POINT('Ctrl Pts',(9.42743337163542,-96.7454831180954,-1.69756769845304E-11));
#34271=CARTESIAN_POINT('Ctrl Pts',(7.07057502871922,-96.5704831180954,-4.08219839617346));
#34272=CARTESIAN_POINT('Ctrl Pts',(4.71371668580301,-96.3954831180953,-8.16439679232994));
#34273=CARTESIAN_POINT('Ctrl Pts',(-1.4702867290402E-11,-96.2204831180954,
-8.16439679232146));
#34274=CARTESIAN_POINT('Ctrl Pts',(-4.71371668583241,-96.0454831180953,
-8.16439679231297));
#34275=CARTESIAN_POINT('Ctrl Pts',(-7.07057502873392,-95.8704831180954,
-4.082198396148));
#34276=CARTESIAN_POINT('Ctrl Pts',(-9.42743337163542,-95.6954831180953,
1.69768315121407E-11));
#34277=CARTESIAN_POINT('Ctrl Pts',(-7.07057502871922,-95.5204831180954,
4.08219839617346));
#34278=CARTESIAN_POINT('Ctrl Pts',(-4.71371668580301,-95.3454831180954,
8.16439679232994));
#34279=CARTESIAN_POINT('Ctrl Pts',(1.47018674401621E-11,-95.1704831180953,
8.16439679232146));
#34280=CARTESIAN_POINT('Ctrl Pts',(4.71371668583241,-94.9954831180954,8.16439679231297));
#34281=CARTESIAN_POINT('Ctrl Pts',(7.07057502873392,-94.8204831180954,4.082198396148));
#34282=CARTESIAN_POINT('Ctrl Pts',(9.42743337163542,-94.6454831180954,-1.69756769845304E-11));
#34283=CARTESIAN_POINT('Ctrl Pts',(7.07057502871922,-94.4704831180954,-4.08219839617346));
#34284=CARTESIAN_POINT('Ctrl Pts',(4.71371668580301,-94.2954831180953,-8.16439679232994));
#34285=CARTESIAN_POINT('Ctrl Pts',(-1.4702867290402E-11,-94.1204831180953,
-8.16439679232146));
#34286=CARTESIAN_POINT('Ctrl Pts',(-4.71371668583241,-93.9454831180954,
-8.16439679231297));
#34287=CARTESIAN_POINT('Ctrl Pts',(-7.07057502873392,-93.7704831180953,
-4.082198396148));
#34288=CARTESIAN_POINT('Ctrl Pts',(-9.42743337163542,-93.5954831180953,
1.69768315121407E-11));
#34289=CARTESIAN_POINT('Ctrl Pts',(-7.07057502871922,-93.4204831180954,
4.08219839617346));
#34290=CARTESIAN_POINT('Ctrl Pts',(-4.71371668580301,-93.2454831180954,
8.16439679232994));
#34291=CARTESIAN_POINT('Ctrl Pts',(1.47018674401621E-11,-93.0704831180954,
8.16439679232146));
#34292=CARTESIAN_POINT('Ctrl Pts',(4.71371668583241,-92.8954831180954,8.16439679231297));
#34293=CARTESIAN_POINT('Ctrl Pts',(7.07057502873392,-92.7204831180954,4.082198396148));
#34294=CARTESIAN_POINT('Ctrl Pts',(9.42743337163542,-92.5454831180953,-1.69756769845304E-11));
#34295=CARTESIAN_POINT('Ctrl Pts',(7.07057502871922,-92.3704831180954,-4.08219839617346));
#34296=CARTESIAN_POINT('Ctrl Pts',(4.71371668580301,-92.1954831180954,-8.16439679232994));
#34297=CARTESIAN_POINT('Ctrl Pts',(-1.4702867290402E-11,-92.0204831180953,
-8.16439679232146));
#34298=CARTESIAN_POINT('Ctrl Pts',(-4.71371668583241,-91.8454831180954,
-8.16439679231297));
#34299=CARTESIAN_POINT('Ctrl Pts',(-7.07057502873392,-91.6704831180954,
-4.082198396148));
#34300=CARTESIAN_POINT('Ctrl Pts',(-9.42743337163542,-91.4954831180954,
1.69768315121407E-11));
#34301=CARTESIAN_POINT('Ctrl Pts',(-7.07057502871922,-91.3204831180953,
4.08219839617346));
#34302=CARTESIAN_POINT('Ctrl Pts',(-4.71371668580301,-91.1454831180954,
8.16439679232994));
#34303=CARTESIAN_POINT('Ctrl Pts',(1.47018674401621E-11,-90.9704831180954,
8.16439679232146));
#34304=CARTESIAN_POINT('Ctrl Pts',(4.71371668583241,-90.7954831180953,8.16439679231297));
#34305=CARTESIAN_POINT('Ctrl Pts',(7.07057502873392,-90.6204831180954,4.082198396148));
#34306=CARTESIAN_POINT('Ctrl Pts',(9.42743337163542,-90.4454831180954,-1.69756769845304E-11));
#34307=CARTESIAN_POINT('Ctrl Pts',(7.07057502871922,-90.2704831180954,-4.08219839617346));
#34308=CARTESIAN_POINT('Ctrl Pts',(4.71371668580301,-90.0954831180954,-8.16439679232994));
#34309=CARTESIAN_POINT('Ctrl Pts',(-1.4702867290402E-11,-89.9204831180954,
-8.16439679232146));
#34310=CARTESIAN_POINT('Ctrl Pts',(-4.71371668583241,-89.7454831180954,
-8.16439679231297));
#34311=CARTESIAN_POINT('Ctrl Pts',(-7.07057502873392,-89.5704831180954,
-4.082198396148));
#34312=CARTESIAN_POINT('Ctrl Pts',(-9.42743337163542,-89.3954831180954,
1.69768315121407E-11));
#34313=CARTESIAN_POINT('Ctrl Pts',(-7.07057502871922,-89.2204831180953,
4.08219839617346));
#34314=CARTESIAN_POINT('Ctrl Pts',(-4.71371668580301,-89.0454831180954,
8.16439679232994));
#34315=CARTESIAN_POINT('Ctrl Pts',(1.47018674401621E-11,-88.8704831180954,
8.16439679232146));
#34316=CARTESIAN_POINT('Ctrl Pts',(4.71371668583241,-88.6954831180954,8.16439679231297));
#34317=CARTESIAN_POINT('Ctrl Pts',(7.07057502873392,-88.5204831180954,4.082198396148));
#34318=CARTESIAN_POINT('Ctrl Pts',(9.42743337163542,-88.3454831180954,-1.69756769845304E-11));
#34319=CARTESIAN_POINT('Ctrl Pts',(7.07057502871922,-88.1704831180954,-4.08219839617346));
#34320=CARTESIAN_POINT('Ctrl Pts',(4.71371668580301,-87.9954831180954,-8.16439679232994));
#34321=CARTESIAN_POINT('Ctrl Pts',(-1.4702867290402E-11,-87.8204831180954,
-8.16439679232146));
#34322=CARTESIAN_POINT('Ctrl Pts',(-4.71371668583241,-87.6454831180954,
-8.16439679231297));
#34323=CARTESIAN_POINT('Ctrl Pts',(-7.07057502873392,-87.4704831180954,
-4.082198396148));
#34324=CARTESIAN_POINT('Ctrl Pts',(-9.42743337163542,-87.2954831180954,
1.69768315121407E-11));
#34325=CARTESIAN_POINT('Ctrl Pts',(-7.07057502871922,-87.1204831180954,
4.08219839617346));
#34326=CARTESIAN_POINT('Ctrl Pts',(-4.71371668580301,-86.9454831180954,
8.16439679232994));
#34327=CARTESIAN_POINT('Ctrl Pts',(1.47018674401621E-11,-86.7704831180954,
8.16439679232146));
#34328=CARTESIAN_POINT('Ctrl Pts',(4.71371668583241,-86.5954831180954,8.16439679231297));
#34329=CARTESIAN_POINT('Ctrl Pts',(7.07057502873392,-86.4204831180953,4.082198396148));
#34330=CARTESIAN_POINT('Ctrl Pts',(9.42743337163542,-86.2454831180954,-1.69756769845304E-11));
#34331=CARTESIAN_POINT('Ctrl Pts',(7.07057502871922,-86.0704831180954,-4.08219839617346));
#34332=CARTESIAN_POINT('Ctrl Pts',(4.71371668580301,-85.8954831180954,-8.16439679232994));
#34333=CARTESIAN_POINT('Ctrl Pts',(-1.4702867290402E-11,-85.7204831180954,
-8.16439679232146));
#34334=CARTESIAN_POINT('Ctrl Pts',(-4.71371668583241,-85.5454831180954,
-8.16439679231297));
#34335=CARTESIAN_POINT('Ctrl Pts',(-7.07057502873392,-85.3704831180954,
-4.082198396148));
#34336=CARTESIAN_POINT('Ctrl Pts',(-9.42743337163542,-85.1954831180954,
1.69768315121407E-11));
#34337=CARTESIAN_POINT('Ctrl Pts',(-7.07057502871922,-85.0204831180954,
4.08219839617346));
#34338=CARTESIAN_POINT('Ctrl Pts',(-4.71371668580301,-84.8454831180954,
8.16439679232994));
#34339=CARTESIAN_POINT('Ctrl Pts',(1.47018674401621E-11,-84.6704831180954,
8.16439679232146));
#34340=CARTESIAN_POINT('Ctrl Pts',(4.71371668583241,-84.4954831180954,8.16439679231297));
#34341=CARTESIAN_POINT('Ctrl Pts',(7.07057502873392,-84.3204831180954,4.082198396148));
#34342=CARTESIAN_POINT('Ctrl Pts',(9.42743337163542,-84.1454831180954,-1.69756769845304E-11));
#34343=CARTESIAN_POINT('Ctrl Pts',(7.07057502871922,-83.9704831180954,-4.08219839617346));
#34344=CARTESIAN_POINT('Ctrl Pts',(4.71371668580301,-83.7954831180954,-8.16439679232994));
#34345=CARTESIAN_POINT('Ctrl Pts',(-1.4702867290402E-11,-83.6204831180954,
-8.16439679232146));
#34346=CARTESIAN_POINT('Ctrl Pts',(-4.71371668583241,-83.4454831180954,
-8.16439679231297));
#34347=CARTESIAN_POINT('Ctrl Pts',(-7.07057502873392,-83.2704831180954,
-4.082198396148));
#34348=CARTESIAN_POINT('Ctrl Pts',(-9.42743337163542,-83.0954831180954,
1.69768315121407E-11));
#34349=CARTESIAN_POINT('Ctrl Pts',(-7.07057502871922,-82.9204831180954,
4.08219839617346));
#34350=CARTESIAN_POINT('Ctrl Pts',(-4.71371668580301,-82.7454831180954,
8.16439679232994));
#34351=CARTESIAN_POINT('Ctrl Pts',(1.47018674401621E-11,-82.5704831180954,
8.16439679232146));
#34352=CARTESIAN_POINT('Ctrl Pts',(4.71371668583241,-82.3954831180954,8.16439679231297));
#34353=CARTESIAN_POINT('Ctrl Pts',(7.07057502873392,-82.2204831180954,4.082198396148));
#34354=CARTESIAN_POINT('Ctrl Pts',(9.42743337163542,-82.0454831180954,-1.69756769845304E-11));
#34355=CARTESIAN_POINT('Ctrl Pts',(7.07057502871922,-81.8704831180954,-4.08219839617346));
#34356=CARTESIAN_POINT('Ctrl Pts',(4.71371668580301,-81.6954831180954,-8.16439679232994));
#34357=CARTESIAN_POINT('Ctrl Pts',(-1.4702867290402E-11,-81.5204831180954,
-8.16439679232146));
#34358=CARTESIAN_POINT('Ctrl Pts',(-4.71371668583241,-81.3454831180954,
-8.16439679231297));
#34359=CARTESIAN_POINT('Ctrl Pts',(-7.07057502873392,-81.1704831180954,
-4.082198396148));
#34360=CARTESIAN_POINT('Ctrl Pts',(-9.42743337163542,-80.9954831180954,
1.69768315121407E-11));
#34361=CARTESIAN_POINT('Ctrl Pts',(-7.07057502871922,-80.8204831180954,
4.08219839617346));
#34362=CARTESIAN_POINT('Ctrl Pts',(-4.71371668580301,-80.6454831180954,
8.16439679232994));
#34363=CARTESIAN_POINT('Ctrl Pts',(1.47018674401621E-11,-80.4704831180954,
8.16439679232146));
#34364=CARTESIAN_POINT('Ctrl Pts',(4.71371668583241,-80.2954831180954,8.16439679231297));
#34365=CARTESIAN_POINT('Ctrl Pts',(7.07057502873392,-80.1204831180954,4.082198396148));
#34366=CARTESIAN_POINT('Ctrl Pts',(9.42743337163542,-79.9454831180954,-1.69756769845304E-11));
#34367=CARTESIAN_POINT('Ctrl Pts',(7.07057502871922,-79.7704831180954,-4.08219839617346));
#34368=CARTESIAN_POINT('Ctrl Pts',(4.71371668580301,-79.5954831180954,-8.16439679232994));
#34369=CARTESIAN_POINT('Ctrl Pts',(-1.4702867290402E-11,-79.4204831180954,
-8.16439679232146));
#34370=CARTESIAN_POINT('Ctrl Pts',(-4.71371668583241,-79.2454831180954,
-8.16439679231297));
#34371=CARTESIAN_POINT('Ctrl Pts',(-7.07057502873392,-79.0704831180954,
-4.082198396148));
#34372=CARTESIAN_POINT('Ctrl Pts',(-9.42743337163542,-78.8954831180954,
1.69768315121407E-11));
#34373=CARTESIAN_POINT('Ctrl Pts',(-7.07057502871922,-78.7204831180954,
4.08219839617346));
#34374=CARTESIAN_POINT('Ctrl Pts',(-4.71371668580301,-78.5454831180954,
8.16439679232994));
#34375=CARTESIAN_POINT('Ctrl Pts',(1.47018674401621E-11,-78.3704831180954,
8.16439679232146));
#34376=CARTESIAN_POINT('Ctrl Pts',(4.71371668583241,-78.1954831180954,8.16439679231297));
#34377=CARTESIAN_POINT('Ctrl Pts',(7.07057502873392,-78.0204831180954,4.082198396148));
#34378=CARTESIAN_POINT('Ctrl Pts',(9.42743337163542,-77.8454831180954,-1.69756769845304E-11));
#34379=CARTESIAN_POINT('Ctrl Pts',(7.07057502871922,-77.6704831180954,-4.08219839617346));
#34380=CARTESIAN_POINT('Ctrl Pts',(4.71371668580301,-77.4954831180954,-8.16439679232994));
#34381=CARTESIAN_POINT('Ctrl Pts',(-1.4702867290402E-11,-77.3204831180954,
-8.16439679232146));
#34382=CARTESIAN_POINT('Ctrl Pts',(-4.71371668583241,-77.1454831180954,
-8.16439679231297));
#34383=CARTESIAN_POINT('Ctrl Pts',(-7.07057502873392,-76.9704831180954,
-4.082198396148));
#34384=CARTESIAN_POINT('Ctrl Pts',(-9.42743337163542,-76.7954831180954,
1.69768315121407E-11));
#34385=CARTESIAN_POINT('Ctrl Pts',(-7.07057502871922,-76.6204831180954,
4.08219839617346));
#34386=CARTESIAN_POINT('Ctrl Pts',(-4.71371668580301,-76.4454831180954,
8.16439679232994));
#34387=CARTESIAN_POINT('Ctrl Pts',(1.47018674401621E-11,-76.2704831180954,
8.16439679232146));
#34388=CARTESIAN_POINT('Ctrl Pts',(4.71371668583241,-76.0954831180954,8.16439679231297));
#34389=CARTESIAN_POINT('Ctrl Pts',(7.07057502873392,-75.9204831180954,4.082198396148));
#34390=CARTESIAN_POINT('Ctrl Pts',(9.42743337163542,-75.7454831180954,-1.69756769845304E-11));
#34391=CARTESIAN_POINT('Ctrl Pts',(7.07057502871922,-75.5704831180954,-4.08219839617346));
#34392=CARTESIAN_POINT('Ctrl Pts',(4.71371668580301,-75.3954831180954,-8.16439679232994));
#34393=CARTESIAN_POINT('Ctrl Pts',(-1.4702867290402E-11,-75.2204831180954,
-8.16439679232146));
#34394=CARTESIAN_POINT('Ctrl Pts',(-4.71371668583241,-75.0454831180954,
-8.16439679231297));
#34395=CARTESIAN_POINT('Ctrl Pts',(-7.07057502873392,-74.8704831180954,
-4.082198396148));
#34396=CARTESIAN_POINT('Ctrl Pts',(-9.42743337163542,-74.6954831180954,
1.69768315121407E-11));
#34397=CARTESIAN_POINT('Ctrl Pts',(-7.07057502871922,-74.5204831180954,
4.08219839617346));
#34398=CARTESIAN_POINT('Ctrl Pts',(-4.71371668580301,-74.3454831180954,
8.16439679232994));
#34399=CARTESIAN_POINT('Ctrl Pts',(1.47018674401621E-11,-74.1704831180954,
8.16439679232146));
#34400=CARTESIAN_POINT('Ctrl Pts',(4.71371668583241,-73.9954831180954,8.16439679231297));
#34401=CARTESIAN_POINT('Ctrl Pts',(7.07057502873392,-73.8204831180954,4.082198396148));
#34402=CARTESIAN_POINT('Ctrl Pts',(9.42743337163542,-73.6454831180954,-1.69756769845304E-11));
#34403=CARTESIAN_POINT('Ctrl Pts',(7.07057502871922,-73.4704831180954,-4.08219839617346));
#34404=CARTESIAN_POINT('Ctrl Pts',(4.71371668580301,-73.2954831180954,-8.16439679232994));
#34405=CARTESIAN_POINT('Ctrl Pts',(-1.4702867290402E-11,-73.1204831180954,
-8.16439679232146));
#34406=CARTESIAN_POINT('Ctrl Pts',(-4.71371668583241,-72.9454831180954,
-8.16439679231297));
#34407=CARTESIAN_POINT('Ctrl Pts',(-7.07057502873392,-72.7704831180954,
-4.082198396148));
#34408=CARTESIAN_POINT('Ctrl Pts',(-9.42743337163542,-72.5954831180954,
1.69768315121407E-11));
#34409=CARTESIAN_POINT('Ctrl Pts',(-7.07057502871922,-72.4204831180954,
4.08219839617346));
#34410=CARTESIAN_POINT('Ctrl Pts',(-4.71371668580301,-72.2454831180954,
8.16439679232994));
#34411=CARTESIAN_POINT('Ctrl Pts',(1.47018674401621E-11,-72.0704831180954,
8.16439679232146));
#34412=CARTESIAN_POINT('Ctrl Pts',(4.71371668583241,-71.8954831180954,8.16439679231297));
#34413=CARTESIAN_POINT('Ctrl Pts',(7.07057502873392,-71.7204831180954,4.082198396148));
#34414=CARTESIAN_POINT('Ctrl Pts',(9.42743337163542,-71.5454831180954,-1.69756769845304E-11));
#34415=CARTESIAN_POINT('Ctrl Pts',(7.07057502871922,-71.3704831180954,-4.08219839617346));
#34416=CARTESIAN_POINT('Ctrl Pts',(4.71371668580301,-71.1954831180954,-8.16439679232994));
#34417=CARTESIAN_POINT('Ctrl Pts',(-1.4702867290402E-11,-71.0204831180954,
-8.16439679232146));
#34418=CARTESIAN_POINT('Ctrl Pts',(-4.71371668583241,-70.8454831180954,
-8.16439679231297));
#34419=CARTESIAN_POINT('Ctrl Pts',(-7.07057502873392,-70.6704831180954,
-4.082198396148));
#34420=CARTESIAN_POINT('Ctrl Pts',(-9.42743337163542,-70.4954831180954,
1.69768315121407E-11));
#34421=CARTESIAN_POINT('Ctrl Pts',(-7.07057502871922,-70.3204831180954,
4.08219839617346));
#34422=CARTESIAN_POINT('Ctrl Pts',(-4.71371668580301,-70.1454831180954,
8.16439679232994));
#34423=CARTESIAN_POINT('Ctrl Pts',(1.47018674401621E-11,-69.9704831180954,
8.16439679232146));
#34424=CARTESIAN_POINT('Ctrl Pts',(4.71371668583241,-69.7954831180954,8.16439679231297));
#34425=CARTESIAN_POINT('Ctrl Pts',(7.07057502873392,-69.6204831180954,4.082198396148));
#34426=CARTESIAN_POINT('Ctrl Pts',(9.42743337163542,-69.4454831180954,-1.69756769845304E-11));
#34427=CARTESIAN_POINT('Ctrl Pts',(7.07057502871922,-69.2704831180954,-4.08219839617346));
#34428=CARTESIAN_POINT('Ctrl Pts',(4.71371668580301,-69.0954831180954,-8.16439679232994));
#34429=CARTESIAN_POINT('Ctrl Pts',(-1.4702867290402E-11,-68.9204831180954,
-8.16439679232146));
#34430=CARTESIAN_POINT('Ctrl Pts',(-4.71371668583241,-68.7454831180954,
-8.16439679231297));
#34431=CARTESIAN_POINT('Ctrl Pts',(-7.07057502873392,-68.5704831180954,
-4.082198396148));
#34432=CARTESIAN_POINT('Ctrl Pts',(-9.42743337163542,-68.3954831180954,
1.69768315121407E-11));
#34433=CARTESIAN_POINT('Ctrl Pts',(-7.07057502871922,-68.2204831180954,
4.08219839617346));
#34434=CARTESIAN_POINT('Ctrl Pts',(-4.71371668580301,-68.0454831180954,
8.16439679232994));
#34435=CARTESIAN_POINT('Ctrl Pts',(1.47018674401621E-11,-67.8704831180954,
8.16439679232146));
#34436=CARTESIAN_POINT('Ctrl Pts',(4.71371668583241,-67.6954831180954,8.16439679231297));
#34437=CARTESIAN_POINT('Ctrl Pts',(7.07057502873392,-67.5204831180954,4.082198396148));
#34438=CARTESIAN_POINT('Ctrl Pts',(9.42743337163542,-67.3454831180954,-1.69756769845304E-11));
#34439=CARTESIAN_POINT('Ctrl Pts',(7.07057502871922,-67.1704831180954,-4.08219839617346));
#34440=CARTESIAN_POINT('Ctrl Pts',(4.71371668580301,-66.9954831180954,-8.16439679232994));
#34441=CARTESIAN_POINT('Ctrl Pts',(-1.4702867290402E-11,-66.8204831180954,
-8.16439679232146));
#34442=CARTESIAN_POINT('Ctrl Pts',(-4.71371668583241,-66.6454831180954,
-8.16439679231297));
#34443=CARTESIAN_POINT('Ctrl Pts',(-7.07057502873392,-66.4704831180954,
-4.082198396148));
#34444=CARTESIAN_POINT('Ctrl Pts',(-9.42743337163542,-66.2954831180954,
1.69768315121407E-11));
#34445=CARTESIAN_POINT('Ctrl Pts',(-7.07057502871922,-66.1204831180954,
4.08219839617346));
#34446=CARTESIAN_POINT('Ctrl Pts',(-4.71371668580301,-65.9454831180954,
8.16439679232994));
#34447=CARTESIAN_POINT('Ctrl Pts',(1.47018674401621E-11,-65.7704831180954,
8.16439679232146));
#34448=CARTESIAN_POINT('Ctrl Pts',(4.71371668583241,-65.5954831180954,8.16439679231297));
#34449=CARTESIAN_POINT('Ctrl Pts',(7.07057502873392,-65.4204831180954,4.082198396148));
#34450=CARTESIAN_POINT('Ctrl Pts',(9.42743337163542,-65.2454831180954,-1.69756769845304E-11));
#34451=CARTESIAN_POINT('Ctrl Pts',(7.07057502871922,-65.0704831180954,-4.08219839617346));
#34452=CARTESIAN_POINT('Ctrl Pts',(4.71371668580301,-64.8954831180954,-8.16439679232994));
#34453=CARTESIAN_POINT('Ctrl Pts',(-1.4702867290402E-11,-64.7204831180954,
-8.16439679232146));
#34454=CARTESIAN_POINT('Ctrl Pts',(-4.71371668583241,-64.5454831180954,
-8.16439679231297));
#34455=CARTESIAN_POINT('Ctrl Pts',(-7.07057502873392,-64.3704831180954,
-4.082198396148));
#34456=CARTESIAN_POINT('Ctrl Pts',(-9.42743337163542,-64.1954831180954,
1.69768315121407E-11));
#34457=CARTESIAN_POINT('Ctrl Pts',(-7.07057502871922,-64.0204831180954,
4.08219839617346));
#34458=CARTESIAN_POINT('Ctrl Pts',(-4.71371668580301,-63.8454831180954,
8.16439679232994));
#34459=CARTESIAN_POINT('Ctrl Pts',(1.47018674401621E-11,-63.6704831180954,
8.16439679232146));
#34460=CARTESIAN_POINT('Ctrl Pts',(4.71371668583241,-63.4954831180954,8.16439679231297));
#34461=CARTESIAN_POINT('Ctrl Pts',(7.07057502873392,-63.3204831180954,4.082198396148));
#34462=CARTESIAN_POINT('Ctrl Pts',(9.42743337163542,-63.1454831180954,-1.69756769845304E-11));
#34463=CARTESIAN_POINT('Ctrl Pts',(7.07057502871922,-62.9704831180954,-4.08219839617346));
#34464=CARTESIAN_POINT('Ctrl Pts',(4.71371668580301,-62.7954831180954,-8.16439679232994));
#34465=CARTESIAN_POINT('Ctrl Pts',(-1.4702867290402E-11,-62.6204831180954,
-8.16439679232146));
#34466=CARTESIAN_POINT('Ctrl Pts',(-4.71371668583241,-62.4454831180954,
-8.16439679231297));
#34467=CARTESIAN_POINT('Ctrl Pts',(-7.07057502873392,-62.2704831180954,
-4.082198396148));
#34468=CARTESIAN_POINT('Ctrl Pts',(-9.42743337163542,-62.0954831180954,
1.69768315121407E-11));
#34469=CARTESIAN_POINT('Ctrl Pts',(-7.07057502871922,-61.9204831180954,
4.08219839617346));
#34470=CARTESIAN_POINT('Ctrl Pts',(-4.71371668580301,-61.7454831180954,
8.16439679232994));
#34471=CARTESIAN_POINT('Ctrl Pts',(1.47018674401621E-11,-61.5704831180954,
8.16439679232146));
#34472=CARTESIAN_POINT('Ctrl Pts',(4.71371668583241,-61.3954831180954,8.16439679231297));
#34473=CARTESIAN_POINT('Ctrl Pts',(7.07057502873392,-61.2204831180954,4.082198396148));
#34474=CARTESIAN_POINT('Ctrl Pts',(9.42743337163542,-61.0454831180954,-1.69756769845304E-11));
#34475=CARTESIAN_POINT('Ctrl Pts',(7.07057502871922,-60.8704831180954,-4.08219839617346));
#34476=CARTESIAN_POINT('Ctrl Pts',(4.71371668580301,-60.6954831180954,-8.16439679232994));
#34477=CARTESIAN_POINT('Ctrl Pts',(-1.4702867290402E-11,-60.5204831180954,
-8.16439679232146));
#34478=CARTESIAN_POINT('Ctrl Pts',(-4.71371668583241,-60.3454831180954,
-8.16439679231297));
#34479=CARTESIAN_POINT('Ctrl Pts',(-7.07057502873392,-60.1704831180954,
-4.082198396148));
#34480=CARTESIAN_POINT('Ctrl Pts',(-9.42743337163542,-59.9954831180954,
1.69768315121407E-11));
#34481=CARTESIAN_POINT('Ctrl Pts',(-7.07057502871922,-59.8204831180954,
4.08219839617346));
#34482=CARTESIAN_POINT('Ctrl Pts',(-4.71371668580301,-59.6454831180954,
8.16439679232994));
#34483=CARTESIAN_POINT('Ctrl Pts',(1.47018674401621E-11,-59.4704831180955,
8.16439679232146));
#34484=CARTESIAN_POINT('Ctrl Pts',(4.71371668583241,-59.2954831180954,8.16439679231297));
#34485=CARTESIAN_POINT('Ctrl Pts',(7.07057502873392,-59.1204831180954,4.082198396148));
#34486=CARTESIAN_POINT('Ctrl Pts',(9.42743337163542,-58.9454831180954,-1.69756769845304E-11));
#34487=CARTESIAN_POINT('Ctrl Pts',(7.07057502871922,-58.7704831180954,-4.08219839617346));
#34488=CARTESIAN_POINT('Ctrl Pts',(4.71371668580301,-58.5954831180954,-8.16439679232994));
#34489=CARTESIAN_POINT('Ctrl Pts',(-1.4702867290402E-11,-58.4204831180954,
-8.16439679232146));
#34490=CARTESIAN_POINT('Ctrl Pts',(-4.71371668583241,-58.2454831180954,
-8.16439679231297));
#34491=CARTESIAN_POINT('Ctrl Pts',(-7.07057502873392,-58.0704831180954,
-4.082198396148));
#34492=CARTESIAN_POINT('Ctrl Pts',(-9.42743337163542,-57.8954831180954,
1.69768315121407E-11));
#34493=CARTESIAN_POINT('Ctrl Pts',(-7.07057502871922,-57.7204831180954,
4.08219839617346));
#34494=CARTESIAN_POINT('Ctrl Pts',(-4.71371668580301,-57.5454831180954,
8.16439679232994));
#34495=CARTESIAN_POINT('Ctrl Pts',(1.47018674401621E-11,-57.3704831180954,
8.16439679232146));
#34496=CARTESIAN_POINT('Ctrl Pts',(4.71371668583241,-57.1954831180954,8.16439679231297));
#34497=CARTESIAN_POINT('Ctrl Pts',(7.07057502873392,-57.0204831180954,4.082198396148));
#34498=CARTESIAN_POINT('Ctrl Pts',(9.42743337163542,-56.8454831180954,-1.69756769845304E-11));
#34499=CARTESIAN_POINT('Ctrl Pts',(7.07057502871922,-56.6704831180954,-4.08219839617346));
#34500=CARTESIAN_POINT('Ctrl Pts',(4.71371668580301,-56.4954831180954,-8.16439679232994));
#34501=CARTESIAN_POINT('Ctrl Pts',(-1.4702867290402E-11,-56.3204831180954,
-8.16439679232146));
#34502=CARTESIAN_POINT('Ctrl Pts',(-4.71371668583241,-56.1454831180954,
-8.16439679231297));
#34503=CARTESIAN_POINT('Ctrl Pts',(-7.07057502873392,-55.9704831180955,
-4.082198396148));
#34504=CARTESIAN_POINT('Ctrl Pts',(-9.42743337163542,-55.7954831180954,
1.69768315121407E-11));
#34505=CARTESIAN_POINT('Ctrl Pts',(-7.07057502871922,-55.6204831180954,
4.08219839617346));
#34506=CARTESIAN_POINT('Ctrl Pts',(-4.71371668580301,-55.4454831180954,
8.16439679232994));
#34507=CARTESIAN_POINT('Ctrl Pts',(1.47018674401621E-11,-55.2704831180954,
8.16439679232146));
#34508=CARTESIAN_POINT('Ctrl Pts',(4.71371668583241,-55.0954831180955,8.16439679231297));
#34509=CARTESIAN_POINT('Ctrl Pts',(7.07057502873392,-54.9204831180954,4.082198396148));
#34510=CARTESIAN_POINT('Ctrl Pts',(9.42743337163542,-54.7454831180954,-1.69756769845304E-11));
#34511=CARTESIAN_POINT('Ctrl Pts',(7.07057502871922,-54.5704831180954,-4.08219839617346));
#34512=CARTESIAN_POINT('Ctrl Pts',(4.71371668580301,-54.3954831180955,-8.16439679232994));
#34513=CARTESIAN_POINT('Ctrl Pts',(-1.4702867290402E-11,-54.2204831180954,
-8.16439679232146));
#34514=CARTESIAN_POINT('Ctrl Pts',(-4.71371668583241,-54.0454831180954,
-8.16439679231297));
#34515=CARTESIAN_POINT('Ctrl Pts',(-7.07057502873392,-53.8704831180954,
-4.082198396148));
#34516=CARTESIAN_POINT('Ctrl Pts',(-9.42743337163542,-53.6954831180954,
1.69768315121407E-11));
#34517=CARTESIAN_POINT('Ctrl Pts',(-7.07057502871922,-53.5204831180954,
4.08219839617346));
#34518=CARTESIAN_POINT('Ctrl Pts',(-4.71371668580301,-53.3454831180955,
8.16439679232994));
#34519=CARTESIAN_POINT('Ctrl Pts',(1.47018674401621E-11,-53.1704831180954,
8.16439679232146));
#34520=CARTESIAN_POINT('Ctrl Pts',(4.71371668583241,-52.9954831180954,8.16439679231297));
#34521=CARTESIAN_POINT('Ctrl Pts',(7.07057502873392,-52.8204831180955,4.082198396148));
#34522=CARTESIAN_POINT('Ctrl Pts',(9.42743337163542,-52.6454831180954,-1.69756769845304E-11));
#34523=CARTESIAN_POINT('Ctrl Pts',(7.07057502871922,-52.4704831180954,-4.08219839617346));
#34524=CARTESIAN_POINT('Ctrl Pts',(4.71371668580301,-52.2954831180954,-8.16439679232994));
#34525=CARTESIAN_POINT('Ctrl Pts',(-1.4702867290402E-11,-52.1204831180955,
-8.16439679232146));
#34526=CARTESIAN_POINT('Ctrl Pts',(-4.71371668583241,-51.9454831180954,
-8.16439679231297));
#34527=CARTESIAN_POINT('Ctrl Pts',(-7.07057502873392,-51.7704831180955,
-4.082198396148));
#34528=CARTESIAN_POINT('Ctrl Pts',(-9.42743337163542,-51.5954831180955,
1.69768315121407E-11));
#34529=CARTESIAN_POINT('Ctrl Pts',(-7.07057502871922,-51.4204831180954,
4.08219839617346));
#34530=CARTESIAN_POINT('Ctrl Pts',(-4.71371668580301,-51.2454831180955,
8.16439679232994));
#34531=CARTESIAN_POINT('Ctrl Pts',(1.47018674401621E-11,-51.0704831180955,
8.16439679232146));
#34532=CARTESIAN_POINT('Ctrl Pts',(4.71371668583241,-50.8954831180954,8.16439679231297));
#34533=CARTESIAN_POINT('Ctrl Pts',(7.07057502873392,-50.7204831180955,4.082198396148));
#34534=CARTESIAN_POINT('Ctrl Pts',(9.42743337163542,-50.5454831180955,-1.69756769845304E-11));
#34535=CARTESIAN_POINT('Ctrl Pts',(7.07057502871922,-50.3704831180955,-4.08219839617346));
#34536=CARTESIAN_POINT('Ctrl Pts',(4.71371668580301,-50.1954831180954,-8.16439679232994));
#34537=CARTESIAN_POINT('Ctrl Pts',(-1.4702867290402E-11,-50.0204831180955,
-8.16439679232146));
#34538=CARTESIAN_POINT('Ctrl Pts',(-4.71371668583241,-49.8454831180955,
-8.16439679231297));
#34539=CARTESIAN_POINT('Ctrl Pts',(-7.07057502873392,-49.6704831180954,
-4.082198396148));
#34540=CARTESIAN_POINT('Ctrl Pts',(-9.42743337163542,-49.4954831180955,
1.69768315121407E-11));
#34541=CARTESIAN_POINT('Ctrl Pts',(-7.07057502871922,-49.3204831180955,
4.08219839617346));
#34542=CARTESIAN_POINT('Ctrl Pts',(-4.71371668580301,-49.1454831180954,
8.16439679232994));
#34543=CARTESIAN_POINT('Ctrl Pts',(1.47018674401621E-11,-48.9704831180955,
8.16439679232146));
#34544=CARTESIAN_POINT('Ctrl Pts',(4.71371668583241,-48.7954831180955,8.16439679231297));
#34545=CARTESIAN_POINT('Ctrl Pts',(7.07057502873392,-48.6204831180954,4.082198396148));
#34546=CARTESIAN_POINT('Ctrl Pts',(9.42743337163542,-48.4454831180955,-1.69756769845304E-11));
#34547=CARTESIAN_POINT('Ctrl Pts',(7.07057502871922,-48.2704831180955,-4.08219839617346));
#34548=CARTESIAN_POINT('Ctrl Pts',(4.71371668580301,-48.0954831180954,-8.16439679232994));
#34549=CARTESIAN_POINT('Ctrl Pts',(-1.4702867290402E-11,-47.9204831180955,
-8.16439679232146));
#34550=CARTESIAN_POINT('Ctrl Pts',(-4.71371668583241,-47.7454831180955,
-8.16439679231297));
#34551=CARTESIAN_POINT('Ctrl Pts',(-7.07057502873392,-47.5704831180955,
-4.082198396148));
#34552=CARTESIAN_POINT('Ctrl Pts',(-9.42743337163542,-47.3954831180955,
1.69768315121407E-11));
#34553=CARTESIAN_POINT('Ctrl Pts',(-7.07057502871922,-47.2204831180955,
4.08219839617346));
#34554=CARTESIAN_POINT('Ctrl Pts',(-4.71371668580301,-47.0454831180955,
8.16439679232994));
#34555=CARTESIAN_POINT('Ctrl Pts',(1.47018674401621E-11,-46.8704831180955,
8.16439679232146));
#34556=CARTESIAN_POINT('Ctrl Pts',(4.71371668583241,-46.6954831180955,8.16439679231297));
#34557=CARTESIAN_POINT('Ctrl Pts',(7.07057502873392,-46.5204831180954,4.082198396148));
#34558=CARTESIAN_POINT('Ctrl Pts',(9.42743337163542,-46.3454831180955,-1.69756769845304E-11));
#34559=CARTESIAN_POINT('Ctrl Pts',(7.07057502871922,-46.1704831180955,-4.08219839617346));
#34560=CARTESIAN_POINT('Ctrl Pts',(4.71371668580301,-45.9954831180954,-8.16439679232994));
#34561=CARTESIAN_POINT('Ctrl Pts',(-1.4702867290402E-11,-45.8204831180955,
-8.16439679232146));
#34562=CARTESIAN_POINT('Ctrl Pts',(-4.71371668583241,-45.6454831180955,
-8.16439679231297));
#34563=CARTESIAN_POINT('Ctrl Pts',(-7.07057502873392,-45.4704831180955,
-4.082198396148));
#34564=CARTESIAN_POINT('Ctrl Pts',(-9.42743337163542,-45.2954831180954,
1.69768315121407E-11));
#34565=CARTESIAN_POINT('Ctrl Pts',(-7.07057502871922,-45.1204831180955,
4.08219839617346));
#34566=CARTESIAN_POINT('Ctrl Pts',(-4.71371668580301,-44.9454831180955,
8.16439679232994));
#34567=CARTESIAN_POINT('Ctrl Pts',(1.47018674401621E-11,-44.7704831180955,
8.16439679232146));
#34568=CARTESIAN_POINT('Ctrl Pts',(4.71371668583241,-44.5954831180955,8.16439679231297));
#34569=CARTESIAN_POINT('Ctrl Pts',(7.07057502873392,-44.4204831180955,4.082198396148));
#34570=CARTESIAN_POINT('Ctrl Pts',(9.42743337163542,-44.2454831180955,-1.69756769845304E-11));
#34571=CARTESIAN_POINT('Ctrl Pts',(7.07057502871922,-44.0704831180955,-4.08219839617346));
#34572=CARTESIAN_POINT('Ctrl Pts',(4.71371668580301,-43.8954831180955,-8.16439679232994));
#34573=CARTESIAN_POINT('Ctrl Pts',(-1.4702867290402E-11,-43.7204831180955,
-8.16439679232146));
#34574=CARTESIAN_POINT('Ctrl Pts',(-1.4702867290402E-11,-213.553019107145,
-8.16439679232146));
#34575=CARTESIAN_POINT('Ctrl Pts',(-4.71371668583241,-213.378019107145,
-8.16439679231297));
#34576=CARTESIAN_POINT('Ctrl Pts',(-7.07057502873392,-213.203019107145,
-4.082198396148));
#34577=CARTESIAN_POINT('Ctrl Pts',(-9.42743337163542,-213.028019107145,
1.69768315121407E-11));
#34578=CARTESIAN_POINT('Ctrl Pts',(-7.07057502871922,-212.853019107145,
4.08219839617346));
#34579=CARTESIAN_POINT('Ctrl Pts',(-4.71371668580301,-212.678019107145,
8.16439679232994));
#34580=CARTESIAN_POINT('Ctrl Pts',(1.47018674401621E-11,-212.503019107145,
8.16439679232146));
#34581=CARTESIAN_POINT('Ctrl Pts',(4.71371668583241,-212.328019107145,8.16439679231297));
#34582=CARTESIAN_POINT('Ctrl Pts',(7.07057502873392,-212.153019107145,4.082198396148));
#34583=CARTESIAN_POINT('Ctrl Pts',(9.42743337163542,-211.978019107145,-1.69756769845304E-11));
#34584=CARTESIAN_POINT('Ctrl Pts',(7.07057502871922,-211.803019107145,-4.08219839617346));
#34585=CARTESIAN_POINT('Ctrl Pts',(4.71371668580301,-211.628019107145,-8.16439679232994));
#34586=CARTESIAN_POINT('Ctrl Pts',(-1.4702867290402E-11,-211.453019107145,
-8.16439679232146));
#34587=CARTESIAN_POINT('Ctrl Pts',(-4.71371668583241,-211.278019107145,
-8.16439679231297));
#34588=CARTESIAN_POINT('Ctrl Pts',(-7.07057502873392,-211.103019107145,
-4.082198396148));
#34589=CARTESIAN_POINT('Ctrl Pts',(-9.42743337163542,-210.928019107145,
1.69768315121407E-11));
#34590=CARTESIAN_POINT('Ctrl Pts',(-7.07057502871922,-210.753019107145,
4.08219839617346));
#34591=CARTESIAN_POINT('Ctrl Pts',(-4.71371668580301,-210.578019107145,
8.16439679232994));
#34592=CARTESIAN_POINT('Ctrl Pts',(1.47018674401621E-11,-210.403019107145,
8.16439679232146));
#34593=CARTESIAN_POINT('Ctrl Pts',(4.71371668583241,-210.228019107145,8.16439679231297));
#34594=CARTESIAN_POINT('Ctrl Pts',(7.07057502873392,-210.053019107145,4.082198396148));
#34595=CARTESIAN_POINT('Ctrl Pts',(9.42743337163542,-209.878019107145,-1.69756769845304E-11));
#34596=CARTESIAN_POINT('Ctrl Pts',(7.07057502871922,-209.703019107145,-4.08219839617346));
#34597=CARTESIAN_POINT('Ctrl Pts',(4.71371668580301,-209.528019107145,-8.16439679232994));
#34598=CARTESIAN_POINT('Ctrl Pts',(-1.4702867290402E-11,-209.353019107145,
-8.16439679232146));
#34599=CARTESIAN_POINT('Ctrl Pts',(-4.71371668583241,-209.178019107145,
-8.16439679231297));
#34600=CARTESIAN_POINT('Ctrl Pts',(-7.07057502873392,-209.003019107145,
-4.082198396148));
#34601=CARTESIAN_POINT('Ctrl Pts',(-9.42743337163542,-208.828019107145,
1.69768315121407E-11));
#34602=CARTESIAN_POINT('Ctrl Pts',(-7.07057502871922,-208.653019107145,
4.08219839617346));
#34603=CARTESIAN_POINT('Ctrl Pts',(-4.71371668580301,-208.478019107145,
8.16439679232994));
#34604=CARTESIAN_POINT('Ctrl Pts',(1.47018674401621E-11,-208.303019107145,
8.16439679232146));
#34605=CARTESIAN_POINT('Ctrl Pts',(4.71371668583241,-208.128019107145,8.16439679231297));
#34606=CARTESIAN_POINT('Ctrl Pts',(7.07057502873392,-207.953019107145,4.082198396148));
#34607=CARTESIAN_POINT('Ctrl Pts',(9.42743337163542,-207.778019107145,-1.69756769845304E-11));
#34608=CARTESIAN_POINT('Ctrl Pts',(7.07057502871922,-207.603019107145,-4.08219839617346));
#34609=CARTESIAN_POINT('Ctrl Pts',(4.71371668580301,-207.428019107145,-8.16439679232994));
#34610=CARTESIAN_POINT('Ctrl Pts',(-1.4702867290402E-11,-207.253019107145,
-8.16439679232146));
#34611=CARTESIAN_POINT('Ctrl Pts',(-4.71371668583241,-207.078019107145,
-8.16439679231297));
#34612=CARTESIAN_POINT('Ctrl Pts',(-7.07057502873392,-206.903019107145,
-4.082198396148));
#34613=CARTESIAN_POINT('Ctrl Pts',(-9.42743337163542,-206.728019107145,
1.69768315121407E-11));
#34614=CARTESIAN_POINT('Ctrl Pts',(-7.07057502871922,-206.553019107145,
4.08219839617346));
#34615=CARTESIAN_POINT('Ctrl Pts',(-4.71371668580301,-206.378019107145,
8.16439679232994));
#34616=CARTESIAN_POINT('Ctrl Pts',(1.47018674401621E-11,-206.203019107145,
8.16439679232146));
#34617=CARTESIAN_POINT('Ctrl Pts',(4.71371668583241,-206.028019107145,8.16439679231297));
#34618=CARTESIAN_POINT('Ctrl Pts',(7.07057502873392,-205.853019107145,4.082198396148));
#34619=CARTESIAN_POINT('Ctrl Pts',(9.42743337163542,-205.678019107145,-1.69756769845304E-11));
#34620=CARTESIAN_POINT('Ctrl Pts',(7.07057502871922,-205.503019107145,-4.08219839617346));
#34621=CARTESIAN_POINT('Ctrl Pts',(4.71371668580301,-205.328019107145,-8.16439679232994));
#34622=CARTESIAN_POINT('Ctrl Pts',(-1.4702867290402E-11,-205.153019107145,
-8.16439679232146));
#34623=CARTESIAN_POINT('Ctrl Pts',(-4.71371668583241,-204.978019107145,
-8.16439679231297));
#34624=CARTESIAN_POINT('Ctrl Pts',(-7.07057502873392,-204.803019107145,
-4.082198396148));
#34625=CARTESIAN_POINT('Ctrl Pts',(-9.42743337163542,-204.628019107145,
1.69768315121407E-11));
#34626=CARTESIAN_POINT('Ctrl Pts',(-7.07057502871922,-204.453019107145,
4.08219839617346));
#34627=CARTESIAN_POINT('Ctrl Pts',(-4.71371668580301,-204.278019107145,
8.16439679232994));
#34628=CARTESIAN_POINT('Ctrl Pts',(1.47018674401621E-11,-204.103019107145,
8.16439679232146));
#34629=CARTESIAN_POINT('Ctrl Pts',(4.71371668583241,-203.928019107145,8.16439679231297));
#34630=CARTESIAN_POINT('Ctrl Pts',(7.07057502873392,-203.753019107145,4.082198396148));
#34631=CARTESIAN_POINT('Ctrl Pts',(9.42743337163542,-203.578019107145,-1.69756769845304E-11));
#34632=CARTESIAN_POINT('Ctrl Pts',(7.07057502871922,-203.403019107145,-4.08219839617346));
#34633=CARTESIAN_POINT('Ctrl Pts',(4.71371668580301,-203.228019107145,-8.16439679232994));
#34634=CARTESIAN_POINT('Ctrl Pts',(-1.4702867290402E-11,-203.053019107145,
-8.16439679232146));
#34635=CARTESIAN_POINT('Ctrl Pts',(-4.71371668583241,-202.878019107145,
-8.16439679231297));
#34636=CARTESIAN_POINT('Ctrl Pts',(-7.07057502873392,-202.703019107145,
-4.082198396148));
#34637=CARTESIAN_POINT('Ctrl Pts',(-9.42743337163542,-202.528019107145,
1.69768315121407E-11));
#34638=CARTESIAN_POINT('Ctrl Pts',(-7.07057502871922,-202.353019107145,
4.08219839617346));
#34639=CARTESIAN_POINT('Ctrl Pts',(-4.71371668580301,-202.178019107145,
8.16439679232994));
#34640=CARTESIAN_POINT('Ctrl Pts',(1.47018674401621E-11,-202.003019107145,
8.16439679232146));
#34641=CARTESIAN_POINT('Ctrl Pts',(4.71371668583241,-201.828019107145,8.16439679231297));
#34642=CARTESIAN_POINT('Ctrl Pts',(7.07057502873392,-201.653019107145,4.082198396148));
#34643=CARTESIAN_POINT('Ctrl Pts',(9.42743337163542,-201.478019107145,-1.69756769845304E-11));
#34644=CARTESIAN_POINT('Ctrl Pts',(7.07057502871922,-201.303019107145,-4.08219839617346));
#34645=CARTESIAN_POINT('Ctrl Pts',(4.71371668580301,-201.128019107145,-8.16439679232994));
#34646=CARTESIAN_POINT('Ctrl Pts',(-1.4702867290402E-11,-200.953019107145,
-8.16439679232146));
#34647=CARTESIAN_POINT('Ctrl Pts',(-4.71371668583241,-200.778019107145,
-8.16439679231297));
#34648=CARTESIAN_POINT('Ctrl Pts',(-7.07057502873392,-200.603019107145,
-4.082198396148));
#34649=CARTESIAN_POINT('Ctrl Pts',(-9.42743337163542,-200.428019107145,
1.69768315121407E-11));
#34650=CARTESIAN_POINT('Ctrl Pts',(-7.07057502871922,-200.253019107145,
4.08219839617346));
#34651=CARTESIAN_POINT('Ctrl Pts',(-4.71371668580301,-200.078019107145,
8.16439679232994));
#34652=CARTESIAN_POINT('Ctrl Pts',(1.47018674401621E-11,-199.903019107145,
8.16439679232146));
#34653=CARTESIAN_POINT('Ctrl Pts',(4.71371668583241,-199.728019107145,8.16439679231297));
#34654=CARTESIAN_POINT('Ctrl Pts',(7.07057502873392,-199.553019107145,4.082198396148));
#34655=CARTESIAN_POINT('Ctrl Pts',(9.42743337163542,-199.378019107145,-1.69756769845304E-11));
#34656=CARTESIAN_POINT('Ctrl Pts',(7.07057502871922,-199.203019107145,-4.08219839617346));
#34657=CARTESIAN_POINT('Ctrl Pts',(4.71371668580301,-199.028019107145,-8.16439679232994));
#34658=CARTESIAN_POINT('Ctrl Pts',(-1.4702867290402E-11,-198.853019107145,
-8.16439679232146));
#34659=CARTESIAN_POINT('Ctrl Pts',(-4.71371668583241,-198.678019107145,
-8.16439679231297));
#34660=CARTESIAN_POINT('Ctrl Pts',(-7.07057502873392,-198.503019107145,
-4.082198396148));
#34661=CARTESIAN_POINT('Ctrl Pts',(-9.42743337163542,-198.328019107145,
1.69768315121407E-11));
#34662=CARTESIAN_POINT('Ctrl Pts',(-7.07057502871922,-198.153019107145,
4.08219839617346));
#34663=CARTESIAN_POINT('Ctrl Pts',(-4.71371668580301,-197.978019107145,
8.16439679232994));
#34664=CARTESIAN_POINT('Ctrl Pts',(1.47018674401621E-11,-197.803019107145,
8.16439679232146));
#34665=CARTESIAN_POINT('Ctrl Pts',(4.71371668583241,-197.628019107145,8.16439679231297));
#34666=CARTESIAN_POINT('Ctrl Pts',(7.07057502873392,-197.453019107145,4.082198396148));
#34667=CARTESIAN_POINT('Ctrl Pts',(9.42743337163542,-197.278019107145,-1.69756769845304E-11));
#34668=CARTESIAN_POINT('Ctrl Pts',(7.07057502871922,-197.103019107145,-4.08219839617346));
#34669=CARTESIAN_POINT('Ctrl Pts',(4.71371668580301,-196.928019107145,-8.16439679232994));
#34670=CARTESIAN_POINT('Ctrl Pts',(-1.4702867290402E-11,-196.753019107145,
-8.16439679232146));
#34671=CARTESIAN_POINT('Ctrl Pts',(-4.71371668583241,-196.578019107145,
-8.16439679231297));
#34672=CARTESIAN_POINT('Ctrl Pts',(-7.07057502873392,-196.403019107145,
-4.082198396148));
#34673=CARTESIAN_POINT('Ctrl Pts',(-9.42743337163542,-196.228019107145,
1.69768315121407E-11));
#34674=CARTESIAN_POINT('Ctrl Pts',(-7.07057502871922,-196.053019107145,
4.08219839617346));
#34675=CARTESIAN_POINT('Ctrl Pts',(-4.71371668580301,-195.878019107145,
8.16439679232994));
#34676=CARTESIAN_POINT('Ctrl Pts',(1.47018674401621E-11,-195.703019107145,
8.16439679232146));
#34677=CARTESIAN_POINT('Ctrl Pts',(4.71371668583241,-195.528019107145,8.16439679231297));
#34678=CARTESIAN_POINT('Ctrl Pts',(7.07057502873392,-195.353019107145,4.082198396148));
#34679=CARTESIAN_POINT('Ctrl Pts',(9.42743337163542,-195.178019107145,-1.69756769845304E-11));
#34680=CARTESIAN_POINT('Ctrl Pts',(7.07057502871922,-195.003019107145,-4.08219839617346));
#34681=CARTESIAN_POINT('Ctrl Pts',(4.71371668580301,-194.828019107145,-8.16439679232994));
#34682=CARTESIAN_POINT('Ctrl Pts',(-1.4702867290402E-11,-194.653019107145,
-8.16439679232146));
#34683=CARTESIAN_POINT('Ctrl Pts',(-4.71371668583241,-194.478019107145,
-8.16439679231297));
#34684=CARTESIAN_POINT('Ctrl Pts',(-7.07057502873392,-194.303019107145,
-4.082198396148));
#34685=CARTESIAN_POINT('Ctrl Pts',(-9.42743337163542,-194.128019107145,
1.69768315121407E-11));
#34686=CARTESIAN_POINT('Ctrl Pts',(-7.07057502871922,-193.953019107145,
4.08219839617346));
#34687=CARTESIAN_POINT('Ctrl Pts',(-4.71371668580301,-193.778019107145,
8.16439679232994));
#34688=CARTESIAN_POINT('Ctrl Pts',(1.47018674401621E-11,-193.603019107145,
8.16439679232146));
#34689=CARTESIAN_POINT('Ctrl Pts',(4.71371668583241,-193.428019107145,8.16439679231297));
#34690=CARTESIAN_POINT('Ctrl Pts',(7.07057502873392,-193.253019107145,4.082198396148));
#34691=CARTESIAN_POINT('Ctrl Pts',(9.42743337163542,-193.078019107145,-1.69756769845304E-11));
#34692=CARTESIAN_POINT('Ctrl Pts',(7.07057502871922,-192.903019107145,-4.08219839617346));
#34693=CARTESIAN_POINT('Ctrl Pts',(4.71371668580301,-192.728019107145,-8.16439679232994));
#34694=CARTESIAN_POINT('Ctrl Pts',(-1.4702867290402E-11,-192.553019107145,
-8.16439679232146));
#34695=CARTESIAN_POINT('Ctrl Pts',(-4.71371668583241,-192.378019107145,
-8.16439679231297));
#34696=CARTESIAN_POINT('Ctrl Pts',(-7.07057502873392,-192.203019107145,
-4.082198396148));
#34697=CARTESIAN_POINT('Ctrl Pts',(-9.42743337163542,-192.028019107145,
1.69768315121407E-11));
#34698=CARTESIAN_POINT('Ctrl Pts',(-7.07057502871922,-191.853019107145,
4.08219839617346));
#34699=CARTESIAN_POINT('Ctrl Pts',(-4.71371668580301,-191.678019107145,
8.16439679232994));
#34700=CARTESIAN_POINT('Ctrl Pts',(1.47018674401621E-11,-191.503019107145,
8.16439679232146));
#34701=CARTESIAN_POINT('Ctrl Pts',(4.71371668583241,-191.328019107145,8.16439679231297));
#34702=CARTESIAN_POINT('Ctrl Pts',(7.07057502873392,-191.153019107145,4.082198396148));
#34703=CARTESIAN_POINT('Ctrl Pts',(9.42743337163542,-190.978019107145,-1.69756769845304E-11));
#34704=CARTESIAN_POINT('Ctrl Pts',(7.07057502871922,-190.803019107145,-4.08219839617346));
#34705=CARTESIAN_POINT('Ctrl Pts',(4.71371668580301,-190.628019107145,-8.16439679232994));
#34706=CARTESIAN_POINT('Ctrl Pts',(-1.4702867290402E-11,-190.453019107145,
-8.16439679232146));
#34707=CARTESIAN_POINT('Ctrl Pts',(-4.71371668583241,-190.278019107145,
-8.16439679231297));
#34708=CARTESIAN_POINT('Ctrl Pts',(-7.07057502873392,-190.103019107145,
-4.082198396148));
#34709=CARTESIAN_POINT('Ctrl Pts',(-9.42743337163542,-189.928019107145,
1.69768315121407E-11));
#34710=CARTESIAN_POINT('Ctrl Pts',(-7.07057502871922,-189.753019107145,
4.08219839617346));
#34711=CARTESIAN_POINT('Ctrl Pts',(-4.71371668580301,-189.578019107145,
8.16439679232994));
#34712=CARTESIAN_POINT('Ctrl Pts',(1.47018674401621E-11,-189.403019107145,
8.16439679232146));
#34713=CARTESIAN_POINT('Ctrl Pts',(4.71371668583241,-189.228019107145,8.16439679231297));
#34714=CARTESIAN_POINT('Ctrl Pts',(7.07057502873392,-189.053019107145,4.082198396148));
#34715=CARTESIAN_POINT('Ctrl Pts',(9.42743337163542,-188.878019107145,-1.69756769845304E-11));
#34716=CARTESIAN_POINT('Ctrl Pts',(7.07057502871922,-188.703019107145,-4.08219839617346));
#34717=CARTESIAN_POINT('Ctrl Pts',(4.71371668580301,-188.528019107145,-8.16439679232994));
#34718=CARTESIAN_POINT('Ctrl Pts',(-1.4702867290402E-11,-188.353019107145,
-8.16439679232146));
#34719=CARTESIAN_POINT('Ctrl Pts',(-4.71371668583241,-188.178019107145,
-8.16439679231297));
#34720=CARTESIAN_POINT('Ctrl Pts',(-7.07057502873392,-188.003019107145,
-4.082198396148));
#34721=CARTESIAN_POINT('Ctrl Pts',(-9.42743337163542,-187.828019107145,
1.69768315121407E-11));
#34722=CARTESIAN_POINT('Ctrl Pts',(-7.07057502871922,-187.653019107145,
4.08219839617346));
#34723=CARTESIAN_POINT('Ctrl Pts',(-4.71371668580301,-187.478019107145,
8.16439679232994));
#34724=CARTESIAN_POINT('Ctrl Pts',(1.47018674401621E-11,-187.303019107145,
8.16439679232146));
#34725=CARTESIAN_POINT('Ctrl Pts',(4.71371668583241,-187.128019107145,8.16439679231297));
#34726=CARTESIAN_POINT('Ctrl Pts',(7.07057502873392,-186.953019107145,4.082198396148));
#34727=CARTESIAN_POINT('Ctrl Pts',(9.42743337163542,-186.778019107145,-1.69756769845304E-11));
#34728=CARTESIAN_POINT('Ctrl Pts',(7.07057502871922,-186.603019107145,-4.08219839617346));
#34729=CARTESIAN_POINT('Ctrl Pts',(4.71371668580301,-186.428019107145,-8.16439679232994));
#34730=CARTESIAN_POINT('Ctrl Pts',(-1.4702867290402E-11,-186.253019107145,
-8.16439679232146));
#34731=CARTESIAN_POINT('Ctrl Pts',(-4.71371668583241,-186.078019107145,
-8.16439679231297));
#34732=CARTESIAN_POINT('Ctrl Pts',(-7.07057502873392,-185.903019107145,
-4.082198396148));
#34733=CARTESIAN_POINT('Ctrl Pts',(-9.42743337163542,-185.728019107145,
1.69768315121407E-11));
#34734=CARTESIAN_POINT('Ctrl Pts',(-7.07057502871922,-185.553019107145,
4.08219839617346));
#34735=CARTESIAN_POINT('Ctrl Pts',(-4.71371668580301,-185.378019107145,
8.16439679232994));
#34736=CARTESIAN_POINT('Ctrl Pts',(1.47018674401621E-11,-185.203019107145,
8.16439679232146));
#34737=CARTESIAN_POINT('Ctrl Pts',(4.71371668583241,-185.028019107145,8.16439679231297));
#34738=CARTESIAN_POINT('Ctrl Pts',(7.07057502873392,-184.853019107145,4.082198396148));
#34739=CARTESIAN_POINT('Ctrl Pts',(9.42743337163542,-184.678019107145,-1.69756769845304E-11));
#34740=CARTESIAN_POINT('Ctrl Pts',(7.07057502871922,-184.503019107145,-4.08219839617346));
#34741=CARTESIAN_POINT('Ctrl Pts',(4.71371668580301,-184.328019107145,-8.16439679232994));
#34742=CARTESIAN_POINT('Ctrl Pts',(-1.4702867290402E-11,-184.153019107145,
-8.16439679232146));
#34743=CARTESIAN_POINT('Ctrl Pts',(-4.71371668583241,-183.978019107145,
-8.16439679231297));
#34744=CARTESIAN_POINT('Ctrl Pts',(-7.07057502873392,-183.803019107145,
-4.082198396148));
#34745=CARTESIAN_POINT('Ctrl Pts',(-9.42743337163542,-183.628019107145,
1.69768315121407E-11));
#34746=CARTESIAN_POINT('Ctrl Pts',(-7.07057502871922,-183.453019107145,
4.08219839617346));
#34747=CARTESIAN_POINT('Ctrl Pts',(-4.71371668580301,-183.278019107145,
8.16439679232994));
#34748=CARTESIAN_POINT('Ctrl Pts',(1.47018674401621E-11,-183.103019107145,
8.16439679232146));
#34749=CARTESIAN_POINT('Ctrl Pts',(4.71371668583241,-182.928019107145,8.16439679231297));
#34750=CARTESIAN_POINT('Ctrl Pts',(7.07057502873392,-182.753019107145,4.082198396148));
#34751=CARTESIAN_POINT('Ctrl Pts',(9.42743337163542,-182.578019107145,-1.69756769845304E-11));
#34752=CARTESIAN_POINT('Ctrl Pts',(7.07057502871922,-182.403019107145,-4.08219839617346));
#34753=CARTESIAN_POINT('Ctrl Pts',(4.71371668580301,-182.228019107145,-8.16439679232994));
#34754=CARTESIAN_POINT('Ctrl Pts',(-1.4702867290402E-11,-182.053019107145,
-8.16439679232146));
#34755=CARTESIAN_POINT('Ctrl Pts',(-4.71371668583241,-181.878019107145,
-8.16439679231297));
#34756=CARTESIAN_POINT('Ctrl Pts',(-7.07057502873392,-181.703019107145,
-4.082198396148));
#34757=CARTESIAN_POINT('Ctrl Pts',(-9.42743337163542,-181.528019107145,
1.69768315121407E-11));
#34758=CARTESIAN_POINT('Ctrl Pts',(-7.07057502871922,-181.353019107145,
4.08219839617346));
#34759=CARTESIAN_POINT('Ctrl Pts',(-4.71371668580301,-181.178019107145,
8.16439679232994));
#34760=CARTESIAN_POINT('Ctrl Pts',(1.47018674401621E-11,-181.003019107145,
8.16439679232146));
#34761=CARTESIAN_POINT('Ctrl Pts',(4.71371668583241,-180.828019107145,8.16439679231297));
#34762=CARTESIAN_POINT('Ctrl Pts',(7.07057502873392,-180.653019107145,4.082198396148));
#34763=CARTESIAN_POINT('Ctrl Pts',(9.42743337163542,-180.478019107145,-1.69756769845304E-11));
#34764=CARTESIAN_POINT('Ctrl Pts',(7.07057502871922,-180.303019107145,-4.08219839617346));
#34765=CARTESIAN_POINT('Ctrl Pts',(4.71371668580301,-180.128019107145,-8.16439679232994));
#34766=CARTESIAN_POINT('Ctrl Pts',(-1.4702867290402E-11,-179.953019107145,
-8.16439679232146));
#34767=CARTESIAN_POINT('Ctrl Pts',(-4.71371668583241,-179.778019107145,
-8.16439679231297));
#34768=CARTESIAN_POINT('Ctrl Pts',(-7.07057502873392,-179.603019107145,
-4.082198396148));
#34769=CARTESIAN_POINT('Ctrl Pts',(-9.42743337163542,-179.428019107145,
1.69768315121407E-11));
#34770=CARTESIAN_POINT('Ctrl Pts',(-7.07057502871922,-179.253019107145,
4.08219839617346));
#34771=CARTESIAN_POINT('Ctrl Pts',(-4.71371668580301,-179.078019107145,
8.16439679232994));
#34772=CARTESIAN_POINT('Ctrl Pts',(1.47018674401621E-11,-178.903019107145,
8.16439679232146));
#34773=CARTESIAN_POINT('Ctrl Pts',(4.71371668583241,-178.728019107145,8.16439679231297));
#34774=CARTESIAN_POINT('Ctrl Pts',(7.07057502873392,-178.553019107145,4.082198396148));
#34775=CARTESIAN_POINT('Ctrl Pts',(9.42743337163542,-178.378019107145,-1.69756769845304E-11));
#34776=CARTESIAN_POINT('Ctrl Pts',(7.07057502871922,-178.203019107145,-4.08219839617346));
#34777=CARTESIAN_POINT('Ctrl Pts',(4.71371668580301,-178.028019107145,-8.16439679232994));
#34778=CARTESIAN_POINT('Ctrl Pts',(-1.4702867290402E-11,-177.853019107145,
-8.16439679232146));
#34779=CARTESIAN_POINT('Ctrl Pts',(-4.71371668583241,-177.678019107145,
-8.16439679231297));
#34780=CARTESIAN_POINT('Ctrl Pts',(-7.07057502873392,-177.503019107145,
-4.082198396148));
#34781=CARTESIAN_POINT('Ctrl Pts',(-9.42743337163542,-177.328019107145,
1.69768315121407E-11));
#34782=CARTESIAN_POINT('Ctrl Pts',(-7.07057502871922,-177.153019107145,
4.08219839617346));
#34783=CARTESIAN_POINT('Ctrl Pts',(-4.71371668580301,-176.978019107145,
8.16439679232994));
#34784=CARTESIAN_POINT('Ctrl Pts',(1.47018674401621E-11,-176.803019107145,
8.16439679232146));
#34785=CARTESIAN_POINT('Ctrl Pts',(4.71371668583241,-176.628019107145,8.16439679231297));
#34786=CARTESIAN_POINT('Ctrl Pts',(7.07057502873392,-176.453019107145,4.082198396148));
#34787=CARTESIAN_POINT('Ctrl Pts',(9.42743337163542,-176.278019107145,-1.69756769845304E-11));
#34788=CARTESIAN_POINT('Ctrl Pts',(7.07057502871922,-176.103019107145,-4.08219839617346));
#34789=CARTESIAN_POINT('Ctrl Pts',(4.71371668580301,-175.928019107145,-8.16439679232994));
#34790=CARTESIAN_POINT('Ctrl Pts',(-1.4702867290402E-11,-175.753019107145,
-8.16439679232146));
#34791=CARTESIAN_POINT('Ctrl Pts',(-4.71371668583241,-175.578019107145,
-8.16439679231297));
#34792=CARTESIAN_POINT('Ctrl Pts',(-7.07057502873392,-175.403019107145,
-4.082198396148));
#34793=CARTESIAN_POINT('Ctrl Pts',(-9.42743337163542,-175.228019107145,
1.69768315121407E-11));
#34794=CARTESIAN_POINT('Ctrl Pts',(-7.07057502871922,-175.053019107145,
4.08219839617346));
#34795=CARTESIAN_POINT('Ctrl Pts',(-4.71371668580301,-174.878019107145,
8.16439679232994));
#34796=CARTESIAN_POINT('Ctrl Pts',(1.47018674401621E-11,-174.703019107145,
8.16439679232146));
#34797=CARTESIAN_POINT('Ctrl Pts',(4.71371668583241,-174.528019107145,8.16439679231297));
#34798=CARTESIAN_POINT('Ctrl Pts',(7.07057502873392,-174.353019107145,4.082198396148));
#34799=CARTESIAN_POINT('Ctrl Pts',(9.42743337163542,-174.178019107145,-1.69756769845304E-11));
#34800=CARTESIAN_POINT('Ctrl Pts',(7.07057502871922,-174.003019107145,-4.08219839617346));
#34801=CARTESIAN_POINT('Ctrl Pts',(4.71371668580301,-173.828019107145,-8.16439679232994));
#34802=CARTESIAN_POINT('Ctrl Pts',(-1.4702867290402E-11,-173.653019107145,
-8.16439679232146));
#34803=CARTESIAN_POINT('Ctrl Pts',(-4.71371668583241,-173.478019107145,
-8.16439679231297));
#34804=CARTESIAN_POINT('Ctrl Pts',(-7.07057502873392,-173.303019107145,
-4.082198396148));
#34805=CARTESIAN_POINT('Ctrl Pts',(-9.42743337163542,-173.128019107145,
1.69768315121407E-11));
#34806=CARTESIAN_POINT('Ctrl Pts',(-7.07057502871922,-172.953019107145,
4.08219839617346));
#34807=CARTESIAN_POINT('Ctrl Pts',(-4.71371668580301,-172.778019107145,
8.16439679232994));
#34808=CARTESIAN_POINT('Ctrl Pts',(1.47018674401621E-11,-172.603019107145,
8.16439679232146));
#34809=CARTESIAN_POINT('Ctrl Pts',(4.71371668583241,-172.428019107145,8.16439679231297));
#34810=CARTESIAN_POINT('Ctrl Pts',(7.07057502873392,-172.253019107145,4.082198396148));
#34811=CARTESIAN_POINT('Ctrl Pts',(9.42743337163542,-172.078019107145,-1.69756769845304E-11));
#34812=CARTESIAN_POINT('Ctrl Pts',(7.07057502871922,-171.903019107145,-4.08219839617346));
#34813=CARTESIAN_POINT('Ctrl Pts',(4.71371668580301,-171.728019107145,-8.16439679232994));
#34814=CARTESIAN_POINT('Ctrl Pts',(-1.4702867290402E-11,-171.553019107145,
-8.16439679232146));
#34815=CARTESIAN_POINT('Ctrl Pts',(-4.71371668583241,-171.378019107145,
-8.16439679231297));
#34816=CARTESIAN_POINT('Ctrl Pts',(-7.07057502873392,-171.203019107145,
-4.082198396148));
#34817=CARTESIAN_POINT('Ctrl Pts',(-9.42743337163542,-171.028019107145,
1.69768315121407E-11));
#34818=CARTESIAN_POINT('Ctrl Pts',(-7.07057502871922,-170.853019107145,
4.08219839617346));
#34819=CARTESIAN_POINT('Ctrl Pts',(-4.71371668580301,-170.678019107145,
8.16439679232994));
#34820=CARTESIAN_POINT('Ctrl Pts',(1.47018674401621E-11,-170.503019107145,
8.16439679232146));
#34821=CARTESIAN_POINT('Ctrl Pts',(4.71371668583241,-170.328019107145,8.16439679231297));
#34822=CARTESIAN_POINT('Ctrl Pts',(7.07057502873392,-170.153019107145,4.082198396148));
#34823=CARTESIAN_POINT('Ctrl Pts',(9.42743337163542,-169.978019107145,-1.69756769845304E-11));
#34824=CARTESIAN_POINT('Ctrl Pts',(7.07057502871922,-169.803019107145,-4.08219839617346));
#34825=CARTESIAN_POINT('Ctrl Pts',(4.71371668580301,-169.628019107145,-8.16439679232994));
#34826=CARTESIAN_POINT('Ctrl Pts',(-1.4702867290402E-11,-169.453019107145,
-8.16439679232146));
#34827=CARTESIAN_POINT('Ctrl Pts',(-4.71371668583241,-169.278019107145,
-8.16439679231297));
#34828=CARTESIAN_POINT('Ctrl Pts',(-7.07057502873392,-169.103019107145,
-4.082198396148));
#34829=CARTESIAN_POINT('Ctrl Pts',(-9.42743337163542,-168.928019107145,
1.69768315121407E-11));
#34830=CARTESIAN_POINT('Ctrl Pts',(-7.07057502871922,-168.753019107145,
4.08219839617346));
#34831=CARTESIAN_POINT('Ctrl Pts',(-4.71371668580301,-168.578019107145,
8.16439679232994));
#34832=CARTESIAN_POINT('Ctrl Pts',(1.47018674401621E-11,-168.403019107145,
8.16439679232146));
#34833=CARTESIAN_POINT('Ctrl Pts',(4.71371668583241,-168.228019107145,8.16439679231297));
#34834=CARTESIAN_POINT('Ctrl Pts',(7.07057502873392,-168.053019107145,4.082198396148));
#34835=CARTESIAN_POINT('Ctrl Pts',(9.42743337163542,-167.878019107145,-1.69756769845304E-11));
#34836=CARTESIAN_POINT('Ctrl Pts',(7.07057502871922,-167.703019107145,-4.08219839617346));
#34837=CARTESIAN_POINT('Ctrl Pts',(4.71371668580301,-167.528019107145,-8.16439679232994));
#34838=CARTESIAN_POINT('Ctrl Pts',(-1.4702867290402E-11,-167.353019107145,
-8.16439679232146));
#34839=CARTESIAN_POINT('Ctrl Pts',(-4.71371668583241,-167.178019107145,
-8.16439679231297));
#34840=CARTESIAN_POINT('Ctrl Pts',(-7.07057502873392,-167.003019107145,
-4.082198396148));
#34841=CARTESIAN_POINT('Ctrl Pts',(-9.42743337163542,-166.828019107145,
1.69768315121407E-11));
#34842=CARTESIAN_POINT('Ctrl Pts',(-7.07057502871922,-166.653019107145,
4.08219839617346));
#34843=CARTESIAN_POINT('Ctrl Pts',(-4.71371668580301,-166.478019107145,
8.16439679232994));
#34844=CARTESIAN_POINT('Ctrl Pts',(1.47018674401621E-11,-166.303019107145,
8.16439679232146));
#34845=CARTESIAN_POINT('Ctrl Pts',(4.71371668583241,-166.128019107145,8.16439679231297));
#34846=CARTESIAN_POINT('Ctrl Pts',(7.07057502873392,-165.953019107145,4.082198396148));
#34847=CARTESIAN_POINT('Ctrl Pts',(9.42743337163542,-165.778019107145,-1.69756769845304E-11));
#34848=CARTESIAN_POINT('Ctrl Pts',(7.07057502871922,-165.603019107145,-4.08219839617346));
#34849=CARTESIAN_POINT('Ctrl Pts',(4.71371668580301,-165.428019107145,-8.16439679232994));
#34850=CARTESIAN_POINT('Ctrl Pts',(-1.4702867290402E-11,-165.253019107145,
-8.16439679232146));
#34851=CARTESIAN_POINT('Ctrl Pts',(-4.71371668583241,-165.078019107145,
-8.16439679231297));
#34852=CARTESIAN_POINT('Ctrl Pts',(-7.07057502873392,-164.903019107145,
-4.082198396148));
#34853=CARTESIAN_POINT('Ctrl Pts',(-9.42743337163542,-164.728019107145,
1.69768315121407E-11));
#34854=CARTESIAN_POINT('Ctrl Pts',(-7.07057502871922,-164.553019107145,
4.08219839617346));
#34855=CARTESIAN_POINT('Ctrl Pts',(-4.71371668580301,-164.378019107145,
8.16439679232994));
#34856=CARTESIAN_POINT('Ctrl Pts',(1.47018674401621E-11,-164.203019107145,
8.16439679232146));
#34857=CARTESIAN_POINT('Ctrl Pts',(4.71371668583241,-164.028019107145,8.16439679231297));
#34858=CARTESIAN_POINT('Ctrl Pts',(7.07057502873392,-163.853019107145,4.082198396148));
#34859=CARTESIAN_POINT('Ctrl Pts',(9.42743337163542,-163.678019107145,-1.69756769845304E-11));
#34860=CARTESIAN_POINT('Ctrl Pts',(7.07057502871922,-163.503019107145,-4.08219839617346));
#34861=CARTESIAN_POINT('Ctrl Pts',(4.71371668580301,-163.328019107145,-8.16439679232994));
#34862=CARTESIAN_POINT('Ctrl Pts',(-1.4702867290402E-11,-163.153019107145,
-8.16439679232146));
#34863=CARTESIAN_POINT('Ctrl Pts',(-4.71371668583241,-162.978019107145,
-8.16439679231297));
#34864=CARTESIAN_POINT('Ctrl Pts',(-7.07057502873392,-162.803019107145,
-4.082198396148));
#34865=CARTESIAN_POINT('Ctrl Pts',(-9.42743337163542,-162.628019107145,
1.69768315121407E-11));
#34866=CARTESIAN_POINT('Ctrl Pts',(-7.07057502871922,-162.453019107145,
4.08219839617346));
#34867=CARTESIAN_POINT('Ctrl Pts',(-4.71371668580301,-162.278019107145,
8.16439679232994));
#34868=CARTESIAN_POINT('Ctrl Pts',(1.47018674401621E-11,-162.103019107145,
8.16439679232146));
#34869=CARTESIAN_POINT('Ctrl Pts',(4.71371668583241,-161.928019107145,8.16439679231297));
#34870=CARTESIAN_POINT('Ctrl Pts',(7.07057502873392,-161.753019107145,4.082198396148));
#34871=CARTESIAN_POINT('Ctrl Pts',(9.42743337163542,-161.578019107145,-1.69756769845304E-11));
#34872=CARTESIAN_POINT('Ctrl Pts',(7.07057502871922,-161.403019107145,-4.08219839617346));
#34873=CARTESIAN_POINT('Ctrl Pts',(4.71371668580301,-161.228019107145,-8.16439679232994));
#34874=CARTESIAN_POINT('Ctrl Pts',(-1.4702867290402E-11,-161.053019107145,
-8.16439679232146));
#34875=CARTESIAN_POINT('Ctrl Pts',(-4.71371668583241,-160.878019107145,
-8.16439679231297));
#34876=CARTESIAN_POINT('Ctrl Pts',(-7.07057502873392,-160.703019107145,
-4.082198396148));
#34877=CARTESIAN_POINT('Ctrl Pts',(-9.42743337163542,-160.528019107145,
1.69768315121407E-11));
#34878=CARTESIAN_POINT('Ctrl Pts',(-7.07057502871922,-160.353019107145,
4.08219839617346));
#34879=CARTESIAN_POINT('Ctrl Pts',(-4.71371668580301,-160.178019107145,
8.16439679232994));
#34880=CARTESIAN_POINT('Ctrl Pts',(1.47018674401621E-11,-160.003019107145,
8.16439679232146));
#34881=CARTESIAN_POINT('Ctrl Pts',(4.71371668583241,-159.828019107145,8.16439679231297));
#34882=CARTESIAN_POINT('Ctrl Pts',(7.07057502873392,-159.653019107145,4.082198396148));
#34883=CARTESIAN_POINT('Ctrl Pts',(9.42743337163542,-159.478019107145,-1.69756769845304E-11));
#34884=CARTESIAN_POINT('Ctrl Pts',(7.07057502871922,-159.303019107145,-4.08219839617346));
#34885=CARTESIAN_POINT('Ctrl Pts',(4.71371668580301,-159.128019107145,-8.16439679232994));
#34886=CARTESIAN_POINT('Ctrl Pts',(-1.4702867290402E-11,-158.953019107145,
-8.16439679232146));
#34887=CARTESIAN_POINT('Ctrl Pts',(-4.71371668583241,-158.778019107145,
-8.16439679231297));
#34888=CARTESIAN_POINT('Ctrl Pts',(-7.07057502873392,-158.603019107145,
-4.082198396148));
#34889=CARTESIAN_POINT('Ctrl Pts',(-9.42743337163542,-158.428019107145,
1.69768315121407E-11));
#34890=CARTESIAN_POINT('Ctrl Pts',(-7.07057502871922,-158.253019107145,
4.08219839617346));
#34891=CARTESIAN_POINT('Ctrl Pts',(-4.71371668580301,-158.078019107145,
8.16439679232994));
#34892=CARTESIAN_POINT('Ctrl Pts',(1.47018674401621E-11,-157.903019107145,
8.16439679232146));
#34893=CARTESIAN_POINT('Ctrl Pts',(4.71371668583241,-157.728019107145,8.16439679231297));
#34894=CARTESIAN_POINT('Ctrl Pts',(7.07057502873392,-157.553019107145,4.082198396148));
#34895=CARTESIAN_POINT('Ctrl Pts',(9.42743337163542,-157.378019107145,-1.69756769845304E-11));
#34896=CARTESIAN_POINT('Ctrl Pts',(7.07057502871922,-157.203019107145,-4.08219839617346));
#34897=CARTESIAN_POINT('Ctrl Pts',(4.71371668580301,-157.028019107145,-8.16439679232994));
#34898=CARTESIAN_POINT('Ctrl Pts',(-1.4702867290402E-11,-156.853019107145,
-8.16439679232146));
#34899=CARTESIAN_POINT('Ctrl Pts',(-4.71371668583241,-156.678019107145,
-8.16439679231297));
#34900=CARTESIAN_POINT('Ctrl Pts',(-7.07057502873392,-156.503019107145,
-4.082198396148));
#34901=CARTESIAN_POINT('Ctrl Pts',(-9.42743337163542,-156.328019107145,
1.69768315121407E-11));
#34902=CARTESIAN_POINT('Ctrl Pts',(-7.07057502871922,-156.153019107145,
4.08219839617346));
#34903=CARTESIAN_POINT('Ctrl Pts',(-4.71371668580301,-155.978019107145,
8.16439679232994));
#34904=CARTESIAN_POINT('Ctrl Pts',(1.47018674401621E-11,-155.803019107145,
8.16439679232146));
#34905=CARTESIAN_POINT('Ctrl Pts',(4.71371668583241,-155.628019107145,8.16439679231297));
#34906=CARTESIAN_POINT('Ctrl Pts',(7.07057502873392,-155.453019107145,4.082198396148));
#34907=CARTESIAN_POINT('Ctrl Pts',(9.42743337163542,-155.278019107145,-1.69756769845304E-11));
#34908=CARTESIAN_POINT('Ctrl Pts',(7.07057502871922,-155.103019107145,-4.08219839617346));
#34909=CARTESIAN_POINT('Ctrl Pts',(4.71371668580301,-154.928019107145,-8.16439679232994));
#34910=CARTESIAN_POINT('Ctrl Pts',(-1.4702867290402E-11,-154.753019107145,
-8.16439679232146));
#34911=CARTESIAN_POINT('Ctrl Pts',(-4.71371668583241,-154.578019107145,
-8.16439679231297));
#34912=CARTESIAN_POINT('Ctrl Pts',(-7.07057502873392,-154.403019107145,
-4.082198396148));
#34913=CARTESIAN_POINT('Ctrl Pts',(-9.42743337163542,-154.228019107145,
1.69768315121407E-11));
#34914=CARTESIAN_POINT('Ctrl Pts',(-7.07057502871922,-154.053019107145,
4.08219839617346));
#34915=CARTESIAN_POINT('Ctrl Pts',(-4.71371668580301,-153.878019107145,
8.16439679232994));
#34916=CARTESIAN_POINT('Ctrl Pts',(1.47018674401621E-11,-153.703019107145,
8.16439679232146));
#34917=CARTESIAN_POINT('Ctrl Pts',(4.71371668583241,-153.528019107145,8.16439679231297));
#34918=CARTESIAN_POINT('Ctrl Pts',(7.07057502873392,-153.353019107145,4.082198396148));
#34919=CARTESIAN_POINT('Ctrl Pts',(9.42743337163542,-153.178019107145,-1.69756769845304E-11));
#34920=CARTESIAN_POINT('Ctrl Pts',(7.07057502871922,-153.003019107145,-4.08219839617346));
#34921=CARTESIAN_POINT('Ctrl Pts',(4.71371668580301,-152.828019107145,-8.16439679232994));
#34922=CARTESIAN_POINT('Ctrl Pts',(-1.4702867290402E-11,-152.653019107145,
-8.16439679232146));
#34923=CARTESIAN_POINT('Ctrl Pts',(-4.71371668583241,-152.478019107145,
-8.16439679231297));
#34924=CARTESIAN_POINT('Ctrl Pts',(-7.07057502873392,-152.303019107145,
-4.082198396148));
#34925=CARTESIAN_POINT('Ctrl Pts',(-9.42743337163542,-152.128019107145,
1.69768315121407E-11));
#34926=CARTESIAN_POINT('Ctrl Pts',(-7.07057502871922,-151.953019107145,
4.08219839617346));
#34927=CARTESIAN_POINT('Ctrl Pts',(-4.71371668580301,-151.778019107145,
8.16439679232994));
#34928=CARTESIAN_POINT('Ctrl Pts',(1.47018674401621E-11,-151.603019107145,
8.16439679232146));
#34929=CARTESIAN_POINT('Ctrl Pts',(4.71371668583241,-151.428019107145,8.16439679231297));
#34930=CARTESIAN_POINT('Ctrl Pts',(7.07057502873392,-151.253019107145,4.082198396148));
#34931=CARTESIAN_POINT('Ctrl Pts',(9.42743337163542,-151.078019107145,-1.69756769845304E-11));
#34932=CARTESIAN_POINT('Ctrl Pts',(7.07057502871922,-150.903019107145,-4.08219839617346));
#34933=CARTESIAN_POINT('Ctrl Pts',(4.71371668580301,-150.728019107145,-8.16439679232994));
#34934=CARTESIAN_POINT('Ctrl Pts',(-1.4702867290402E-11,-150.553019107145,
-8.16439679232146));
#34935=CARTESIAN_POINT('Ctrl Pts',(-4.71371668583241,-150.378019107145,
-8.16439679231297));
#34936=CARTESIAN_POINT('Ctrl Pts',(-7.07057502873392,-150.203019107145,
-4.082198396148));
#34937=CARTESIAN_POINT('Ctrl Pts',(-9.42743337163542,-150.028019107145,
1.69768315121407E-11));
#34938=CARTESIAN_POINT('Ctrl Pts',(-7.07057502871922,-149.853019107145,
4.08219839617346));
#34939=CARTESIAN_POINT('Ctrl Pts',(-4.71371668580301,-149.678019107145,
8.16439679232994));
#34940=CARTESIAN_POINT('Ctrl Pts',(1.47018674401621E-11,-149.503019107145,
8.16439679232146));
#34941=CARTESIAN_POINT('Ctrl Pts',(4.71371668583241,-149.328019107145,8.16439679231297));
#34942=CARTESIAN_POINT('Ctrl Pts',(7.07057502873392,-149.153019107145,4.082198396148));
#34943=CARTESIAN_POINT('Ctrl Pts',(9.42743337163542,-148.978019107145,-1.69756769845304E-11));
#34944=CARTESIAN_POINT('Ctrl Pts',(7.07057502871922,-148.803019107145,-4.08219839617346));
#34945=CARTESIAN_POINT('Ctrl Pts',(4.71371668580301,-148.628019107145,-8.16439679232994));
#34946=CARTESIAN_POINT('Ctrl Pts',(-1.4702867290402E-11,-148.453019107145,
-8.16439679232146));
#34947=CARTESIAN_POINT('Ctrl Pts',(-4.71371668583241,-148.278019107145,
-8.16439679231297));
#34948=CARTESIAN_POINT('Ctrl Pts',(-7.07057502873392,-148.103019107145,
-4.082198396148));
#34949=CARTESIAN_POINT('Ctrl Pts',(-9.42743337163542,-147.928019107145,
1.69768315121407E-11));
#34950=CARTESIAN_POINT('Ctrl Pts',(-7.07057502871922,-147.753019107145,
4.08219839617346));
#34951=CARTESIAN_POINT('Ctrl Pts',(-4.71371668580301,-147.578019107145,
8.16439679232994));
#34952=CARTESIAN_POINT('Ctrl Pts',(1.47018674401621E-11,-147.403019107145,
8.16439679232146));
#34953=CARTESIAN_POINT('Ctrl Pts',(4.71371668583241,-147.228019107145,8.16439679231297));
#34954=CARTESIAN_POINT('Ctrl Pts',(7.07057502873392,-147.053019107145,4.082198396148));
#34955=CARTESIAN_POINT('Ctrl Pts',(9.42743337163542,-146.878019107145,-1.69756769845304E-11));
#34956=CARTESIAN_POINT('Ctrl Pts',(7.07057502871922,-146.703019107145,-4.08219839617346));
#34957=CARTESIAN_POINT('Ctrl Pts',(4.71371668580301,-146.528019107145,-8.16439679232994));
#34958=CARTESIAN_POINT('Ctrl Pts',(-1.4702867290402E-11,-146.353019107145,
-8.16439679232146));
#34959=CARTESIAN_POINT('Ctrl Pts',(-4.71371668583241,-146.178019107145,
-8.16439679231297));
#34960=CARTESIAN_POINT('Ctrl Pts',(-7.07057502873392,-146.003019107145,
-4.082198396148));
#34961=CARTESIAN_POINT('Ctrl Pts',(-9.42743337163542,-145.828019107145,
1.69768315121407E-11));
#34962=CARTESIAN_POINT('Ctrl Pts',(-7.07057502871922,-145.653019107145,
4.08219839617346));
#34963=CARTESIAN_POINT('Ctrl Pts',(-4.71371668580301,-145.478019107145,
8.16439679232994));
#34964=CARTESIAN_POINT('Ctrl Pts',(1.47018674401621E-11,-145.303019107145,
8.16439679232146));
#34965=CARTESIAN_POINT('Ctrl Pts',(4.71371668583241,-145.128019107145,8.16439679231297));
#34966=CARTESIAN_POINT('Ctrl Pts',(7.07057502873392,-144.953019107145,4.082198396148));
#34967=CARTESIAN_POINT('Ctrl Pts',(9.42743337163542,-144.778019107145,-1.69756769845304E-11));
#34968=CARTESIAN_POINT('Ctrl Pts',(7.07057502871922,-144.603019107145,-4.08219839617346));
#34969=CARTESIAN_POINT('Ctrl Pts',(4.71371668580301,-144.428019107145,-8.16439679232994));
#34970=CARTESIAN_POINT('Ctrl Pts',(-1.4702867290402E-11,-144.253019107145,
-8.16439679232146));
#34971=CARTESIAN_POINT('Ctrl Pts',(-4.71371668583241,-144.078019107145,
-8.16439679231297));
#34972=CARTESIAN_POINT('Ctrl Pts',(-7.07057502873392,-143.903019107145,
-4.082198396148));
#34973=CARTESIAN_POINT('Ctrl Pts',(-9.42743337163542,-143.728019107145,
1.69768315121407E-11));
#34974=CARTESIAN_POINT('Ctrl Pts',(-7.07057502871922,-143.553019107145,
4.08219839617346));
#34975=CARTESIAN_POINT('Ctrl Pts',(-4.71371668580301,-143.378019107145,
8.16439679232994));
#34976=CARTESIAN_POINT('Ctrl Pts',(1.47018674401621E-11,-143.203019107145,
8.16439679232146));
#34977=CARTESIAN_POINT('Ctrl Pts',(4.71371668583241,-143.028019107145,8.16439679231297));
#34978=CARTESIAN_POINT('Ctrl Pts',(7.07057502873392,-142.853019107145,4.082198396148));
#34979=CARTESIAN_POINT('Ctrl Pts',(9.42743337163542,-142.678019107145,-1.69756769845304E-11));
#34980=CARTESIAN_POINT('Ctrl Pts',(7.07057502871922,-142.503019107145,-4.08219839617346));
#34981=CARTESIAN_POINT('Ctrl Pts',(4.71371668580301,-142.328019107145,-8.16439679232994));
#34982=CARTESIAN_POINT('Ctrl Pts',(-1.4702867290402E-11,-142.153019107145,
-8.16439679232146));
#34983=CARTESIAN_POINT('Ctrl Pts',(-4.71371668583241,-141.978019107145,
-8.16439679231297));
#34984=CARTESIAN_POINT('Ctrl Pts',(-7.07057502873392,-141.803019107145,
-4.082198396148));
#34985=CARTESIAN_POINT('Ctrl Pts',(-9.42743337163542,-141.628019107145,
1.69768315121407E-11));
#34986=CARTESIAN_POINT('Ctrl Pts',(-7.07057502871922,-141.453019107145,
4.08219839617346));
#34987=CARTESIAN_POINT('Ctrl Pts',(-4.71371668580301,-141.278019107145,
8.16439679232994));
#34988=CARTESIAN_POINT('Ctrl Pts',(1.47018674401621E-11,-141.103019107145,
8.16439679232146));
#34989=CARTESIAN_POINT('Ctrl Pts',(4.71371668583241,-140.928019107145,8.16439679231297));
#34990=CARTESIAN_POINT('Ctrl Pts',(7.07057502873392,-140.753019107145,4.082198396148));
#34991=CARTESIAN_POINT('Ctrl Pts',(9.42743337163542,-140.578019107145,-1.69756769845304E-11));
#34992=CARTESIAN_POINT('Ctrl Pts',(7.07057502871922,-140.403019107145,-4.08219839617346));
#34993=CARTESIAN_POINT('Ctrl Pts',(4.71371668580301,-140.228019107145,-8.16439679232994));
#34994=CARTESIAN_POINT('Ctrl Pts',(-1.4702867290402E-11,-140.053019107145,
-8.16439679232146));
#34995=CARTESIAN_POINT('Ctrl Pts',(-4.71371668583241,-139.878019107145,
-8.16439679231297));
#34996=CARTESIAN_POINT('Ctrl Pts',(-7.07057502873392,-139.703019107145,
-4.082198396148));
#34997=CARTESIAN_POINT('Ctrl Pts',(-9.42743337163542,-139.528019107145,
1.69768315121407E-11));
#34998=CARTESIAN_POINT('Ctrl Pts',(-7.07057502871922,-139.353019107145,
4.08219839617346));
#34999=CARTESIAN_POINT('Ctrl Pts',(-4.71371668580301,-139.178019107145,
8.16439679232994));
#35000=CARTESIAN_POINT('Ctrl Pts',(1.47018674401621E-11,-139.003019107145,
8.16439679232146));
#35001=CARTESIAN_POINT('Ctrl Pts',(4.71371668583241,-138.828019107145,8.16439679231297));
#35002=CARTESIAN_POINT('Ctrl Pts',(7.07057502873392,-138.653019107145,4.082198396148));
#35003=CARTESIAN_POINT('Ctrl Pts',(9.42743337163542,-138.478019107145,-1.69756769845304E-11));
#35004=CARTESIAN_POINT('Ctrl Pts',(7.07057502871922,-138.303019107145,-4.08219839617346));
#35005=CARTESIAN_POINT('Ctrl Pts',(4.71371668580301,-138.128019107145,-8.16439679232994));
#35006=CARTESIAN_POINT('Ctrl Pts',(-1.4702867290402E-11,-137.953019107145,
-8.16439679232146));
#35007=CARTESIAN_POINT('Ctrl Pts',(-4.71371668583241,-137.778019107145,
-8.16439679231297));
#35008=CARTESIAN_POINT('Ctrl Pts',(-7.07057502873392,-137.603019107145,
-4.082198396148));
#35009=CARTESIAN_POINT('Ctrl Pts',(-9.42743337163542,-137.428019107145,
1.69768315121407E-11));
#35010=CARTESIAN_POINT('Ctrl Pts',(-7.07057502871922,-137.253019107145,
4.08219839617346));
#35011=CARTESIAN_POINT('Ctrl Pts',(-4.71371668580301,-137.078019107145,
8.16439679232994));
#35012=CARTESIAN_POINT('Ctrl Pts',(1.47018674401621E-11,-136.903019107145,
8.16439679232146));
#35013=CARTESIAN_POINT('Ctrl Pts',(4.71371668583241,-136.728019107145,8.16439679231297));
#35014=CARTESIAN_POINT('Ctrl Pts',(7.07057502873392,-136.553019107145,4.082198396148));
#35015=CARTESIAN_POINT('Ctrl Pts',(9.42743337163542,-136.378019107145,-1.69756769845304E-11));
#35016=CARTESIAN_POINT('Ctrl Pts',(7.07057502871922,-136.203019107145,-4.08219839617346));
#35017=CARTESIAN_POINT('Ctrl Pts',(4.71371668580301,-136.028019107145,-8.16439679232994));
#35018=CARTESIAN_POINT('Ctrl Pts',(-1.4702867290402E-11,-135.853019107145,
-8.16439679232146));
#35019=CARTESIAN_POINT('Ctrl Pts',(-4.71371668583241,-135.678019107145,
-8.16439679231297));
#35020=CARTESIAN_POINT('Ctrl Pts',(-7.07057502873392,-135.503019107145,
-4.082198396148));
#35021=CARTESIAN_POINT('Ctrl Pts',(-9.42743337163542,-135.328019107145,
1.69768315121407E-11));
#35022=CARTESIAN_POINT('Ctrl Pts',(-7.07057502871922,-135.153019107145,
4.08219839617346));
#35023=CARTESIAN_POINT('Ctrl Pts',(-4.71371668580301,-134.978019107145,
8.16439679232994));
#35024=CARTESIAN_POINT('Ctrl Pts',(1.47018674401621E-11,-134.803019107145,
8.16439679232146));
#35025=CARTESIAN_POINT('Ctrl Pts',(4.71371668583241,-134.628019107145,8.16439679231297));
#35026=CARTESIAN_POINT('Ctrl Pts',(7.07057502873392,-134.453019107145,4.082198396148));
#35027=CARTESIAN_POINT('Ctrl Pts',(9.42743337163542,-134.278019107145,-1.69756769845304E-11));
#35028=CARTESIAN_POINT('Ctrl Pts',(7.07057502871922,-134.103019107145,-4.08219839617346));
#35029=CARTESIAN_POINT('Ctrl Pts',(4.71371668580301,-133.928019107145,-8.16439679232994));
#35030=CARTESIAN_POINT('Ctrl Pts',(-1.4702867290402E-11,-133.753019107145,
-8.16439679232146));
#35031=CARTESIAN_POINT('Ctrl Pts',(-4.71371668583241,-133.578019107145,
-8.16439679231297));
#35032=CARTESIAN_POINT('Ctrl Pts',(-7.07057502873392,-133.403019107145,
-4.082198396148));
#35033=CARTESIAN_POINT('Ctrl Pts',(-9.42743337163542,-133.228019107145,
1.69768315121407E-11));
#35034=CARTESIAN_POINT('Ctrl Pts',(-7.07057502871922,-133.053019107145,
4.08219839617346));
#35035=CARTESIAN_POINT('Ctrl Pts',(-4.71371668580301,-132.878019107145,
8.16439679232994));
#35036=CARTESIAN_POINT('Ctrl Pts',(1.47018674401621E-11,-132.703019107145,
8.16439679232146));
#35037=CARTESIAN_POINT('Ctrl Pts',(4.71371668583241,-132.528019107145,8.16439679231297));
#35038=CARTESIAN_POINT('Ctrl Pts',(7.07057502873392,-132.353019107145,4.082198396148));
#35039=CARTESIAN_POINT('Ctrl Pts',(9.42743337163542,-132.178019107145,-1.69756769845304E-11));
#35040=CARTESIAN_POINT('Ctrl Pts',(7.07057502871922,-132.003019107145,-4.08219839617346));
#35041=CARTESIAN_POINT('Ctrl Pts',(4.71371668580301,-131.828019107145,-8.16439679232994));
#35042=CARTESIAN_POINT('Ctrl Pts',(-1.4702867290402E-11,-131.653019107145,
-8.16439679232146));
#35043=CARTESIAN_POINT('Ctrl Pts',(-4.71371668583241,-131.478019107145,
-8.16439679231297));
#35044=CARTESIAN_POINT('Ctrl Pts',(-7.07057502873392,-131.303019107145,
-4.082198396148));
#35045=CARTESIAN_POINT('Ctrl Pts',(-9.42743337163542,-131.128019107145,
1.69768315121407E-11));
#35046=CARTESIAN_POINT('Ctrl Pts',(-7.07057502871922,-130.953019107145,
4.08219839617346));
#35047=CARTESIAN_POINT('Ctrl Pts',(-4.71371668580301,-130.778019107145,
8.16439679232994));
#35048=CARTESIAN_POINT('Ctrl Pts',(1.47018674401621E-11,-130.603019107145,
8.16439679232146));
#35049=CARTESIAN_POINT('Ctrl Pts',(4.71371668583241,-130.428019107145,8.16439679231297));
#35050=CARTESIAN_POINT('Ctrl Pts',(7.07057502873392,-130.253019107145,4.082198396148));
#35051=CARTESIAN_POINT('Ctrl Pts',(9.42743337163542,-130.078019107145,-1.69756769845304E-11));
#35052=CARTESIAN_POINT('Ctrl Pts',(7.07057502871922,-129.903019107145,-4.08219839617346));
#35053=CARTESIAN_POINT('Ctrl Pts',(4.71371668580301,-129.728019107145,-8.16439679232994));
#35054=CARTESIAN_POINT('Ctrl Pts',(-1.4702867290402E-11,-129.553019107145,
-8.16439679232146));
#35055=CARTESIAN_POINT('Ctrl Pts',(-4.71371668583241,-129.378019107145,
-8.16439679231297));
#35056=CARTESIAN_POINT('Ctrl Pts',(-7.07057502873392,-129.203019107145,
-4.082198396148));
#35057=CARTESIAN_POINT('Ctrl Pts',(-9.42743337163542,-129.028019107145,
1.69768315121407E-11));
#35058=CARTESIAN_POINT('Ctrl Pts',(-7.07057502871922,-128.853019107145,
4.08219839617346));
#35059=CARTESIAN_POINT('Ctrl Pts',(-4.71371668580301,-128.678019107145,
8.16439679232994));
#35060=CARTESIAN_POINT('Ctrl Pts',(1.47018674401621E-11,-128.503019107145,
8.16439679232146));
#35061=CARTESIAN_POINT('Ctrl Pts',(4.71371668583241,-128.328019107145,8.16439679231297));
#35062=CARTESIAN_POINT('Ctrl Pts',(7.07057502873392,-128.153019107145,4.082198396148));
#35063=CARTESIAN_POINT('Ctrl Pts',(9.42743337163542,-127.978019107145,-1.69756769845304E-11));
#35064=CARTESIAN_POINT('Ctrl Pts',(7.07057502871922,-127.803019107145,-4.08219839617346));
#35065=CARTESIAN_POINT('Ctrl Pts',(4.71371668580301,-127.628019107145,-8.16439679232994));
#35066=CARTESIAN_POINT('Ctrl Pts',(-1.4702867290402E-11,-127.453019107145,
-8.16439679232146));
#35067=CARTESIAN_POINT('Ctrl Pts',(-4.71371668583241,-127.278019107145,
-8.16439679231297));
#35068=CARTESIAN_POINT('Ctrl Pts',(-7.07057502873392,-127.103019107145,
-4.082198396148));
#35069=CARTESIAN_POINT('Ctrl Pts',(-9.42743337163542,-126.928019107145,
1.69768315121407E-11));
#35070=CARTESIAN_POINT('Ctrl Pts',(-7.07057502871922,-126.753019107145,
4.08219839617346));
#35071=CARTESIAN_POINT('Ctrl Pts',(-4.71371668580301,-126.578019107145,
8.16439679232994));
#35072=CARTESIAN_POINT('Ctrl Pts',(1.47018674401621E-11,-126.403019107145,
8.16439679232146));
#35073=CARTESIAN_POINT('Ctrl Pts',(4.71371668583241,-126.228019107145,8.16439679231297));
#35074=CARTESIAN_POINT('Ctrl Pts',(7.07057502873392,-126.053019107145,4.082198396148));
#35075=CARTESIAN_POINT('Ctrl Pts',(9.42743337163542,-125.878019107145,-1.69756769845304E-11));
#35076=CARTESIAN_POINT('Ctrl Pts',(7.07057502871922,-125.703019107145,-4.08219839617346));
#35077=CARTESIAN_POINT('Ctrl Pts',(4.71371668580301,-125.528019107145,-8.16439679232994));
#35078=CARTESIAN_POINT('Ctrl Pts',(-1.4702867290402E-11,-125.353019107145,
-8.16439679232146));
#35079=CARTESIAN_POINT('Ctrl Pts',(-4.71371668583241,-125.178019107145,
-8.16439679231297));
#35080=CARTESIAN_POINT('Ctrl Pts',(-7.07057502873392,-125.003019107145,
-4.082198396148));
#35081=CARTESIAN_POINT('Ctrl Pts',(-9.42743337163542,-124.828019107145,
1.69768315121407E-11));
#35082=CARTESIAN_POINT('Ctrl Pts',(-7.07057502871922,-124.653019107145,
4.08219839617346));
#35083=CARTESIAN_POINT('Ctrl Pts',(-4.71371668580301,-124.478019107145,
8.16439679232994));
#35084=CARTESIAN_POINT('Ctrl Pts',(1.47018674401621E-11,-124.303019107145,
8.16439679232146));
#35085=CARTESIAN_POINT('Ctrl Pts',(4.71371668583241,-124.128019107145,8.16439679231297));
#35086=CARTESIAN_POINT('Ctrl Pts',(7.07057502873392,-123.953019107145,4.082198396148));
#35087=CARTESIAN_POINT('Ctrl Pts',(9.42743337163542,-123.778019107145,-1.69756769845304E-11));
#35088=CARTESIAN_POINT('Ctrl Pts',(7.07057502871922,-123.603019107145,-4.08219839617346));
#35089=CARTESIAN_POINT('Ctrl Pts',(4.71371668580301,-123.428019107145,-8.16439679232994));
#35090=CARTESIAN_POINT('Ctrl Pts',(-1.4702867290402E-11,-123.253019107145,
-8.16439679232146));
#35091=CARTESIAN_POINT('Ctrl Pts',(-4.71371668583241,-123.078019107145,
-8.16439679231297));
#35092=CARTESIAN_POINT('Ctrl Pts',(-7.07057502873392,-122.903019107145,
-4.082198396148));
#35093=CARTESIAN_POINT('Ctrl Pts',(-9.42743337163542,-122.728019107145,
1.69768315121407E-11));
#35094=CARTESIAN_POINT('Ctrl Pts',(-7.07057502871922,-122.553019107145,
4.08219839617346));
#35095=CARTESIAN_POINT('Ctrl Pts',(-4.71371668580301,-122.378019107145,
8.16439679232994));
#35096=CARTESIAN_POINT('Ctrl Pts',(1.47018674401621E-11,-122.203019107145,
8.16439679232146));
#35097=CARTESIAN_POINT('Ctrl Pts',(4.71371668583241,-122.028019107145,8.16439679231297));
#35098=CARTESIAN_POINT('Ctrl Pts',(7.07057502873392,-121.853019107145,4.082198396148));
#35099=CARTESIAN_POINT('Ctrl Pts',(9.42743337163542,-121.678019107145,-1.69756769845304E-11));
#35100=CARTESIAN_POINT('Ctrl Pts',(7.07057502871922,-121.503019107145,-4.08219839617346));
#35101=CARTESIAN_POINT('Ctrl Pts',(4.71371668580301,-121.328019107145,-8.16439679232994));
#35102=CARTESIAN_POINT('Ctrl Pts',(-1.4702867290402E-11,-121.153019107145,
-8.16439679232146));
#35103=CARTESIAN_POINT('Ctrl Pts',(-4.71371668583241,-120.978019107145,
-8.16439679231297));
#35104=CARTESIAN_POINT('Ctrl Pts',(-7.07057502873392,-120.803019107145,
-4.082198396148));
#35105=CARTESIAN_POINT('Ctrl Pts',(-9.42743337163542,-120.628019107145,
1.69768315121407E-11));
#35106=CARTESIAN_POINT('Ctrl Pts',(-7.07057502871922,-120.453019107145,
4.08219839617346));
#35107=CARTESIAN_POINT('Ctrl Pts',(-4.71371668580301,-120.278019107145,
8.16439679232994));
#35108=CARTESIAN_POINT('Ctrl Pts',(1.47018674401621E-11,-120.103019107145,
8.16439679232146));
#35109=CARTESIAN_POINT('Ctrl Pts',(4.71371668583241,-119.928019107145,8.16439679231297));
#35110=CARTESIAN_POINT('Ctrl Pts',(7.07057502873392,-119.753019107145,4.082198396148));
#35111=CARTESIAN_POINT('Ctrl Pts',(9.42743337163542,-119.578019107145,-1.69756769845304E-11));
#35112=CARTESIAN_POINT('Ctrl Pts',(7.07057502871922,-119.403019107145,-4.08219839617346));
#35113=CARTESIAN_POINT('Ctrl Pts',(4.71371668580301,-119.228019107145,-8.16439679232994));
#35114=CARTESIAN_POINT('Ctrl Pts',(-1.4702867290402E-11,-119.053019107145,
-8.16439679232146));
#35115=CARTESIAN_POINT('Ctrl Pts',(-4.71371668583241,-118.878019107145,
-8.16439679231297));
#35116=CARTESIAN_POINT('Ctrl Pts',(-7.07057502873392,-118.703019107145,
-4.082198396148));
#35117=CARTESIAN_POINT('Ctrl Pts',(-9.42743337163542,-118.528019107145,
1.69768315121407E-11));
#35118=CARTESIAN_POINT('Ctrl Pts',(-7.07057502871922,-118.353019107145,
4.08219839617346));
#35119=CARTESIAN_POINT('Ctrl Pts',(-4.71371668580301,-118.178019107145,
8.16439679232994));
#35120=CARTESIAN_POINT('Ctrl Pts',(1.47018674401621E-11,-118.003019107145,
8.16439679232146));
#35121=CARTESIAN_POINT('Ctrl Pts',(4.71371668583241,-117.828019107145,8.16439679231297));
#35122=CARTESIAN_POINT('Ctrl Pts',(7.07057502873392,-117.653019107145,4.082198396148));
#35123=CARTESIAN_POINT('Ctrl Pts',(9.42743337163542,-117.478019107145,-1.69756769845304E-11));
#35124=CARTESIAN_POINT('Ctrl Pts',(7.07057502871922,-117.303019107145,-4.08219839617346));
#35125=CARTESIAN_POINT('Ctrl Pts',(4.71371668580301,-117.128019107145,-8.16439679232994));
#35126=CARTESIAN_POINT('Ctrl Pts',(-1.4702867290402E-11,-116.953019107145,
-8.16439679232146));
#35127=CARTESIAN_POINT('Ctrl Pts',(-4.71371668583241,-116.778019107145,
-8.16439679231297));
#35128=CARTESIAN_POINT('Ctrl Pts',(-7.07057502873392,-116.603019107145,
-4.082198396148));
#35129=CARTESIAN_POINT('Ctrl Pts',(-9.42743337163542,-116.428019107145,
1.69768315121407E-11));
#35130=CARTESIAN_POINT('Ctrl Pts',(-7.07057502871922,-116.253019107145,
4.08219839617346));
#35131=CARTESIAN_POINT('Ctrl Pts',(-4.71371668580301,-116.078019107145,
8.16439679232994));
#35132=CARTESIAN_POINT('Ctrl Pts',(1.47018674401621E-11,-115.903019107145,
8.16439679232146));
#35133=CARTESIAN_POINT('Ctrl Pts',(4.71371668583241,-115.728019107145,8.16439679231297));
#35134=CARTESIAN_POINT('Ctrl Pts',(7.07057502873392,-115.553019107145,4.082198396148));
#35135=CARTESIAN_POINT('Ctrl Pts',(9.42743337163542,-115.378019107145,-1.69756769845304E-11));
#35136=CARTESIAN_POINT('Ctrl Pts',(7.07057502871922,-115.203019107145,-4.08219839617346));
#35137=CARTESIAN_POINT('Ctrl Pts',(4.71371668580301,-115.028019107145,-8.16439679232994));
#35138=CARTESIAN_POINT('Ctrl Pts',(-1.4702867290402E-11,-114.853019107145,
-8.16439679232146));
#35139=CARTESIAN_POINT('Ctrl Pts',(-4.71371668583241,-114.678019107145,
-8.16439679231297));
#35140=CARTESIAN_POINT('Ctrl Pts',(-7.07057502873392,-114.503019107145,
-4.082198396148));
#35141=CARTESIAN_POINT('Ctrl Pts',(-9.42743337163542,-114.328019107145,
1.69768315121407E-11));
#35142=CARTESIAN_POINT('Ctrl Pts',(-7.07057502871922,-114.153019107145,
4.08219839617346));
#35143=CARTESIAN_POINT('Ctrl Pts',(-4.71371668580301,-113.978019107145,
8.16439679232994));
#35144=CARTESIAN_POINT('Ctrl Pts',(1.47018674401621E-11,-113.803019107145,
8.16439679232146));
#35145=CARTESIAN_POINT('Ctrl Pts',(4.71371668583241,-113.628019107145,8.16439679231297));
#35146=CARTESIAN_POINT('Ctrl Pts',(7.07057502873392,-113.453019107145,4.082198396148));
#35147=CARTESIAN_POINT('Ctrl Pts',(9.42743337163542,-113.278019107145,-1.69756769845304E-11));
#35148=CARTESIAN_POINT('Ctrl Pts',(7.07057502871922,-113.103019107145,-4.08219839617346));
#35149=CARTESIAN_POINT('Ctrl Pts',(4.71371668580301,-112.928019107145,-8.16439679232994));
#35150=CARTESIAN_POINT('Ctrl Pts',(-1.4702867290402E-11,-112.753019107145,
-8.16439679232146));
#35151=CARTESIAN_POINT('Ctrl Pts',(-4.71371668583241,-112.578019107145,
-8.16439679231297));
#35152=CARTESIAN_POINT('Ctrl Pts',(-7.07057502873392,-112.403019107145,
-4.082198396148));
#35153=CARTESIAN_POINT('Ctrl Pts',(-9.42743337163542,-112.228019107145,
1.69768315121407E-11));
#35154=CARTESIAN_POINT('Ctrl Pts',(-7.07057502871922,-112.053019107145,
4.08219839617346));
#35155=CARTESIAN_POINT('Ctrl Pts',(-4.71371668580301,-111.878019107145,
8.16439679232994));
#35156=CARTESIAN_POINT('Ctrl Pts',(1.47018674401621E-11,-111.703019107145,
8.16439679232146));
#35157=CARTESIAN_POINT('Ctrl Pts',(4.71371668583241,-111.528019107145,8.16439679231297));
#35158=CARTESIAN_POINT('Ctrl Pts',(7.07057502873392,-111.353019107145,4.082198396148));
#35159=CARTESIAN_POINT('Ctrl Pts',(9.42743337163542,-111.178019107145,-1.69756769845304E-11));
#35160=CARTESIAN_POINT('Ctrl Pts',(7.07057502871922,-111.003019107145,-4.08219839617346));
#35161=CARTESIAN_POINT('Ctrl Pts',(4.71371668580301,-110.828019107145,-8.16439679232994));
#35162=CARTESIAN_POINT('Ctrl Pts',(-1.4702867290402E-11,-110.653019107145,
-8.16439679232146));
#35163=CARTESIAN_POINT('Ctrl Pts',(-4.71371668583241,-110.478019107145,
-8.16439679231297));
#35164=CARTESIAN_POINT('Ctrl Pts',(-7.07057502873392,-110.303019107145,
-4.082198396148));
#35165=CARTESIAN_POINT('Ctrl Pts',(-9.42743337163542,-110.128019107145,
1.69768315121407E-11));
#35166=CARTESIAN_POINT('Ctrl Pts',(-7.07057502871922,-109.953019107145,
4.08219839617346));
#35167=CARTESIAN_POINT('Ctrl Pts',(-4.71371668580301,-109.778019107145,
8.16439679232994));
#35168=CARTESIAN_POINT('Ctrl Pts',(1.47018674401621E-11,-109.603019107145,
8.16439679232146));
#35169=CARTESIAN_POINT('Ctrl Pts',(4.71371668583241,-109.428019107145,8.16439679231297));
#35170=CARTESIAN_POINT('Ctrl Pts',(7.07057502873392,-109.253019107145,4.082198396148));
#35171=CARTESIAN_POINT('Ctrl Pts',(9.42743337163542,-109.078019107145,-1.69756769845304E-11));
#35172=CARTESIAN_POINT('Ctrl Pts',(7.07057502871922,-108.903019107145,-4.08219839617346));
#35173=CARTESIAN_POINT('Ctrl Pts',(4.71371668580301,-108.728019107145,-8.16439679232994));
#35174=CARTESIAN_POINT('Ctrl Pts',(-1.4702867290402E-11,-108.553019107145,
-8.16439679232146));
#35175=CARTESIAN_POINT('Ctrl Pts',(-4.71371668583241,-108.378019107145,
-8.16439679231297));
#35176=CARTESIAN_POINT('Ctrl Pts',(-7.07057502873392,-108.203019107145,
-4.082198396148));
#35177=CARTESIAN_POINT('Ctrl Pts',(-9.42743337163542,-108.028019107145,
1.69768315121407E-11));
#35178=CARTESIAN_POINT('Ctrl Pts',(-7.07057502871922,-107.853019107145,
4.08219839617346));
#35179=CARTESIAN_POINT('Ctrl Pts',(-4.71371668580301,-107.678019107145,
8.16439679232994));
#35180=CARTESIAN_POINT('Ctrl Pts',(1.47018674401621E-11,-107.503019107145,
8.16439679232146));
#35181=CARTESIAN_POINT('Ctrl Pts',(4.71371668583241,-107.328019107145,8.16439679231297));
#35182=CARTESIAN_POINT('Ctrl Pts',(7.07057502873392,-107.153019107145,4.082198396148));
#35183=CARTESIAN_POINT('Ctrl Pts',(9.42743337163542,-106.978019107145,-1.69756769845304E-11));
#35184=CARTESIAN_POINT('Ctrl Pts',(7.07057502871922,-106.803019107145,-4.08219839617346));
#35185=CARTESIAN_POINT('Ctrl Pts',(4.71371668580301,-106.628019107145,-8.16439679232994));
#35186=CARTESIAN_POINT('Ctrl Pts',(-1.4702867290402E-11,-106.453019107145,
-8.16439679232146));
#35187=CARTESIAN_POINT('Ctrl Pts',(-4.71371668583241,-106.278019107145,
-8.16439679231297));
#35188=CARTESIAN_POINT('Ctrl Pts',(-7.07057502873392,-106.103019107145,
-4.082198396148));
#35189=CARTESIAN_POINT('Ctrl Pts',(-9.42743337163542,-105.928019107145,
1.69768315121407E-11));
#35190=CARTESIAN_POINT('Ctrl Pts',(-7.07057502871922,-105.753019107145,
4.08219839617346));
#35191=CARTESIAN_POINT('Ctrl Pts',(-4.71371668580301,-105.578019107145,
8.16439679232994));
#35192=CARTESIAN_POINT('Ctrl Pts',(1.47018674401621E-11,-105.403019107145,
8.16439679232146));
#35193=CARTESIAN_POINT('Ctrl Pts',(4.71371668583241,-105.228019107145,8.16439679231297));
#35194=CARTESIAN_POINT('Ctrl Pts',(7.07057502873392,-105.053019107145,4.082198396148));
#35195=CARTESIAN_POINT('Ctrl Pts',(9.42743337163542,-104.878019107145,-1.69756769845304E-11));
#35196=CARTESIAN_POINT('Ctrl Pts',(7.07057502871922,-104.703019107145,-4.08219839617346));
#35197=CARTESIAN_POINT('Ctrl Pts',(4.71371668580301,-104.528019107145,-8.16439679232994));
#35198=CARTESIAN_POINT('Ctrl Pts',(-1.4702867290402E-11,-104.353019107145,
-8.16439679232146));
#35199=CARTESIAN_POINT('Ctrl Pts',(-4.71371668583241,-104.178019107145,
-8.16439679231297));
#35200=CARTESIAN_POINT('Ctrl Pts',(-7.07057502873392,-104.003019107145,
-4.082198396148));
#35201=CARTESIAN_POINT('Ctrl Pts',(-9.42743337163542,-103.828019107145,
1.69768315121407E-11));
#35202=CARTESIAN_POINT('Ctrl Pts',(-7.07057502871922,-103.653019107145,
4.08219839617346));
#35203=CARTESIAN_POINT('Ctrl Pts',(-4.71371668580301,-103.478019107145,
8.16439679232994));
#35204=CARTESIAN_POINT('Ctrl Pts',(1.47018674401621E-11,-103.303019107145,
8.16439679232146));
#35205=CARTESIAN_POINT('Ctrl Pts',(4.71371668583241,-103.128019107145,8.16439679231297));
#35206=CARTESIAN_POINT('Ctrl Pts',(7.07057502873392,-102.953019107145,4.082198396148));
#35207=CARTESIAN_POINT('Ctrl Pts',(9.42743337163542,-102.778019107145,-1.69756769845304E-11));
#35208=CARTESIAN_POINT('Ctrl Pts',(7.07057502871922,-102.603019107145,-4.08219839617346));
#35209=CARTESIAN_POINT('Ctrl Pts',(4.71371668580301,-102.428019107145,-8.16439679232994));
#35210=CARTESIAN_POINT('Ctrl Pts',(-1.4702867290402E-11,-102.253019107145,
-8.16439679232146));
#35211=CARTESIAN_POINT('Ctrl Pts',(-4.71371668583241,-102.078019107145,
-8.16439679231297));
#35212=CARTESIAN_POINT('Ctrl Pts',(-7.07057502873392,-101.903019107145,
-4.082198396148));
#35213=CARTESIAN_POINT('Ctrl Pts',(-9.42743337163542,-101.728019107145,
1.69768315121407E-11));
#35214=CARTESIAN_POINT('Ctrl Pts',(-7.07057502871922,-101.553019107145,
4.08219839617346));
#35215=CARTESIAN_POINT('Ctrl Pts',(-4.71371668580301,-101.378019107145,
8.16439679232994));
#35216=CARTESIAN_POINT('Ctrl Pts',(1.47018674401621E-11,-101.203019107145,
8.16439679232146));
#35217=CARTESIAN_POINT('Ctrl Pts',(4.71371668583241,-101.028019107145,8.16439679231297));
#35218=CARTESIAN_POINT('Ctrl Pts',(7.07057502873392,-100.853019107145,4.082198396148));
#35219=CARTESIAN_POINT('Ctrl Pts',(9.42743337163542,-100.678019107145,-1.69756769845304E-11));
#35220=CARTESIAN_POINT('Ctrl Pts',(7.07057502871922,-100.503019107145,-4.08219839617346));
#35221=CARTESIAN_POINT('Ctrl Pts',(4.71371668580301,-100.328019107145,-8.16439679232994));
#35222=CARTESIAN_POINT('Ctrl Pts',(-1.4702867290402E-11,-100.153019107145,
-8.16439679232146));
#35223=CARTESIAN_POINT('Ctrl Pts',(-4.71371668583241,-99.9780191071451,
-8.16439679231297));
#35224=CARTESIAN_POINT('Ctrl Pts',(-7.07057502873392,-99.8030191071451,
-4.082198396148));
#35225=CARTESIAN_POINT('Ctrl Pts',(-9.42743337163542,-99.6280191071451,
1.69768315121407E-11));
#35226=CARTESIAN_POINT('Ctrl Pts',(-7.07057502871922,-99.4530191071451,
4.08219839617346));
#35227=CARTESIAN_POINT('Ctrl Pts',(-4.71371668580301,-99.2780191071451,
8.16439679232994));
#35228=CARTESIAN_POINT('Ctrl Pts',(1.47018674401621E-11,-99.1030191071451,
8.16439679232146));
#35229=CARTESIAN_POINT('Ctrl Pts',(4.71371668583241,-98.9280191071451,8.16439679231297));
#35230=CARTESIAN_POINT('Ctrl Pts',(7.07057502873392,-98.7530191071451,4.082198396148));
#35231=CARTESIAN_POINT('Ctrl Pts',(9.42743337163542,-98.5780191071451,-1.69756769845304E-11));
#35232=CARTESIAN_POINT('Ctrl Pts',(7.07057502871922,-98.4030191071451,-4.08219839617346));
#35233=CARTESIAN_POINT('Ctrl Pts',(4.71371668580301,-98.2280191071451,-8.16439679232994));
#35234=CARTESIAN_POINT('Ctrl Pts',(-1.4702867290402E-11,-98.0530191071451,
-8.16439679232146));
#35235=CARTESIAN_POINT('Ctrl Pts',(-4.71371668583241,-97.8780191071451,
-8.16439679231297));
#35236=CARTESIAN_POINT('Ctrl Pts',(-7.07057502873392,-97.7030191071451,
-4.082198396148));
#35237=CARTESIAN_POINT('Ctrl Pts',(-9.42743337163542,-97.5280191071451,
1.69768315121407E-11));
#35238=CARTESIAN_POINT('Ctrl Pts',(-7.07057502871922,-97.3530191071451,
4.08219839617346));
#35239=CARTESIAN_POINT('Ctrl Pts',(-4.71371668580301,-97.1780191071451,
8.16439679232994));
#35240=CARTESIAN_POINT('Ctrl Pts',(1.47018674401621E-11,-97.0030191071451,
8.16439679232146));
#35241=CARTESIAN_POINT('Ctrl Pts',(4.71371668583241,-96.8280191071451,8.16439679231297));
#35242=CARTESIAN_POINT('Ctrl Pts',(7.07057502873392,-96.6530191071451,4.082198396148));
#35243=CARTESIAN_POINT('Ctrl Pts',(9.42743337163542,-96.4780191071451,-1.69756769845304E-11));
#35244=CARTESIAN_POINT('Ctrl Pts',(7.07057502871922,-96.3030191071451,-4.08219839617346));
#35245=CARTESIAN_POINT('Ctrl Pts',(4.71371668580301,-96.1280191071451,-8.16439679232994));
#35246=CARTESIAN_POINT('Ctrl Pts',(-1.4702867290402E-11,-95.9530191071451,
-8.16439679232146));
#35247=CARTESIAN_POINT('Ctrl Pts',(-4.71371668583241,-95.7780191071451,
-8.16439679231297));
#35248=CARTESIAN_POINT('Ctrl Pts',(-7.07057502873392,-95.6030191071451,
-4.082198396148));
#35249=CARTESIAN_POINT('Ctrl Pts',(-9.42743337163542,-95.4280191071451,
1.69768315121407E-11));
#35250=CARTESIAN_POINT('Ctrl Pts',(-7.07057502871922,-95.2530191071451,
4.08219839617346));
#35251=CARTESIAN_POINT('Ctrl Pts',(-4.71371668580301,-95.0780191071451,
8.16439679232994));
#35252=CARTESIAN_POINT('Ctrl Pts',(1.47018674401621E-11,-94.9030191071451,
8.16439679232146));
#35253=CARTESIAN_POINT('Ctrl Pts',(4.71371668583241,-94.7280191071451,8.16439679231297));
#35254=CARTESIAN_POINT('Ctrl Pts',(7.07057502873392,-94.5530191071451,4.082198396148));
#35255=CARTESIAN_POINT('Ctrl Pts',(9.42743337163542,-94.3780191071451,-1.69756769845304E-11));
#35256=CARTESIAN_POINT('Ctrl Pts',(7.07057502871922,-94.2030191071451,-4.08219839617346));
#35257=CARTESIAN_POINT('Ctrl Pts',(4.71371668580301,-94.0280191071451,-8.16439679232994));
#35258=CARTESIAN_POINT('Ctrl Pts',(-1.4702867290402E-11,-93.8530191071451,
-8.16439679232146));
#35259=CARTESIAN_POINT('Ctrl Pts',(-4.71371668583241,-93.6780191071451,
-8.16439679231297));
#35260=CARTESIAN_POINT('Ctrl Pts',(-7.07057502873392,-93.5030191071451,
-4.082198396148));
#35261=CARTESIAN_POINT('Ctrl Pts',(-9.42743337163542,-93.3280191071451,
1.69768315121407E-11));
#35262=CARTESIAN_POINT('Ctrl Pts',(-7.07057502871922,-93.1530191071451,
4.08219839617346));
#35263=CARTESIAN_POINT('Ctrl Pts',(-4.71371668580301,-92.9780191071451,
8.16439679232994));
#35264=CARTESIAN_POINT('Ctrl Pts',(1.47018674401621E-11,-92.8030191071451,
8.16439679232146));
#35265=CARTESIAN_POINT('Ctrl Pts',(4.71371668583241,-92.6280191071451,8.16439679231297));
#35266=CARTESIAN_POINT('Ctrl Pts',(7.07057502873392,-92.4530191071451,4.082198396148));
#35267=CARTESIAN_POINT('Ctrl Pts',(9.42743337163542,-92.2780191071451,-1.69756769845304E-11));
#35268=CARTESIAN_POINT('Ctrl Pts',(7.07057502871922,-92.1030191071451,-4.08219839617346));
#35269=CARTESIAN_POINT('Ctrl Pts',(4.71371668580301,-91.9280191071451,-8.16439679232994));
#35270=CARTESIAN_POINT('Ctrl Pts',(-1.4702867290402E-11,-91.7530191071451,
-8.16439679232146));
#35271=CARTESIAN_POINT('Ctrl Pts',(-4.71371668583241,-91.5780191071451,
-8.16439679231297));
#35272=CARTESIAN_POINT('Ctrl Pts',(-7.07057502873392,-91.4030191071451,
-4.082198396148));
#35273=CARTESIAN_POINT('Ctrl Pts',(-9.42743337163542,-91.2280191071451,
1.69768315121407E-11));
#35274=CARTESIAN_POINT('Ctrl Pts',(-7.07057502871922,-91.0530191071451,
4.08219839617346));
#35275=CARTESIAN_POINT('Ctrl Pts',(-4.71371668580301,-90.8780191071451,
8.16439679232994));
#35276=CARTESIAN_POINT('Ctrl Pts',(1.47018674401621E-11,-90.7030191071451,
8.16439679232146));
#35277=CARTESIAN_POINT('Ctrl Pts',(4.71371668583241,-90.5280191071451,8.16439679231297));
#35278=CARTESIAN_POINT('Ctrl Pts',(7.07057502873392,-90.3530191071451,4.082198396148));
#35279=CARTESIAN_POINT('Ctrl Pts',(9.42743337163542,-90.1780191071451,-1.69756769845304E-11));
#35280=CARTESIAN_POINT('Ctrl Pts',(7.07057502871922,-90.0030191071451,-4.08219839617346));
#35281=CARTESIAN_POINT('Ctrl Pts',(4.71371668580301,-89.8280191071451,-8.16439679232994));
#35282=CARTESIAN_POINT('Ctrl Pts',(-1.4702867290402E-11,-89.6530191071451,
-8.16439679232146));
#35283=CARTESIAN_POINT('Ctrl Pts',(-4.71371668583241,-89.4780191071451,
-8.16439679231297));
#35284=CARTESIAN_POINT('Ctrl Pts',(-7.07057502873392,-89.3030191071451,
-4.082198396148));
#35285=CARTESIAN_POINT('Ctrl Pts',(-9.42743337163542,-89.1280191071451,
1.69768315121407E-11));
#35286=CARTESIAN_POINT('Ctrl Pts',(-7.07057502871922,-88.9530191071451,
4.08219839617346));
#35287=CARTESIAN_POINT('Ctrl Pts',(-4.71371668580301,-88.7780191071451,
8.16439679232994));
#35288=CARTESIAN_POINT('Ctrl Pts',(1.47018674401621E-11,-88.6030191071451,
8.16439679232146));
#35289=CARTESIAN_POINT('Ctrl Pts',(4.71371668583241,-88.4280191071451,8.16439679231297));
#35290=CARTESIAN_POINT('Ctrl Pts',(7.07057502873392,-88.2530191071451,4.082198396148));
#35291=CARTESIAN_POINT('Ctrl Pts',(9.42743337163542,-88.0780191071452,-1.69756769845304E-11));
#35292=CARTESIAN_POINT('Ctrl Pts',(7.07057502871922,-87.9030191071451,-4.08219839617346));
#35293=CARTESIAN_POINT('Ctrl Pts',(4.71371668580301,-87.7280191071451,-8.16439679232994));
#35294=CARTESIAN_POINT('Ctrl Pts',(-1.4702867290402E-11,-87.5530191071451,
-8.16439679232146));
#35295=CARTESIAN_POINT('Ctrl Pts',(-4.71371668583241,-87.3780191071451,
-8.16439679231297));
#35296=CARTESIAN_POINT('Ctrl Pts',(-7.07057502873392,-87.2030191071451,
-4.082198396148));
#35297=CARTESIAN_POINT('Ctrl Pts',(-9.42743337163542,-87.0280191071451,
1.69768315121407E-11));
#35298=CARTESIAN_POINT('Ctrl Pts',(-7.07057502871922,-86.8530191071451,
4.08219839617346));
#35299=CARTESIAN_POINT('Ctrl Pts',(-4.71371668580301,-86.6780191071451,
8.16439679232994));
#35300=CARTESIAN_POINT('Ctrl Pts',(1.47018674401621E-11,-86.5030191071452,
8.16439679232146));
#35301=CARTESIAN_POINT('Ctrl Pts',(4.71371668583241,-86.3280191071451,8.16439679231297));
#35302=CARTESIAN_POINT('Ctrl Pts',(7.07057502873392,-86.1530191071451,4.082198396148));
#35303=CARTESIAN_POINT('Ctrl Pts',(9.42743337163542,-85.9780191071451,-1.69756769845304E-11));
#35304=CARTESIAN_POINT('Ctrl Pts',(7.07057502871922,-85.8030191071452,-4.08219839617346));
#35305=CARTESIAN_POINT('Ctrl Pts',(4.71371668580301,-85.6280191071451,-8.16439679232994));
#35306=CARTESIAN_POINT('Ctrl Pts',(-1.4702867290402E-11,-85.4530191071451,
-8.16439679232146));
#35307=CARTESIAN_POINT('Ctrl Pts',(-4.71371668583241,-85.2780191071451,
-8.16439679231297));
#35308=CARTESIAN_POINT('Ctrl Pts',(-7.07057502873392,-85.1030191071451,
-4.082198396148));
#35309=CARTESIAN_POINT('Ctrl Pts',(-9.42743337163542,-84.9280191071451,
1.69768315121407E-11));
#35310=CARTESIAN_POINT('Ctrl Pts',(-7.07057502871922,-84.7530191071451,
4.08219839617346));
#35311=CARTESIAN_POINT('Ctrl Pts',(-4.71371668580301,-84.5780191071451,
8.16439679232994));
#35312=CARTESIAN_POINT('Ctrl Pts',(1.47018674401621E-11,-84.4030191071451,
8.16439679232146));
#35313=CARTESIAN_POINT('Ctrl Pts',(4.71371668583241,-84.2280191071451,8.16439679231297));
#35314=CARTESIAN_POINT('Ctrl Pts',(7.07057502873392,-84.0530191071451,4.082198396148));
#35315=CARTESIAN_POINT('Ctrl Pts',(9.42743337163542,-83.8780191071451,-1.69756769845304E-11));
#35316=CARTESIAN_POINT('Ctrl Pts',(7.07057502871922,-83.7030191071452,-4.08219839617346));
#35317=CARTESIAN_POINT('Ctrl Pts',(4.71371668580301,-83.5280191071451,-8.16439679232994));
#35318=CARTESIAN_POINT('Ctrl Pts',(-1.4702867290402E-11,-83.3530191071451,
-8.16439679232146));
#35319=CARTESIAN_POINT('Ctrl Pts',(-4.71371668583241,-83.1780191071451,
-8.16439679231297));
#35320=CARTESIAN_POINT('Ctrl Pts',(-7.07057502873392,-83.0030191071451,
-4.082198396148));
#35321=CARTESIAN_POINT('Ctrl Pts',(-9.42743337163542,-82.8280191071451,
1.69768315121407E-11));
#35322=CARTESIAN_POINT('Ctrl Pts',(-7.07057502871922,-82.6530191071451,
4.08219839617346));
#35323=CARTESIAN_POINT('Ctrl Pts',(-4.71371668580301,-82.4780191071451,
8.16439679232994));
#35324=CARTESIAN_POINT('Ctrl Pts',(1.47018674401621E-11,-82.3030191071451,
8.16439679232146));
#35325=CARTESIAN_POINT('Ctrl Pts',(4.71371668583241,-82.1280191071452,8.16439679231297));
#35326=CARTESIAN_POINT('Ctrl Pts',(7.07057502873392,-81.9530191071452,4.082198396148));
#35327=CARTESIAN_POINT('Ctrl Pts',(9.42743337163542,-81.7780191071451,-1.69756769845304E-11));
#35328=CARTESIAN_POINT('Ctrl Pts',(7.07057502871922,-81.6030191071452,-4.08219839617346));
#35329=CARTESIAN_POINT('Ctrl Pts',(4.71371668580301,-81.4280191071452,-8.16439679232994));
#35330=CARTESIAN_POINT('Ctrl Pts',(-1.4702867290402E-11,-81.2530191071451,
-8.16439679232146));
#35331=CARTESIAN_POINT('Ctrl Pts',(-4.71371668583241,-81.0780191071451,
-8.16439679231297));
#35332=CARTESIAN_POINT('Ctrl Pts',(-7.07057502873392,-80.9030191071452,
-4.082198396148));
#35333=CARTESIAN_POINT('Ctrl Pts',(-9.42743337163542,-80.7280191071451,
1.69768315121407E-11));
#35334=CARTESIAN_POINT('Ctrl Pts',(-7.07057502871922,-80.5530191071452,
4.08219839617346));
#35335=CARTESIAN_POINT('Ctrl Pts',(-4.71371668580301,-80.3780191071451,
8.16439679232994));
#35336=CARTESIAN_POINT('Ctrl Pts',(1.47018674401621E-11,-80.2030191071451,
8.16439679232146));
#35337=CARTESIAN_POINT('Ctrl Pts',(4.71371668583241,-80.0280191071451,8.16439679231297));
#35338=CARTESIAN_POINT('Ctrl Pts',(7.07057502873392,-79.8530191071451,4.082198396148));
#35339=CARTESIAN_POINT('Ctrl Pts',(9.42743337163542,-79.6780191071451,-1.69756769845304E-11));
#35340=CARTESIAN_POINT('Ctrl Pts',(7.07057502871922,-79.5030191071451,-4.08219839617346));
#35341=CARTESIAN_POINT('Ctrl Pts',(4.71371668580301,-79.3280191071452,-8.16439679232994));
#35342=CARTESIAN_POINT('Ctrl Pts',(-1.4702867290402E-11,-79.1530191071452,
-8.16439679232146));
#35343=CARTESIAN_POINT('Ctrl Pts',(-4.71371668583241,-78.9780191071451,
-8.16439679231297));
#35344=CARTESIAN_POINT('Ctrl Pts',(-7.07057502873392,-78.8030191071452,
-4.082198396148));
#35345=CARTESIAN_POINT('Ctrl Pts',(-9.42743337163542,-78.6280191071451,
1.69768315121407E-11));
#35346=CARTESIAN_POINT('Ctrl Pts',(-7.07057502871922,-78.4530191071451,
4.08219839617346));
#35347=CARTESIAN_POINT('Ctrl Pts',(-4.71371668580301,-78.2780191071452,
8.16439679232994));
#35348=CARTESIAN_POINT('Ctrl Pts',(1.47018674401621E-11,-78.1030191071452,
8.16439679232146));
#35349=CARTESIAN_POINT('Ctrl Pts',(4.71371668583241,-77.9280191071451,8.16439679231297));
#35350=CARTESIAN_POINT('Ctrl Pts',(7.07057502873392,-77.7530191071452,4.082198396148));
#35351=CARTESIAN_POINT('Ctrl Pts',(9.42743337163542,-77.5780191071452,-1.69756769845304E-11));
#35352=CARTESIAN_POINT('Ctrl Pts',(7.07057502871922,-77.4030191071451,-4.08219839617346));
#35353=CARTESIAN_POINT('Ctrl Pts',(4.71371668580301,-77.2280191071452,-8.16439679232994));
#35354=CARTESIAN_POINT('Ctrl Pts',(-1.4702867290402E-11,-77.0530191071452,
-8.16439679232146));
#35355=CARTESIAN_POINT('Ctrl Pts',(-4.71371668583241,-76.8780191071451,
-8.16439679231297));
#35356=CARTESIAN_POINT('Ctrl Pts',(-7.07057502873392,-76.7030191071452,
-4.082198396148));
#35357=CARTESIAN_POINT('Ctrl Pts',(-9.42743337163542,-76.5280191071452,
1.69768315121407E-11));
#35358=CARTESIAN_POINT('Ctrl Pts',(-7.07057502871922,-76.3530191071451,
4.08219839617346));
#35359=CARTESIAN_POINT('Ctrl Pts',(-4.71371668580301,-76.1780191071451,
8.16439679232994));
#35360=CARTESIAN_POINT('Ctrl Pts',(1.47018674401621E-11,-76.0030191071452,
8.16439679232146));
#35361=CARTESIAN_POINT('Ctrl Pts',(4.71371668583241,-75.8280191071452,8.16439679231297));
#35362=CARTESIAN_POINT('Ctrl Pts',(7.07057502873392,-75.6530191071451,4.082198396148));
#35363=CARTESIAN_POINT('Ctrl Pts',(9.42743337163542,-75.4780191071452,-1.69756769845304E-11));
#35364=CARTESIAN_POINT('Ctrl Pts',(7.07057502871922,-75.3030191071451,-4.08219839617346));
#35365=CARTESIAN_POINT('Ctrl Pts',(4.71371668580301,-75.1280191071451,-8.16439679232994));
#35366=CARTESIAN_POINT('Ctrl Pts',(-1.4702867290402E-11,-74.9530191071452,
-8.16439679232146));
#35367=CARTESIAN_POINT('Ctrl Pts',(-4.71371668583241,-74.7780191071452,
-8.16439679231297));
#35368=CARTESIAN_POINT('Ctrl Pts',(-7.07057502873392,-74.6030191071451,
-4.082198396148));
#35369=CARTESIAN_POINT('Ctrl Pts',(-9.42743337163542,-74.4280191071451,
1.69768315121407E-11));
#35370=CARTESIAN_POINT('Ctrl Pts',(-7.07057502871922,-74.2530191071452,
4.08219839617346));
#35371=CARTESIAN_POINT('Ctrl Pts',(-4.71371668580301,-74.0780191071452,
8.16439679232994));
#35372=CARTESIAN_POINT('Ctrl Pts',(1.47018674401621E-11,-73.9030191071452,
8.16439679232146));
#35373=CARTESIAN_POINT('Ctrl Pts',(4.71371668583241,-73.7280191071452,8.16439679231297));
#35374=CARTESIAN_POINT('Ctrl Pts',(7.07057502873392,-73.5530191071451,4.082198396148));
#35375=CARTESIAN_POINT('Ctrl Pts',(9.42743337163542,-73.3780191071452,-1.69756769845304E-11));
#35376=CARTESIAN_POINT('Ctrl Pts',(7.07057502871922,-73.2030191071452,-4.08219839617346));
#35377=CARTESIAN_POINT('Ctrl Pts',(4.71371668580301,-73.0280191071452,-8.16439679232994));
#35378=CARTESIAN_POINT('Ctrl Pts',(-1.4702867290402E-11,-72.8530191071452,
-8.16439679232146));
#35379=CARTESIAN_POINT('Ctrl Pts',(-4.71371668583241,-72.6780191071452,
-8.16439679231297));
#35380=CARTESIAN_POINT('Ctrl Pts',(-7.07057502873392,-72.5030191071451,
-4.082198396148));
#35381=CARTESIAN_POINT('Ctrl Pts',(-9.42743337163542,-72.3280191071452,
1.69768315121407E-11));
#35382=CARTESIAN_POINT('Ctrl Pts',(-7.07057502871922,-72.1530191071452,
4.08219839617346));
#35383=CARTESIAN_POINT('Ctrl Pts',(-4.71371668580301,-71.9780191071451,
8.16439679232994));
#35384=CARTESIAN_POINT('Ctrl Pts',(1.47018674401621E-11,-71.8030191071452,
8.16439679232146));
#35385=CARTESIAN_POINT('Ctrl Pts',(4.71371668583241,-71.6280191071452,8.16439679231297));
#35386=CARTESIAN_POINT('Ctrl Pts',(7.07057502873392,-71.4530191071452,4.082198396148));
#35387=CARTESIAN_POINT('Ctrl Pts',(9.42743337163542,-71.2780191071452,-1.69756769845304E-11));
#35388=CARTESIAN_POINT('Ctrl Pts',(7.07057502871922,-71.1030191071452,-4.08219839617346));
#35389=CARTESIAN_POINT('Ctrl Pts',(4.71371668580301,-70.9280191071451,-8.16439679232994));
#35390=CARTESIAN_POINT('Ctrl Pts',(-1.4702867290402E-11,-70.7530191071451,
-8.16439679232146));
#35391=CARTESIAN_POINT('Ctrl Pts',(-4.71371668583241,-70.5780191071452,
-8.16439679231297));
#35392=CARTESIAN_POINT('Ctrl Pts',(-7.07057502873392,-70.4030191071452,
-4.082198396148));
#35393=CARTESIAN_POINT('Ctrl Pts',(-9.42743337163542,-70.2280191071452,
1.69768315121407E-11));
#35394=CARTESIAN_POINT('Ctrl Pts',(-7.07057502871922,-70.0530191071452,
4.08219839617346));
#35395=CARTESIAN_POINT('Ctrl Pts',(-4.71371668580301,-69.8780191071452,
8.16439679232994));
#35396=CARTESIAN_POINT('Ctrl Pts',(1.47018674401621E-11,-69.7030191071452,
8.16439679232146));
#35397=CARTESIAN_POINT('Ctrl Pts',(4.71371668583241,-69.5280191071452,8.16439679231297));
#35398=CARTESIAN_POINT('Ctrl Pts',(7.07057502873392,-69.3530191071452,4.082198396148));
#35399=CARTESIAN_POINT('Ctrl Pts',(9.42743337163542,-69.1780191071452,-1.69756769845304E-11));
#35400=CARTESIAN_POINT('Ctrl Pts',(7.07057502871922,-69.0030191071452,-4.08219839617346));
#35401=CARTESIAN_POINT('Ctrl Pts',(4.71371668580301,-68.8280191071452,-8.16439679232994));
#35402=CARTESIAN_POINT('Ctrl Pts',(-1.4702867290402E-11,-68.6530191071452,
-8.16439679232146));
#35403=CARTESIAN_POINT('Ctrl Pts',(-4.71371668583241,-68.4780191071452,
-8.16439679231297));
#35404=CARTESIAN_POINT('Ctrl Pts',(-7.07057502873392,-68.3030191071452,
-4.082198396148));
#35405=CARTESIAN_POINT('Ctrl Pts',(-9.42743337163542,-68.1280191071452,
1.69768315121407E-11));
#35406=CARTESIAN_POINT('Ctrl Pts',(-7.07057502871922,-67.9530191071452,
4.08219839617346));
#35407=CARTESIAN_POINT('Ctrl Pts',(-4.71371668580301,-67.7780191071452,
8.16439679232994));
#35408=CARTESIAN_POINT('Ctrl Pts',(1.47018674401621E-11,-67.6030191071452,
8.16439679232146));
#35409=CARTESIAN_POINT('Ctrl Pts',(4.71371668583241,-67.4280191071452,8.16439679231297));
#35410=CARTESIAN_POINT('Ctrl Pts',(7.07057502873392,-67.2530191071452,4.082198396148));
#35411=CARTESIAN_POINT('Ctrl Pts',(9.42743337163542,-67.0780191071452,-1.69756769845304E-11));
#35412=CARTESIAN_POINT('Ctrl Pts',(7.07057502871922,-66.9030191071452,-4.08219839617346));
#35413=CARTESIAN_POINT('Ctrl Pts',(4.71371668580301,-66.7280191071452,-8.16439679232994));
#35414=CARTESIAN_POINT('Ctrl Pts',(-1.4702867290402E-11,-66.5530191071452,
-8.16439679232146));
#35415=CARTESIAN_POINT('Ctrl Pts',(-4.71371668583241,-66.3780191071452,
-8.16439679231297));
#35416=CARTESIAN_POINT('Ctrl Pts',(-7.07057502873392,-66.2030191071452,
-4.082198396148));
#35417=CARTESIAN_POINT('Ctrl Pts',(-9.42743337163542,-66.0280191071452,
1.69768315121407E-11));
#35418=CARTESIAN_POINT('Ctrl Pts',(-7.07057502871922,-65.8530191071452,
4.08219839617346));
#35419=CARTESIAN_POINT('Ctrl Pts',(-4.71371668580301,-65.6780191071452,
8.16439679232994));
#35420=CARTESIAN_POINT('Ctrl Pts',(1.47018674401621E-11,-65.5030191071452,
8.16439679232146));
#35421=CARTESIAN_POINT('Ctrl Pts',(4.71371668583241,-65.3280191071452,8.16439679231297));
#35422=CARTESIAN_POINT('Ctrl Pts',(7.07057502873392,-65.1530191071452,4.082198396148));
#35423=CARTESIAN_POINT('Ctrl Pts',(9.42743337163542,-64.9780191071452,-1.69756769845304E-11));
#35424=CARTESIAN_POINT('Ctrl Pts',(7.07057502871922,-64.8030191071452,-4.08219839617346));
#35425=CARTESIAN_POINT('Ctrl Pts',(4.71371668580301,-64.6280191071452,-8.16439679232994));
#35426=CARTESIAN_POINT('Ctrl Pts',(-1.4702867290402E-11,-64.4530191071452,
-8.16439679232146));
#35427=CARTESIAN_POINT('Ctrl Pts',(-4.71371668583241,-64.2780191071452,
-8.16439679231297));
#35428=CARTESIAN_POINT('Ctrl Pts',(-7.07057502873392,-64.1030191071452,
-4.082198396148));
#35429=CARTESIAN_POINT('Ctrl Pts',(-9.42743337163542,-63.9280191071452,
1.69768315121407E-11));
#35430=CARTESIAN_POINT('Ctrl Pts',(-7.07057502871922,-63.7530191071452,
4.08219839617346));
#35431=CARTESIAN_POINT('Ctrl Pts',(-4.71371668580301,-63.5780191071452,
8.16439679232994));
#35432=CARTESIAN_POINT('Ctrl Pts',(1.47018674401621E-11,-63.4030191071452,
8.16439679232146));
#35433=CARTESIAN_POINT('Ctrl Pts',(4.71371668583241,-63.2280191071452,8.16439679231297));
#35434=CARTESIAN_POINT('Ctrl Pts',(7.07057502873392,-63.0530191071452,4.082198396148));
#35435=CARTESIAN_POINT('Ctrl Pts',(9.42743337163542,-62.8780191071452,-1.69756769845304E-11));
#35436=CARTESIAN_POINT('Ctrl Pts',(7.07057502871922,-62.7030191071452,-4.08219839617346));
#35437=CARTESIAN_POINT('Ctrl Pts',(4.71371668580301,-62.5280191071452,-8.16439679232994));
#35438=CARTESIAN_POINT('Ctrl Pts',(-1.4702867290402E-11,-62.3530191071452,
-8.16439679232146));
#35439=CARTESIAN_POINT('Ctrl Pts',(-4.71371668583241,-62.1780191071452,
-8.16439679231297));
#35440=CARTESIAN_POINT('Ctrl Pts',(-7.07057502873392,-62.0030191071452,
-4.082198396148));
#35441=CARTESIAN_POINT('Ctrl Pts',(-9.42743337163542,-61.8280191071452,
1.69768315121407E-11));
#35442=CARTESIAN_POINT('Ctrl Pts',(-7.07057502871922,-61.6530191071452,
4.08219839617346));
#35443=CARTESIAN_POINT('Ctrl Pts',(-4.71371668580301,-61.4780191071452,
8.16439679232994));
#35444=CARTESIAN_POINT('Ctrl Pts',(1.47018674401621E-11,-61.3030191071452,
8.16439679232146));
#35445=CARTESIAN_POINT('Ctrl Pts',(4.71371668583241,-61.1280191071452,8.16439679231297));
#35446=CARTESIAN_POINT('Ctrl Pts',(7.07057502873392,-60.9530191071452,4.082198396148));
#35447=CARTESIAN_POINT('Ctrl Pts',(9.42743337163542,-60.7780191071452,-1.69756769845304E-11));
#35448=CARTESIAN_POINT('Ctrl Pts',(7.07057502871922,-60.6030191071452,-4.08219839617346));
#35449=CARTESIAN_POINT('Ctrl Pts',(4.71371668580301,-60.4280191071452,-8.16439679232994));
#35450=CARTESIAN_POINT('Ctrl Pts',(-1.4702867290402E-11,-60.2530191071452,
-8.16439679232146));
#35451=CARTESIAN_POINT('Ctrl Pts',(-4.71371668583241,-60.0780191071452,
-8.16439679231297));
#35452=CARTESIAN_POINT('Ctrl Pts',(-7.07057502873392,-59.9030191071452,
-4.082198396148));
#35453=CARTESIAN_POINT('Ctrl Pts',(-9.42743337163542,-59.7280191071452,
1.69768315121407E-11));
#35454=CARTESIAN_POINT('Ctrl Pts',(-7.07057502871922,-59.5530191071452,
4.08219839617346));
#35455=CARTESIAN_POINT('Ctrl Pts',(-4.71371668580301,-59.3780191071452,
8.16439679232994));
#35456=CARTESIAN_POINT('Ctrl Pts',(1.47018674401621E-11,-59.2030191071452,
8.16439679232146));
#35457=CARTESIAN_POINT('Ctrl Pts',(4.71371668583241,-59.0280191071452,8.16439679231297));
#35458=CARTESIAN_POINT('Ctrl Pts',(7.07057502873392,-58.8530191071452,4.082198396148));
#35459=CARTESIAN_POINT('Ctrl Pts',(9.42743337163542,-58.6780191071452,-1.69756769845304E-11));
#35460=CARTESIAN_POINT('Ctrl Pts',(7.07057502871922,-58.5030191071452,-4.08219839617346));
#35461=CARTESIAN_POINT('Ctrl Pts',(4.71371668580301,-58.3280191071452,-8.16439679232994));
#35462=CARTESIAN_POINT('Ctrl Pts',(-1.4702867290402E-11,-58.1530191071452,
-8.16439679232146));
#35463=CARTESIAN_POINT('Ctrl Pts',(-4.71371668583241,-57.9780191071452,
-8.16439679231297));
#35464=CARTESIAN_POINT('Ctrl Pts',(-7.07057502873392,-57.8030191071452,
-4.082198396148));
#35465=CARTESIAN_POINT('Ctrl Pts',(-9.42743337163542,-57.6280191071452,
1.69768315121407E-11));
#35466=CARTESIAN_POINT('Ctrl Pts',(-7.07057502871922,-57.4530191071452,
4.08219839617346));
#35467=CARTESIAN_POINT('Ctrl Pts',(-4.71371668580301,-57.2780191071452,
8.16439679232994));
#35468=CARTESIAN_POINT('Ctrl Pts',(1.47018674401621E-11,-57.1030191071452,
8.16439679232146));
#35469=CARTESIAN_POINT('Ctrl Pts',(4.71371668583241,-56.9280191071452,8.16439679231297));
#35470=CARTESIAN_POINT('Ctrl Pts',(7.07057502873392,-56.7530191071452,4.082198396148));
#35471=CARTESIAN_POINT('Ctrl Pts',(9.42743337163542,-56.5780191071452,-1.69756769845304E-11));
#35472=CARTESIAN_POINT('Ctrl Pts',(7.07057502871922,-56.4030191071452,-4.08219839617346));
#35473=CARTESIAN_POINT('Ctrl Pts',(4.71371668580301,-56.2280191071452,-8.16439679232994));
#35474=CARTESIAN_POINT('Ctrl Pts',(-1.4702867290402E-11,-56.0530191071452,
-8.16439679232146));
#35475=CARTESIAN_POINT('Ctrl Pts',(-4.71371668583241,-55.8780191071452,
-8.16439679231297));
#35476=CARTESIAN_POINT('Ctrl Pts',(-7.07057502873392,-55.7030191071452,
-4.082198396148));
#35477=CARTESIAN_POINT('Ctrl Pts',(-9.42743337163542,-55.5280191071452,
1.69768315121407E-11));
#35478=CARTESIAN_POINT('Ctrl Pts',(-7.07057502871922,-55.3530191071452,
4.08219839617346));
#35479=CARTESIAN_POINT('Ctrl Pts',(-4.71371668580301,-55.1780191071452,
8.16439679232994));
#35480=CARTESIAN_POINT('Ctrl Pts',(1.47018674401621E-11,-55.0030191071452,
8.16439679232146));
#35481=CARTESIAN_POINT('Ctrl Pts',(4.71371668583241,-54.8280191071452,8.16439679231297));
#35482=CARTESIAN_POINT('Ctrl Pts',(7.07057502873392,-54.6530191071452,4.082198396148));
#35483=CARTESIAN_POINT('Ctrl Pts',(9.42743337163542,-54.4780191071452,-1.69756769845304E-11));
#35484=CARTESIAN_POINT('Ctrl Pts',(7.07057502871922,-54.3030191071452,-4.08219839617346));
#35485=CARTESIAN_POINT('Ctrl Pts',(4.71371668580301,-54.1280191071452,-8.16439679232994));
#35486=CARTESIAN_POINT('Ctrl Pts',(-1.4702867290402E-11,-53.9530191071452,
-8.16439679232146));
#35487=CARTESIAN_POINT('Ctrl Pts',(-4.71371668583241,-53.7780191071452,
-8.16439679231297));
#35488=CARTESIAN_POINT('Ctrl Pts',(-7.07057502873392,-53.6030191071452,
-4.082198396148));
#35489=CARTESIAN_POINT('Ctrl Pts',(-9.42743337163542,-53.4280191071452,
1.69768315121407E-11));
#35490=CARTESIAN_POINT('Ctrl Pts',(-7.07057502871922,-53.2530191071452,
4.08219839617346));
#35491=CARTESIAN_POINT('Ctrl Pts',(-4.71371668580301,-53.0780191071452,
8.16439679232994));
#35492=CARTESIAN_POINT('Ctrl Pts',(1.47018674401621E-11,-52.9030191071452,
8.16439679232146));
#35493=CARTESIAN_POINT('Ctrl Pts',(4.71371668583241,-52.7280191071452,8.16439679231297));
#35494=CARTESIAN_POINT('Ctrl Pts',(7.07057502873392,-52.5530191071452,4.082198396148));
#35495=CARTESIAN_POINT('Ctrl Pts',(9.42743337163542,-52.3780191071452,-1.69756769845304E-11));
#35496=CARTESIAN_POINT('Ctrl Pts',(7.07057502871922,-52.2030191071452,-4.08219839617346));
#35497=CARTESIAN_POINT('Ctrl Pts',(4.71371668580301,-52.0280191071452,-8.16439679232994));
#35498=CARTESIAN_POINT('Ctrl Pts',(-1.4702867290402E-11,-51.8530191071452,
-8.16439679232146));
#35499=CARTESIAN_POINT('Ctrl Pts',(-4.71371668583241,-51.6780191071452,
-8.16439679231297));
#35500=CARTESIAN_POINT('Ctrl Pts',(-7.07057502873392,-51.5030191071452,
-4.082198396148));
#35501=CARTESIAN_POINT('Ctrl Pts',(-9.42743337163542,-51.3280191071452,
1.69768315121407E-11));
#35502=CARTESIAN_POINT('Ctrl Pts',(-7.07057502871922,-51.1530191071452,
4.08219839617346));
#35503=CARTESIAN_POINT('Ctrl Pts',(-4.71371668580301,-50.9780191071452,
8.16439679232994));
#35504=CARTESIAN_POINT('Ctrl Pts',(1.47018674401621E-11,-50.8030191071452,
8.16439679232146));
#35505=CARTESIAN_POINT('Ctrl Pts',(4.71371668583241,-50.6280191071452,8.16439679231297));
#35506=CARTESIAN_POINT('Ctrl Pts',(7.07057502873392,-50.4530191071452,4.082198396148));
#35507=CARTESIAN_POINT('Ctrl Pts',(9.42743337163542,-50.2780191071452,-1.69756769845304E-11));
#35508=CARTESIAN_POINT('Ctrl Pts',(7.07057502871922,-50.1030191071452,-4.08219839617346));
#35509=CARTESIAN_POINT('Ctrl Pts',(4.71371668580301,-49.9280191071452,-8.16439679232994));
#35510=CARTESIAN_POINT('Ctrl Pts',(-1.4702867290402E-11,-49.7530191071452,
-8.16439679232146));
#35511=CARTESIAN_POINT('Ctrl Pts',(-4.71371668583241,-49.5780191071452,
-8.16439679231297));
#35512=CARTESIAN_POINT('Ctrl Pts',(-7.07057502873392,-49.4030191071452,
-4.082198396148));
#35513=CARTESIAN_POINT('Ctrl Pts',(-9.42743337163542,-49.2280191071452,
1.69768315121407E-11));
#35514=CARTESIAN_POINT('Ctrl Pts',(-7.07057502871922,-49.0530191071452,
4.08219839617346));
#35515=CARTESIAN_POINT('Ctrl Pts',(-4.71371668580301,-48.8780191071452,
8.16439679232994));
#35516=CARTESIAN_POINT('Ctrl Pts',(1.47018674401621E-11,-48.7030191071452,
8.16439679232146));
#35517=CARTESIAN_POINT('Ctrl Pts',(4.71371668583241,-48.5280191071452,8.16439679231297));
#35518=CARTESIAN_POINT('Ctrl Pts',(7.07057502873392,-48.3530191071452,4.082198396148));
#35519=CARTESIAN_POINT('Ctrl Pts',(9.42743337163542,-48.1780191071452,-1.69756769845304E-11));
#35520=CARTESIAN_POINT('Ctrl Pts',(7.07057502871922,-48.0030191071452,-4.08219839617346));
#35521=CARTESIAN_POINT('Ctrl Pts',(4.71371668580301,-47.8280191071452,-8.16439679232994));
#35522=CARTESIAN_POINT('Ctrl Pts',(-1.4702867290402E-11,-47.6530191071452,
-8.16439679232146));
#35523=CARTESIAN_POINT('Ctrl Pts',(-4.71371668583241,-47.4780191071452,
-8.16439679231297));
#35524=CARTESIAN_POINT('Ctrl Pts',(-7.07057502873392,-47.3030191071452,
-4.082198396148));
#35525=CARTESIAN_POINT('Ctrl Pts',(-9.42743337163542,-47.1280191071452,
1.69768315121407E-11));
#35526=CARTESIAN_POINT('Ctrl Pts',(-7.07057502871922,-46.9530191071452,
4.08219839617346));
#35527=CARTESIAN_POINT('Ctrl Pts',(-4.71371668580301,-46.7780191071452,
8.16439679232994));
#35528=CARTESIAN_POINT('Ctrl Pts',(1.47018674401621E-11,-46.6030191071452,
8.16439679232146));
#35529=CARTESIAN_POINT('Ctrl Pts',(4.71371668583241,-46.4280191071452,8.16439679231297));
#35530=CARTESIAN_POINT('Ctrl Pts',(7.07057502873392,-46.2530191071452,4.082198396148));
#35531=CARTESIAN_POINT('Ctrl Pts',(9.42743337163542,-46.0780191071452,-1.69756769845304E-11));
#35532=CARTESIAN_POINT('Ctrl Pts',(7.07057502871922,-45.9030191071452,-4.08219839617346));
#35533=CARTESIAN_POINT('Ctrl Pts',(4.71371668580301,-45.7280191071452,-8.16439679232994));
#35534=CARTESIAN_POINT('Ctrl Pts',(-1.4702867290402E-11,-45.5530191071452,
-8.16439679232146));
#35535=CARTESIAN_POINT('Ctrl Pts',(-4.71371668583241,-45.3780191071452,
-8.16439679231297));
#35536=CARTESIAN_POINT('Ctrl Pts',(-7.07057502873392,-45.2030191071452,
-4.082198396148));
#35537=CARTESIAN_POINT('Ctrl Pts',(-9.42743337163542,-45.0280191071452,
1.69768315121407E-11));
#35538=CARTESIAN_POINT('Ctrl Pts',(-7.07057502871922,-44.8530191071452,
4.08219839617346));
#35539=CARTESIAN_POINT('Ctrl Pts',(-4.71371668580301,-44.6780191071452,
8.16439679232994));
#35540=CARTESIAN_POINT('Ctrl Pts',(1.47018674401621E-11,-44.5030191071452,
8.16439679232146));
#35541=CARTESIAN_POINT('Ctrl Pts',(4.71371668583241,-44.3280191071452,8.16439679231297));
#35542=CARTESIAN_POINT('Ctrl Pts',(7.07057502873392,-44.1530191071452,4.082198396148));
#35543=CARTESIAN_POINT('Ctrl Pts',(9.42743337163542,-43.9780191071452,-1.69756769845304E-11));
#35544=CARTESIAN_POINT('Ctrl Pts',(7.07057502871922,-43.8030191071452,-4.08219839617346));
#35545=CARTESIAN_POINT('Ctrl Pts',(4.71371668580301,-43.6280191071452,-8.16439679232994));
#35546=CARTESIAN_POINT('Ctrl Pts',(-1.4702867290402E-11,-43.4530191071452,
-8.16439679232146));
#35547=CARTESIAN_POINT('Ctrl Pts',(-1.51301075899711E-11,-213.429517970998,
-8.40164026751963));
#35548=CARTESIAN_POINT('Ctrl Pts',(-4.85068927010199,-213.254517970998,
-8.4016402675109));
#35549=CARTESIAN_POINT('Ctrl Pts',(-7.27603390513785,-213.079517970998,
-4.20082013374671));
#35550=CARTESIAN_POINT('Ctrl Pts',(-9.70137854017372,-212.904517970998,
1.74701493417668E-11));
#35551=CARTESIAN_POINT('Ctrl Pts',(-7.27603390512272,-212.729517970998,
4.20082013377292));
#35552=CARTESIAN_POINT('Ctrl Pts',(-4.85068927007173,-212.554517970998,
8.40164026752836));
#35553=CARTESIAN_POINT('Ctrl Pts',(1.5129078685785E-11,-212.379517970998,
8.40164026751963));
#35554=CARTESIAN_POINT('Ctrl Pts',(4.85068927010198,-212.204517970998,8.4016402675109));
#35555=CARTESIAN_POINT('Ctrl Pts',(7.27603390513785,-212.029517970998,4.20082013374672));
#35556=CARTESIAN_POINT('Ctrl Pts',(9.70137854017372,-211.854517970998,-1.74689612655491E-11));
#35557=CARTESIAN_POINT('Ctrl Pts',(7.27603390512273,-211.679517970998,-4.20082013377291));
#35558=CARTESIAN_POINT('Ctrl Pts',(4.85068927007173,-211.504517970998,-8.40164026752836));
#35559=CARTESIAN_POINT('Ctrl Pts',(-1.51301075899711E-11,-211.329517970998,
-8.40164026751963));
#35560=CARTESIAN_POINT('Ctrl Pts',(-4.85068927010199,-211.154517970998,
-8.4016402675109));
#35561=CARTESIAN_POINT('Ctrl Pts',(-7.27603390513785,-210.979517970998,
-4.20082013374671));
#35562=CARTESIAN_POINT('Ctrl Pts',(-9.70137854017372,-210.804517970998,
1.74701493417668E-11));
#35563=CARTESIAN_POINT('Ctrl Pts',(-7.27603390512272,-210.629517970998,
4.20082013377292));
#35564=CARTESIAN_POINT('Ctrl Pts',(-4.85068927007173,-210.454517970998,
8.40164026752836));
#35565=CARTESIAN_POINT('Ctrl Pts',(1.5129078685785E-11,-210.279517970998,
8.40164026751963));
#35566=CARTESIAN_POINT('Ctrl Pts',(4.85068927010198,-210.104517970998,8.4016402675109));
#35567=CARTESIAN_POINT('Ctrl Pts',(7.27603390513785,-209.929517970998,4.20082013374672));
#35568=CARTESIAN_POINT('Ctrl Pts',(9.70137854017372,-209.754517970998,-1.74689612655491E-11));
#35569=CARTESIAN_POINT('Ctrl Pts',(7.27603390512273,-209.579517970998,-4.20082013377291));
#35570=CARTESIAN_POINT('Ctrl Pts',(4.85068927007173,-209.404517970998,-8.40164026752836));
#35571=CARTESIAN_POINT('Ctrl Pts',(-1.51301075899711E-11,-209.229517970998,
-8.40164026751963));
#35572=CARTESIAN_POINT('Ctrl Pts',(-4.85068927010199,-209.054517970998,
-8.4016402675109));
#35573=CARTESIAN_POINT('Ctrl Pts',(-7.27603390513785,-208.879517970998,
-4.20082013374671));
#35574=CARTESIAN_POINT('Ctrl Pts',(-9.70137854017372,-208.704517970998,
1.74701493417668E-11));
#35575=CARTESIAN_POINT('Ctrl Pts',(-7.27603390512272,-208.529517970998,
4.20082013377292));
#35576=CARTESIAN_POINT('Ctrl Pts',(-4.85068927007173,-208.354517970998,
8.40164026752836));
#35577=CARTESIAN_POINT('Ctrl Pts',(1.5129078685785E-11,-208.179517970998,
8.40164026751963));
#35578=CARTESIAN_POINT('Ctrl Pts',(4.85068927010198,-208.004517970998,8.4016402675109));
#35579=CARTESIAN_POINT('Ctrl Pts',(7.27603390513785,-207.829517970998,4.20082013374672));
#35580=CARTESIAN_POINT('Ctrl Pts',(9.70137854017372,-207.654517970998,-1.74689612655491E-11));
#35581=CARTESIAN_POINT('Ctrl Pts',(7.27603390512273,-207.479517970998,-4.20082013377291));
#35582=CARTESIAN_POINT('Ctrl Pts',(4.85068927007173,-207.304517970998,-8.40164026752836));
#35583=CARTESIAN_POINT('Ctrl Pts',(-1.51301075899711E-11,-207.129517970998,
-8.40164026751963));
#35584=CARTESIAN_POINT('Ctrl Pts',(-4.85068927010199,-206.954517970998,
-8.4016402675109));
#35585=CARTESIAN_POINT('Ctrl Pts',(-7.27603390513785,-206.779517970998,
-4.20082013374671));
#35586=CARTESIAN_POINT('Ctrl Pts',(-9.70137854017372,-206.604517970998,
1.74701493417668E-11));
#35587=CARTESIAN_POINT('Ctrl Pts',(-7.27603390512272,-206.429517970998,
4.20082013377292));
#35588=CARTESIAN_POINT('Ctrl Pts',(-4.85068927007173,-206.254517970998,
8.40164026752836));
#35589=CARTESIAN_POINT('Ctrl Pts',(1.5129078685785E-11,-206.079517970998,
8.40164026751963));
#35590=CARTESIAN_POINT('Ctrl Pts',(4.85068927010198,-205.904517970998,8.4016402675109));
#35591=CARTESIAN_POINT('Ctrl Pts',(7.27603390513785,-205.729517970998,4.20082013374672));
#35592=CARTESIAN_POINT('Ctrl Pts',(9.70137854017372,-205.554517970998,-1.74689612655491E-11));
#35593=CARTESIAN_POINT('Ctrl Pts',(7.27603390512273,-205.379517970998,-4.20082013377291));
#35594=CARTESIAN_POINT('Ctrl Pts',(4.85068927007173,-205.204517970998,-8.40164026752836));
#35595=CARTESIAN_POINT('Ctrl Pts',(-1.51301075899711E-11,-205.029517970998,
-8.40164026751963));
#35596=CARTESIAN_POINT('Ctrl Pts',(-4.85068927010199,-204.854517970998,
-8.4016402675109));
#35597=CARTESIAN_POINT('Ctrl Pts',(-7.27603390513785,-204.679517970998,
-4.20082013374671));
#35598=CARTESIAN_POINT('Ctrl Pts',(-9.70137854017372,-204.504517970998,
1.74701493417668E-11));
#35599=CARTESIAN_POINT('Ctrl Pts',(-7.27603390512272,-204.329517970998,
4.20082013377292));
#35600=CARTESIAN_POINT('Ctrl Pts',(-4.85068927007173,-204.154517970998,
8.40164026752836));
#35601=CARTESIAN_POINT('Ctrl Pts',(1.5129078685785E-11,-203.979517970998,
8.40164026751963));
#35602=CARTESIAN_POINT('Ctrl Pts',(4.85068927010198,-203.804517970998,8.4016402675109));
#35603=CARTESIAN_POINT('Ctrl Pts',(7.27603390513785,-203.629517970998,4.20082013374672));
#35604=CARTESIAN_POINT('Ctrl Pts',(9.70137854017372,-203.454517970998,-1.74689612655491E-11));
#35605=CARTESIAN_POINT('Ctrl Pts',(7.27603390512273,-203.279517970998,-4.20082013377291));
#35606=CARTESIAN_POINT('Ctrl Pts',(4.85068927007173,-203.104517970998,-8.40164026752836));
#35607=CARTESIAN_POINT('Ctrl Pts',(-1.51301075899711E-11,-202.929517970998,
-8.40164026751963));
#35608=CARTESIAN_POINT('Ctrl Pts',(-4.85068927010199,-202.754517970998,
-8.4016402675109));
#35609=CARTESIAN_POINT('Ctrl Pts',(-7.27603390513785,-202.579517970998,
-4.20082013374671));
#35610=CARTESIAN_POINT('Ctrl Pts',(-9.70137854017372,-202.404517970998,
1.74701493417668E-11));
#35611=CARTESIAN_POINT('Ctrl Pts',(-7.27603390512272,-202.229517970998,
4.20082013377292));
#35612=CARTESIAN_POINT('Ctrl Pts',(-4.85068927007173,-202.054517970998,
8.40164026752836));
#35613=CARTESIAN_POINT('Ctrl Pts',(1.5129078685785E-11,-201.879517970998,
8.40164026751963));
#35614=CARTESIAN_POINT('Ctrl Pts',(4.85068927010198,-201.704517970998,8.4016402675109));
#35615=CARTESIAN_POINT('Ctrl Pts',(7.27603390513785,-201.529517970998,4.20082013374672));
#35616=CARTESIAN_POINT('Ctrl Pts',(9.70137854017372,-201.354517970998,-1.74689612655491E-11));
#35617=CARTESIAN_POINT('Ctrl Pts',(7.27603390512273,-201.179517970998,-4.20082013377291));
#35618=CARTESIAN_POINT('Ctrl Pts',(4.85068927007173,-201.004517970998,-8.40164026752836));
#35619=CARTESIAN_POINT('Ctrl Pts',(-1.51301075899711E-11,-200.829517970998,
-8.40164026751963));
#35620=CARTESIAN_POINT('Ctrl Pts',(-4.85068927010199,-200.654517970998,
-8.4016402675109));
#35621=CARTESIAN_POINT('Ctrl Pts',(-7.27603390513785,-200.479517970998,
-4.20082013374671));
#35622=CARTESIAN_POINT('Ctrl Pts',(-9.70137854017372,-200.304517970998,
1.74701493417668E-11));
#35623=CARTESIAN_POINT('Ctrl Pts',(-7.27603390512272,-200.129517970998,
4.20082013377292));
#35624=CARTESIAN_POINT('Ctrl Pts',(-4.85068927007173,-199.954517970998,
8.40164026752836));
#35625=CARTESIAN_POINT('Ctrl Pts',(1.5129078685785E-11,-199.779517970998,
8.40164026751963));
#35626=CARTESIAN_POINT('Ctrl Pts',(4.85068927010198,-199.604517970998,8.4016402675109));
#35627=CARTESIAN_POINT('Ctrl Pts',(7.27603390513785,-199.429517970998,4.20082013374672));
#35628=CARTESIAN_POINT('Ctrl Pts',(9.70137854017372,-199.254517970998,-1.74689612655491E-11));
#35629=CARTESIAN_POINT('Ctrl Pts',(7.27603390512273,-199.079517970998,-4.20082013377291));
#35630=CARTESIAN_POINT('Ctrl Pts',(4.85068927007173,-198.904517970998,-8.40164026752836));
#35631=CARTESIAN_POINT('Ctrl Pts',(-1.51301075899711E-11,-198.729517970998,
-8.40164026751963));
#35632=CARTESIAN_POINT('Ctrl Pts',(-4.85068927010199,-198.554517970998,
-8.4016402675109));
#35633=CARTESIAN_POINT('Ctrl Pts',(-7.27603390513785,-198.379517970998,
-4.20082013374671));
#35634=CARTESIAN_POINT('Ctrl Pts',(-9.70137854017372,-198.204517970998,
1.74701493417668E-11));
#35635=CARTESIAN_POINT('Ctrl Pts',(-7.27603390512272,-198.029517970998,
4.20082013377292));
#35636=CARTESIAN_POINT('Ctrl Pts',(-4.85068927007173,-197.854517970998,
8.40164026752836));
#35637=CARTESIAN_POINT('Ctrl Pts',(1.5129078685785E-11,-197.679517970998,
8.40164026751963));
#35638=CARTESIAN_POINT('Ctrl Pts',(4.85068927010198,-197.504517970998,8.4016402675109));
#35639=CARTESIAN_POINT('Ctrl Pts',(7.27603390513785,-197.329517970998,4.20082013374672));
#35640=CARTESIAN_POINT('Ctrl Pts',(9.70137854017372,-197.154517970998,-1.74689612655491E-11));
#35641=CARTESIAN_POINT('Ctrl Pts',(7.27603390512273,-196.979517970998,-4.20082013377291));
#35642=CARTESIAN_POINT('Ctrl Pts',(4.85068927007173,-196.804517970998,-8.40164026752836));
#35643=CARTESIAN_POINT('Ctrl Pts',(-1.51301075899711E-11,-196.629517970998,
-8.40164026751963));
#35644=CARTESIAN_POINT('Ctrl Pts',(-4.85068927010199,-196.454517970998,
-8.4016402675109));
#35645=CARTESIAN_POINT('Ctrl Pts',(-7.27603390513785,-196.279517970998,
-4.20082013374671));
#35646=CARTESIAN_POINT('Ctrl Pts',(-9.70137854017372,-196.104517970998,
1.74701493417668E-11));
#35647=CARTESIAN_POINT('Ctrl Pts',(-7.27603390512272,-195.929517970998,
4.20082013377292));
#35648=CARTESIAN_POINT('Ctrl Pts',(-4.85068927007173,-195.754517970998,
8.40164026752836));
#35649=CARTESIAN_POINT('Ctrl Pts',(1.5129078685785E-11,-195.579517970998,
8.40164026751963));
#35650=CARTESIAN_POINT('Ctrl Pts',(4.85068927010198,-195.404517970998,8.4016402675109));
#35651=CARTESIAN_POINT('Ctrl Pts',(7.27603390513785,-195.229517970998,4.20082013374672));
#35652=CARTESIAN_POINT('Ctrl Pts',(9.70137854017372,-195.054517970998,-1.74689612655491E-11));
#35653=CARTESIAN_POINT('Ctrl Pts',(7.27603390512273,-194.879517970998,-4.20082013377291));
#35654=CARTESIAN_POINT('Ctrl Pts',(4.85068927007173,-194.704517970998,-8.40164026752836));
#35655=CARTESIAN_POINT('Ctrl Pts',(-1.51301075899711E-11,-194.529517970998,
-8.40164026751963));
#35656=CARTESIAN_POINT('Ctrl Pts',(-4.85068927010199,-194.354517970998,
-8.4016402675109));
#35657=CARTESIAN_POINT('Ctrl Pts',(-7.27603390513785,-194.179517970998,
-4.20082013374671));
#35658=CARTESIAN_POINT('Ctrl Pts',(-9.70137854017372,-194.004517970998,
1.74701493417668E-11));
#35659=CARTESIAN_POINT('Ctrl Pts',(-7.27603390512272,-193.829517970998,
4.20082013377292));
#35660=CARTESIAN_POINT('Ctrl Pts',(-4.85068927007173,-193.654517970998,
8.40164026752836));
#35661=CARTESIAN_POINT('Ctrl Pts',(1.5129078685785E-11,-193.479517970998,
8.40164026751963));
#35662=CARTESIAN_POINT('Ctrl Pts',(4.85068927010198,-193.304517970998,8.4016402675109));
#35663=CARTESIAN_POINT('Ctrl Pts',(7.27603390513785,-193.129517970998,4.20082013374672));
#35664=CARTESIAN_POINT('Ctrl Pts',(9.70137854017372,-192.954517970998,-1.74689612655491E-11));
#35665=CARTESIAN_POINT('Ctrl Pts',(7.27603390512273,-192.779517970998,-4.20082013377291));
#35666=CARTESIAN_POINT('Ctrl Pts',(4.85068927007173,-192.604517970998,-8.40164026752836));
#35667=CARTESIAN_POINT('Ctrl Pts',(-1.51301075899711E-11,-192.429517970998,
-8.40164026751963));
#35668=CARTESIAN_POINT('Ctrl Pts',(-4.85068927010199,-192.254517970998,
-8.4016402675109));
#35669=CARTESIAN_POINT('Ctrl Pts',(-7.27603390513785,-192.079517970998,
-4.20082013374671));
#35670=CARTESIAN_POINT('Ctrl Pts',(-9.70137854017372,-191.904517970998,
1.74701493417668E-11));
#35671=CARTESIAN_POINT('Ctrl Pts',(-7.27603390512272,-191.729517970998,
4.20082013377292));
#35672=CARTESIAN_POINT('Ctrl Pts',(-4.85068927007173,-191.554517970998,
8.40164026752836));
#35673=CARTESIAN_POINT('Ctrl Pts',(1.5129078685785E-11,-191.379517970998,
8.40164026751963));
#35674=CARTESIAN_POINT('Ctrl Pts',(4.85068927010198,-191.204517970998,8.4016402675109));
#35675=CARTESIAN_POINT('Ctrl Pts',(7.27603390513785,-191.029517970998,4.20082013374672));
#35676=CARTESIAN_POINT('Ctrl Pts',(9.70137854017372,-190.854517970998,-1.74689612655491E-11));
#35677=CARTESIAN_POINT('Ctrl Pts',(7.27603390512273,-190.679517970998,-4.20082013377291));
#35678=CARTESIAN_POINT('Ctrl Pts',(4.85068927007173,-190.504517970998,-8.40164026752836));
#35679=CARTESIAN_POINT('Ctrl Pts',(-1.51301075899711E-11,-190.329517970998,
-8.40164026751963));
#35680=CARTESIAN_POINT('Ctrl Pts',(-4.85068927010199,-190.154517970998,
-8.4016402675109));
#35681=CARTESIAN_POINT('Ctrl Pts',(-7.27603390513785,-189.979517970998,
-4.20082013374671));
#35682=CARTESIAN_POINT('Ctrl Pts',(-9.70137854017372,-189.804517970998,
1.74701493417668E-11));
#35683=CARTESIAN_POINT('Ctrl Pts',(-7.27603390512272,-189.629517970998,
4.20082013377292));
#35684=CARTESIAN_POINT('Ctrl Pts',(-4.85068927007173,-189.454517970998,
8.40164026752836));
#35685=CARTESIAN_POINT('Ctrl Pts',(1.5129078685785E-11,-189.279517970998,
8.40164026751963));
#35686=CARTESIAN_POINT('Ctrl Pts',(4.85068927010198,-189.104517970998,8.4016402675109));
#35687=CARTESIAN_POINT('Ctrl Pts',(7.27603390513785,-188.929517970998,4.20082013374672));
#35688=CARTESIAN_POINT('Ctrl Pts',(9.70137854017372,-188.754517970998,-1.74689612655491E-11));
#35689=CARTESIAN_POINT('Ctrl Pts',(7.27603390512273,-188.579517970998,-4.20082013377291));
#35690=CARTESIAN_POINT('Ctrl Pts',(4.85068927007173,-188.404517970998,-8.40164026752836));
#35691=CARTESIAN_POINT('Ctrl Pts',(-1.51301075899711E-11,-188.229517970998,
-8.40164026751963));
#35692=CARTESIAN_POINT('Ctrl Pts',(-4.85068927010199,-188.054517970998,
-8.4016402675109));
#35693=CARTESIAN_POINT('Ctrl Pts',(-7.27603390513785,-187.879517970998,
-4.20082013374671));
#35694=CARTESIAN_POINT('Ctrl Pts',(-9.70137854017372,-187.704517970998,
1.74701493417668E-11));
#35695=CARTESIAN_POINT('Ctrl Pts',(-7.27603390512272,-187.529517970998,
4.20082013377292));
#35696=CARTESIAN_POINT('Ctrl Pts',(-4.85068927007173,-187.354517970998,
8.40164026752836));
#35697=CARTESIAN_POINT('Ctrl Pts',(1.5129078685785E-11,-187.179517970998,
8.40164026751963));
#35698=CARTESIAN_POINT('Ctrl Pts',(4.85068927010198,-187.004517970998,8.4016402675109));
#35699=CARTESIAN_POINT('Ctrl Pts',(7.27603390513785,-186.829517970998,4.20082013374672));
#35700=CARTESIAN_POINT('Ctrl Pts',(9.70137854017372,-186.654517970998,-1.74689612655491E-11));
#35701=CARTESIAN_POINT('Ctrl Pts',(7.27603390512273,-186.479517970998,-4.20082013377291));
#35702=CARTESIAN_POINT('Ctrl Pts',(4.85068927007173,-186.304517970998,-8.40164026752836));
#35703=CARTESIAN_POINT('Ctrl Pts',(-1.51301075899711E-11,-186.129517970998,
-8.40164026751963));
#35704=CARTESIAN_POINT('Ctrl Pts',(-4.85068927010199,-185.954517970998,
-8.4016402675109));
#35705=CARTESIAN_POINT('Ctrl Pts',(-7.27603390513785,-185.779517970998,
-4.20082013374671));
#35706=CARTESIAN_POINT('Ctrl Pts',(-9.70137854017372,-185.604517970998,
1.74701493417668E-11));
#35707=CARTESIAN_POINT('Ctrl Pts',(-7.27603390512272,-185.429517970998,
4.20082013377292));
#35708=CARTESIAN_POINT('Ctrl Pts',(-4.85068927007173,-185.254517970998,
8.40164026752836));
#35709=CARTESIAN_POINT('Ctrl Pts',(1.5129078685785E-11,-185.079517970998,
8.40164026751963));
#35710=CARTESIAN_POINT('Ctrl Pts',(4.85068927010198,-184.904517970998,8.4016402675109));
#35711=CARTESIAN_POINT('Ctrl Pts',(7.27603390513785,-184.729517970998,4.20082013374672));
#35712=CARTESIAN_POINT('Ctrl Pts',(9.70137854017372,-184.554517970998,-1.74689612655491E-11));
#35713=CARTESIAN_POINT('Ctrl Pts',(7.27603390512273,-184.379517970998,-4.20082013377291));
#35714=CARTESIAN_POINT('Ctrl Pts',(4.85068927007173,-184.204517970998,-8.40164026752836));
#35715=CARTESIAN_POINT('Ctrl Pts',(-1.51301075899711E-11,-184.029517970998,
-8.40164026751963));
#35716=CARTESIAN_POINT('Ctrl Pts',(-4.85068927010199,-183.854517970998,
-8.4016402675109));
#35717=CARTESIAN_POINT('Ctrl Pts',(-7.27603390513785,-183.679517970998,
-4.20082013374671));
#35718=CARTESIAN_POINT('Ctrl Pts',(-9.70137854017372,-183.504517970998,
1.74701493417668E-11));
#35719=CARTESIAN_POINT('Ctrl Pts',(-7.27603390512272,-183.329517970998,
4.20082013377292));
#35720=CARTESIAN_POINT('Ctrl Pts',(-4.85068927007173,-183.154517970998,
8.40164026752836));
#35721=CARTESIAN_POINT('Ctrl Pts',(1.5129078685785E-11,-182.979517970998,
8.40164026751963));
#35722=CARTESIAN_POINT('Ctrl Pts',(4.85068927010198,-182.804517970998,8.4016402675109));
#35723=CARTESIAN_POINT('Ctrl Pts',(7.27603390513785,-182.629517970998,4.20082013374672));
#35724=CARTESIAN_POINT('Ctrl Pts',(9.70137854017372,-182.454517970998,-1.74689612655491E-11));
#35725=CARTESIAN_POINT('Ctrl Pts',(7.27603390512273,-182.279517970998,-4.20082013377291));
#35726=CARTESIAN_POINT('Ctrl Pts',(4.85068927007173,-182.104517970998,-8.40164026752836));
#35727=CARTESIAN_POINT('Ctrl Pts',(-1.51301075899711E-11,-181.929517970998,
-8.40164026751963));
#35728=CARTESIAN_POINT('Ctrl Pts',(-4.85068927010199,-181.754517970998,
-8.4016402675109));
#35729=CARTESIAN_POINT('Ctrl Pts',(-7.27603390513785,-181.579517970998,
-4.20082013374671));
#35730=CARTESIAN_POINT('Ctrl Pts',(-9.70137854017372,-181.404517970998,
1.74701493417668E-11));
#35731=CARTESIAN_POINT('Ctrl Pts',(-7.27603390512272,-181.229517970998,
4.20082013377292));
#35732=CARTESIAN_POINT('Ctrl Pts',(-4.85068927007173,-181.054517970998,
8.40164026752836));
#35733=CARTESIAN_POINT('Ctrl Pts',(1.5129078685785E-11,-180.879517970998,
8.40164026751963));
#35734=CARTESIAN_POINT('Ctrl Pts',(4.85068927010198,-180.704517970998,8.4016402675109));
#35735=CARTESIAN_POINT('Ctrl Pts',(7.27603390513785,-180.529517970998,4.20082013374672));
#35736=CARTESIAN_POINT('Ctrl Pts',(9.70137854017372,-180.354517970998,-1.74689612655491E-11));
#35737=CARTESIAN_POINT('Ctrl Pts',(7.27603390512273,-180.179517970998,-4.20082013377291));
#35738=CARTESIAN_POINT('Ctrl Pts',(4.85068927007173,-180.004517970998,-8.40164026752836));
#35739=CARTESIAN_POINT('Ctrl Pts',(-1.51301075899711E-11,-179.829517970998,
-8.40164026751963));
#35740=CARTESIAN_POINT('Ctrl Pts',(-4.85068927010199,-179.654517970998,
-8.4016402675109));
#35741=CARTESIAN_POINT('Ctrl Pts',(-7.27603390513785,-179.479517970998,
-4.20082013374671));
#35742=CARTESIAN_POINT('Ctrl Pts',(-9.70137854017372,-179.304517970998,
1.74701493417668E-11));
#35743=CARTESIAN_POINT('Ctrl Pts',(-7.27603390512272,-179.129517970998,
4.20082013377292));
#35744=CARTESIAN_POINT('Ctrl Pts',(-4.85068927007173,-178.954517970998,
8.40164026752836));
#35745=CARTESIAN_POINT('Ctrl Pts',(1.5129078685785E-11,-178.779517970998,
8.40164026751963));
#35746=CARTESIAN_POINT('Ctrl Pts',(4.85068927010198,-178.604517970998,8.4016402675109));
#35747=CARTESIAN_POINT('Ctrl Pts',(7.27603390513785,-178.429517970998,4.20082013374672));
#35748=CARTESIAN_POINT('Ctrl Pts',(9.70137854017372,-178.254517970998,-1.74689612655491E-11));
#35749=CARTESIAN_POINT('Ctrl Pts',(7.27603390512273,-178.079517970998,-4.20082013377291));
#35750=CARTESIAN_POINT('Ctrl Pts',(4.85068927007173,-177.904517970998,-8.40164026752836));
#35751=CARTESIAN_POINT('Ctrl Pts',(-1.51301075899711E-11,-177.729517970998,
-8.40164026751963));
#35752=CARTESIAN_POINT('Ctrl Pts',(-4.85068927010199,-177.554517970998,
-8.4016402675109));
#35753=CARTESIAN_POINT('Ctrl Pts',(-7.27603390513785,-177.379517970998,
-4.20082013374671));
#35754=CARTESIAN_POINT('Ctrl Pts',(-9.70137854017372,-177.204517970998,
1.74701493417668E-11));
#35755=CARTESIAN_POINT('Ctrl Pts',(-7.27603390512272,-177.029517970998,
4.20082013377292));
#35756=CARTESIAN_POINT('Ctrl Pts',(-4.85068927007173,-176.854517970998,
8.40164026752836));
#35757=CARTESIAN_POINT('Ctrl Pts',(1.5129078685785E-11,-176.679517970998,
8.40164026751963));
#35758=CARTESIAN_POINT('Ctrl Pts',(4.85068927010198,-176.504517970998,8.4016402675109));
#35759=CARTESIAN_POINT('Ctrl Pts',(7.27603390513785,-176.329517970998,4.20082013374672));
#35760=CARTESIAN_POINT('Ctrl Pts',(9.70137854017372,-176.154517970998,-1.74689612655491E-11));
#35761=CARTESIAN_POINT('Ctrl Pts',(7.27603390512273,-175.979517970998,-4.20082013377291));
#35762=CARTESIAN_POINT('Ctrl Pts',(4.85068927007173,-175.804517970998,-8.40164026752836));
#35763=CARTESIAN_POINT('Ctrl Pts',(-1.51301075899711E-11,-175.629517970998,
-8.40164026751963));
#35764=CARTESIAN_POINT('Ctrl Pts',(-4.85068927010199,-175.454517970998,
-8.4016402675109));
#35765=CARTESIAN_POINT('Ctrl Pts',(-7.27603390513785,-175.279517970998,
-4.20082013374671));
#35766=CARTESIAN_POINT('Ctrl Pts',(-9.70137854017372,-175.104517970998,
1.74701493417668E-11));
#35767=CARTESIAN_POINT('Ctrl Pts',(-7.27603390512272,-174.929517970998,
4.20082013377292));
#35768=CARTESIAN_POINT('Ctrl Pts',(-4.85068927007173,-174.754517970998,
8.40164026752836));
#35769=CARTESIAN_POINT('Ctrl Pts',(1.5129078685785E-11,-174.579517970998,
8.40164026751963));
#35770=CARTESIAN_POINT('Ctrl Pts',(4.85068927010198,-174.404517970998,8.4016402675109));
#35771=CARTESIAN_POINT('Ctrl Pts',(7.27603390513785,-174.229517970998,4.20082013374672));
#35772=CARTESIAN_POINT('Ctrl Pts',(9.70137854017372,-174.054517970998,-1.74689612655491E-11));
#35773=CARTESIAN_POINT('Ctrl Pts',(7.27603390512273,-173.879517970998,-4.20082013377291));
#35774=CARTESIAN_POINT('Ctrl Pts',(4.85068927007173,-173.704517970998,-8.40164026752836));
#35775=CARTESIAN_POINT('Ctrl Pts',(-1.51301075899711E-11,-173.529517970998,
-8.40164026751963));
#35776=CARTESIAN_POINT('Ctrl Pts',(-4.85068927010199,-173.354517970998,
-8.4016402675109));
#35777=CARTESIAN_POINT('Ctrl Pts',(-7.27603390513785,-173.179517970998,
-4.20082013374671));
#35778=CARTESIAN_POINT('Ctrl Pts',(-9.70137854017372,-173.004517970998,
1.74701493417668E-11));
#35779=CARTESIAN_POINT('Ctrl Pts',(-7.27603390512272,-172.829517970998,
4.20082013377292));
#35780=CARTESIAN_POINT('Ctrl Pts',(-4.85068927007173,-172.654517970998,
8.40164026752836));
#35781=CARTESIAN_POINT('Ctrl Pts',(1.5129078685785E-11,-172.479517970998,
8.40164026751963));
#35782=CARTESIAN_POINT('Ctrl Pts',(4.85068927010198,-172.304517970998,8.4016402675109));
#35783=CARTESIAN_POINT('Ctrl Pts',(7.27603390513785,-172.129517970998,4.20082013374672));
#35784=CARTESIAN_POINT('Ctrl Pts',(9.70137854017372,-171.954517970998,-1.74689612655491E-11));
#35785=CARTESIAN_POINT('Ctrl Pts',(7.27603390512273,-171.779517970998,-4.20082013377291));
#35786=CARTESIAN_POINT('Ctrl Pts',(4.85068927007173,-171.604517970998,-8.40164026752836));
#35787=CARTESIAN_POINT('Ctrl Pts',(-1.51301075899711E-11,-171.429517970998,
-8.40164026751963));
#35788=CARTESIAN_POINT('Ctrl Pts',(-4.85068927010199,-171.254517970998,
-8.4016402675109));
#35789=CARTESIAN_POINT('Ctrl Pts',(-7.27603390513785,-171.079517970998,
-4.20082013374671));
#35790=CARTESIAN_POINT('Ctrl Pts',(-9.70137854017372,-170.904517970998,
1.74701493417668E-11));
#35791=CARTESIAN_POINT('Ctrl Pts',(-7.27603390512272,-170.729517970998,
4.20082013377292));
#35792=CARTESIAN_POINT('Ctrl Pts',(-4.85068927007173,-170.554517970998,
8.40164026752836));
#35793=CARTESIAN_POINT('Ctrl Pts',(1.5129078685785E-11,-170.379517970998,
8.40164026751963));
#35794=CARTESIAN_POINT('Ctrl Pts',(4.85068927010198,-170.204517970998,8.4016402675109));
#35795=CARTESIAN_POINT('Ctrl Pts',(7.27603390513785,-170.029517970998,4.20082013374672));
#35796=CARTESIAN_POINT('Ctrl Pts',(9.70137854017372,-169.854517970998,-1.74689612655491E-11));
#35797=CARTESIAN_POINT('Ctrl Pts',(7.27603390512273,-169.679517970998,-4.20082013377291));
#35798=CARTESIAN_POINT('Ctrl Pts',(4.85068927007173,-169.504517970998,-8.40164026752836));
#35799=CARTESIAN_POINT('Ctrl Pts',(-1.51301075899711E-11,-169.329517970998,
-8.40164026751963));
#35800=CARTESIAN_POINT('Ctrl Pts',(-4.85068927010199,-169.154517970998,
-8.4016402675109));
#35801=CARTESIAN_POINT('Ctrl Pts',(-7.27603390513785,-168.979517970998,
-4.20082013374671));
#35802=CARTESIAN_POINT('Ctrl Pts',(-9.70137854017372,-168.804517970998,
1.74701493417668E-11));
#35803=CARTESIAN_POINT('Ctrl Pts',(-7.27603390512272,-168.629517970998,
4.20082013377292));
#35804=CARTESIAN_POINT('Ctrl Pts',(-4.85068927007173,-168.454517970998,
8.40164026752836));
#35805=CARTESIAN_POINT('Ctrl Pts',(1.5129078685785E-11,-168.279517970998,
8.40164026751963));
#35806=CARTESIAN_POINT('Ctrl Pts',(4.85068927010198,-168.104517970998,8.4016402675109));
#35807=CARTESIAN_POINT('Ctrl Pts',(7.27603390513785,-167.929517970998,4.20082013374672));
#35808=CARTESIAN_POINT('Ctrl Pts',(9.70137854017372,-167.754517970998,-1.74689612655491E-11));
#35809=CARTESIAN_POINT('Ctrl Pts',(7.27603390512273,-167.579517970998,-4.20082013377291));
#35810=CARTESIAN_POINT('Ctrl Pts',(4.85068927007173,-167.404517970998,-8.40164026752836));
#35811=CARTESIAN_POINT('Ctrl Pts',(-1.51301075899711E-11,-167.229517970998,
-8.40164026751963));
#35812=CARTESIAN_POINT('Ctrl Pts',(-4.85068927010199,-167.054517970998,
-8.4016402675109));
#35813=CARTESIAN_POINT('Ctrl Pts',(-7.27603390513785,-166.879517970998,
-4.20082013374671));
#35814=CARTESIAN_POINT('Ctrl Pts',(-9.70137854017372,-166.704517970998,
1.74701493417668E-11));
#35815=CARTESIAN_POINT('Ctrl Pts',(-7.27603390512272,-166.529517970998,
4.20082013377292));
#35816=CARTESIAN_POINT('Ctrl Pts',(-4.85068927007173,-166.354517970998,
8.40164026752836));
#35817=CARTESIAN_POINT('Ctrl Pts',(1.5129078685785E-11,-166.179517970998,
8.40164026751963));
#35818=CARTESIAN_POINT('Ctrl Pts',(4.85068927010198,-166.004517970998,8.4016402675109));
#35819=CARTESIAN_POINT('Ctrl Pts',(7.27603390513785,-165.829517970998,4.20082013374672));
#35820=CARTESIAN_POINT('Ctrl Pts',(9.70137854017372,-165.654517970998,-1.74689612655491E-11));
#35821=CARTESIAN_POINT('Ctrl Pts',(7.27603390512273,-165.479517970998,-4.20082013377291));
#35822=CARTESIAN_POINT('Ctrl Pts',(4.85068927007173,-165.304517970998,-8.40164026752836));
#35823=CARTESIAN_POINT('Ctrl Pts',(-1.51301075899711E-11,-165.129517970998,
-8.40164026751963));
#35824=CARTESIAN_POINT('Ctrl Pts',(-4.85068927010199,-164.954517970998,
-8.4016402675109));
#35825=CARTESIAN_POINT('Ctrl Pts',(-7.27603390513785,-164.779517970998,
-4.20082013374671));
#35826=CARTESIAN_POINT('Ctrl Pts',(-9.70137854017372,-164.604517970998,
1.74701493417668E-11));
#35827=CARTESIAN_POINT('Ctrl Pts',(-7.27603390512272,-164.429517970998,
4.20082013377292));
#35828=CARTESIAN_POINT('Ctrl Pts',(-4.85068927007173,-164.254517970998,
8.40164026752836));
#35829=CARTESIAN_POINT('Ctrl Pts',(1.5129078685785E-11,-164.079517970998,
8.40164026751963));
#35830=CARTESIAN_POINT('Ctrl Pts',(4.85068927010198,-163.904517970998,8.4016402675109));
#35831=CARTESIAN_POINT('Ctrl Pts',(7.27603390513785,-163.729517970998,4.20082013374672));
#35832=CARTESIAN_POINT('Ctrl Pts',(9.70137854017372,-163.554517970998,-1.74689612655491E-11));
#35833=CARTESIAN_POINT('Ctrl Pts',(7.27603390512273,-163.379517970998,-4.20082013377291));
#35834=CARTESIAN_POINT('Ctrl Pts',(4.85068927007173,-163.204517970998,-8.40164026752836));
#35835=CARTESIAN_POINT('Ctrl Pts',(-1.51301075899711E-11,-163.029517970998,
-8.40164026751963));
#35836=CARTESIAN_POINT('Ctrl Pts',(-4.85068927010199,-162.854517970998,
-8.4016402675109));
#35837=CARTESIAN_POINT('Ctrl Pts',(-7.27603390513785,-162.679517970998,
-4.20082013374671));
#35838=CARTESIAN_POINT('Ctrl Pts',(-9.70137854017372,-162.504517970998,
1.74701493417668E-11));
#35839=CARTESIAN_POINT('Ctrl Pts',(-7.27603390512272,-162.329517970998,
4.20082013377292));
#35840=CARTESIAN_POINT('Ctrl Pts',(-4.85068927007173,-162.154517970998,
8.40164026752836));
#35841=CARTESIAN_POINT('Ctrl Pts',(1.5129078685785E-11,-161.979517970998,
8.40164026751963));
#35842=CARTESIAN_POINT('Ctrl Pts',(4.85068927010198,-161.804517970998,8.4016402675109));
#35843=CARTESIAN_POINT('Ctrl Pts',(7.27603390513785,-161.629517970998,4.20082013374672));
#35844=CARTESIAN_POINT('Ctrl Pts',(9.70137854017372,-161.454517970998,-1.74689612655491E-11));
#35845=CARTESIAN_POINT('Ctrl Pts',(7.27603390512273,-161.279517970998,-4.20082013377291));
#35846=CARTESIAN_POINT('Ctrl Pts',(4.85068927007173,-161.104517970998,-8.40164026752836));
#35847=CARTESIAN_POINT('Ctrl Pts',(-1.51301075899711E-11,-160.929517970998,
-8.40164026751963));
#35848=CARTESIAN_POINT('Ctrl Pts',(-4.85068927010199,-160.754517970998,
-8.4016402675109));
#35849=CARTESIAN_POINT('Ctrl Pts',(-7.27603390513785,-160.579517970998,
-4.20082013374671));
#35850=CARTESIAN_POINT('Ctrl Pts',(-9.70137854017372,-160.404517970998,
1.74701493417668E-11));
#35851=CARTESIAN_POINT('Ctrl Pts',(-7.27603390512272,-160.229517970998,
4.20082013377292));
#35852=CARTESIAN_POINT('Ctrl Pts',(-4.85068927007173,-160.054517970998,
8.40164026752836));
#35853=CARTESIAN_POINT('Ctrl Pts',(1.5129078685785E-11,-159.879517970998,
8.40164026751963));
#35854=CARTESIAN_POINT('Ctrl Pts',(4.85068927010198,-159.704517970998,8.4016402675109));
#35855=CARTESIAN_POINT('Ctrl Pts',(7.27603390513785,-159.529517970998,4.20082013374672));
#35856=CARTESIAN_POINT('Ctrl Pts',(9.70137854017372,-159.354517970998,-1.74689612655491E-11));
#35857=CARTESIAN_POINT('Ctrl Pts',(7.27603390512273,-159.179517970998,-4.20082013377291));
#35858=CARTESIAN_POINT('Ctrl Pts',(4.85068927007173,-159.004517970998,-8.40164026752836));
#35859=CARTESIAN_POINT('Ctrl Pts',(-1.51301075899711E-11,-158.829517970998,
-8.40164026751963));
#35860=CARTESIAN_POINT('Ctrl Pts',(-4.85068927010199,-158.654517970998,
-8.4016402675109));
#35861=CARTESIAN_POINT('Ctrl Pts',(-7.27603390513785,-158.479517970998,
-4.20082013374671));
#35862=CARTESIAN_POINT('Ctrl Pts',(-9.70137854017372,-158.304517970998,
1.74701493417668E-11));
#35863=CARTESIAN_POINT('Ctrl Pts',(-7.27603390512272,-158.129517970998,
4.20082013377292));
#35864=CARTESIAN_POINT('Ctrl Pts',(-4.85068927007173,-157.954517970998,
8.40164026752836));
#35865=CARTESIAN_POINT('Ctrl Pts',(1.5129078685785E-11,-157.779517970998,
8.40164026751963));
#35866=CARTESIAN_POINT('Ctrl Pts',(4.85068927010198,-157.604517970998,8.4016402675109));
#35867=CARTESIAN_POINT('Ctrl Pts',(7.27603390513785,-157.429517970998,4.20082013374672));
#35868=CARTESIAN_POINT('Ctrl Pts',(9.70137854017372,-157.254517970998,-1.74689612655491E-11));
#35869=CARTESIAN_POINT('Ctrl Pts',(7.27603390512273,-157.079517970998,-4.20082013377291));
#35870=CARTESIAN_POINT('Ctrl Pts',(4.85068927007173,-156.904517970998,-8.40164026752836));
#35871=CARTESIAN_POINT('Ctrl Pts',(-1.51301075899711E-11,-156.729517970998,
-8.40164026751963));
#35872=CARTESIAN_POINT('Ctrl Pts',(-4.85068927010199,-156.554517970998,
-8.4016402675109));
#35873=CARTESIAN_POINT('Ctrl Pts',(-7.27603390513785,-156.379517970998,
-4.20082013374671));
#35874=CARTESIAN_POINT('Ctrl Pts',(-9.70137854017372,-156.204517970998,
1.74701493417668E-11));
#35875=CARTESIAN_POINT('Ctrl Pts',(-7.27603390512272,-156.029517970998,
4.20082013377292));
#35876=CARTESIAN_POINT('Ctrl Pts',(-4.85068927007173,-155.854517970998,
8.40164026752836));
#35877=CARTESIAN_POINT('Ctrl Pts',(1.5129078685785E-11,-155.679517970998,
8.40164026751963));
#35878=CARTESIAN_POINT('Ctrl Pts',(4.85068927010198,-155.504517970998,8.4016402675109));
#35879=CARTESIAN_POINT('Ctrl Pts',(7.27603390513785,-155.329517970998,4.20082013374672));
#35880=CARTESIAN_POINT('Ctrl Pts',(9.70137854017372,-155.154517970998,-1.74689612655491E-11));
#35881=CARTESIAN_POINT('Ctrl Pts',(7.27603390512273,-154.979517970998,-4.20082013377291));
#35882=CARTESIAN_POINT('Ctrl Pts',(4.85068927007173,-154.804517970998,-8.40164026752836));
#35883=CARTESIAN_POINT('Ctrl Pts',(-1.51301075899711E-11,-154.629517970998,
-8.40164026751963));
#35884=CARTESIAN_POINT('Ctrl Pts',(-4.85068927010199,-154.454517970998,
-8.4016402675109));
#35885=CARTESIAN_POINT('Ctrl Pts',(-7.27603390513785,-154.279517970998,
-4.20082013374671));
#35886=CARTESIAN_POINT('Ctrl Pts',(-9.70137854017372,-154.104517970998,
1.74701493417668E-11));
#35887=CARTESIAN_POINT('Ctrl Pts',(-7.27603390512272,-153.929517970998,
4.20082013377292));
#35888=CARTESIAN_POINT('Ctrl Pts',(-4.85068927007173,-153.754517970998,
8.40164026752836));
#35889=CARTESIAN_POINT('Ctrl Pts',(1.5129078685785E-11,-153.579517970998,
8.40164026751963));
#35890=CARTESIAN_POINT('Ctrl Pts',(4.85068927010198,-153.404517970998,8.4016402675109));
#35891=CARTESIAN_POINT('Ctrl Pts',(7.27603390513785,-153.229517970998,4.20082013374672));
#35892=CARTESIAN_POINT('Ctrl Pts',(9.70137854017372,-153.054517970998,-1.74689612655491E-11));
#35893=CARTESIAN_POINT('Ctrl Pts',(7.27603390512273,-152.879517970998,-4.20082013377291));
#35894=CARTESIAN_POINT('Ctrl Pts',(4.85068927007173,-152.704517970998,-8.40164026752836));
#35895=CARTESIAN_POINT('Ctrl Pts',(-1.51301075899711E-11,-152.529517970998,
-8.40164026751963));
#35896=CARTESIAN_POINT('Ctrl Pts',(-4.85068927010199,-152.354517970998,
-8.4016402675109));
#35897=CARTESIAN_POINT('Ctrl Pts',(-7.27603390513785,-152.179517970998,
-4.20082013374671));
#35898=CARTESIAN_POINT('Ctrl Pts',(-9.70137854017372,-152.004517970998,
1.74701493417668E-11));
#35899=CARTESIAN_POINT('Ctrl Pts',(-7.27603390512272,-151.829517970998,
4.20082013377292));
#35900=CARTESIAN_POINT('Ctrl Pts',(-4.85068927007173,-151.654517970998,
8.40164026752836));
#35901=CARTESIAN_POINT('Ctrl Pts',(1.5129078685785E-11,-151.479517970998,
8.40164026751963));
#35902=CARTESIAN_POINT('Ctrl Pts',(4.85068927010198,-151.304517970998,8.4016402675109));
#35903=CARTESIAN_POINT('Ctrl Pts',(7.27603390513785,-151.129517970998,4.20082013374672));
#35904=CARTESIAN_POINT('Ctrl Pts',(9.70137854017372,-150.954517970998,-1.74689612655491E-11));
#35905=CARTESIAN_POINT('Ctrl Pts',(7.27603390512273,-150.779517970998,-4.20082013377291));
#35906=CARTESIAN_POINT('Ctrl Pts',(4.85068927007173,-150.604517970998,-8.40164026752836));
#35907=CARTESIAN_POINT('Ctrl Pts',(-1.51301075899711E-11,-150.429517970998,
-8.40164026751963));
#35908=CARTESIAN_POINT('Ctrl Pts',(-4.85068927010199,-150.254517970998,
-8.4016402675109));
#35909=CARTESIAN_POINT('Ctrl Pts',(-7.27603390513785,-150.079517970998,
-4.20082013374671));
#35910=CARTESIAN_POINT('Ctrl Pts',(-9.70137854017372,-149.904517970998,
1.74701493417668E-11));
#35911=CARTESIAN_POINT('Ctrl Pts',(-7.27603390512272,-149.729517970998,
4.20082013377292));
#35912=CARTESIAN_POINT('Ctrl Pts',(-4.85068927007173,-149.554517970998,
8.40164026752836));
#35913=CARTESIAN_POINT('Ctrl Pts',(1.5129078685785E-11,-149.379517970998,
8.40164026751963));
#35914=CARTESIAN_POINT('Ctrl Pts',(4.85068927010198,-149.204517970998,8.4016402675109));
#35915=CARTESIAN_POINT('Ctrl Pts',(7.27603390513785,-149.029517970998,4.20082013374672));
#35916=CARTESIAN_POINT('Ctrl Pts',(9.70137854017372,-148.854517970998,-1.74689612655491E-11));
#35917=CARTESIAN_POINT('Ctrl Pts',(7.27603390512273,-148.679517970998,-4.20082013377291));
#35918=CARTESIAN_POINT('Ctrl Pts',(4.85068927007173,-148.504517970998,-8.40164026752836));
#35919=CARTESIAN_POINT('Ctrl Pts',(-1.51301075899711E-11,-148.329517970998,
-8.40164026751963));
#35920=CARTESIAN_POINT('Ctrl Pts',(-4.85068927010199,-148.154517970998,
-8.4016402675109));
#35921=CARTESIAN_POINT('Ctrl Pts',(-7.27603390513785,-147.979517970998,
-4.20082013374671));
#35922=CARTESIAN_POINT('Ctrl Pts',(-9.70137854017372,-147.804517970998,
1.74701493417668E-11));
#35923=CARTESIAN_POINT('Ctrl Pts',(-7.27603390512272,-147.629517970998,
4.20082013377292));
#35924=CARTESIAN_POINT('Ctrl Pts',(-4.85068927007173,-147.454517970998,
8.40164026752836));
#35925=CARTESIAN_POINT('Ctrl Pts',(1.5129078685785E-11,-147.279517970998,
8.40164026751963));
#35926=CARTESIAN_POINT('Ctrl Pts',(4.85068927010198,-147.104517970998,8.4016402675109));
#35927=CARTESIAN_POINT('Ctrl Pts',(7.27603390513785,-146.929517970998,4.20082013374672));
#35928=CARTESIAN_POINT('Ctrl Pts',(9.70137854017372,-146.754517970998,-1.74689612655491E-11));
#35929=CARTESIAN_POINT('Ctrl Pts',(7.27603390512273,-146.579517970998,-4.20082013377291));
#35930=CARTESIAN_POINT('Ctrl Pts',(4.85068927007173,-146.404517970998,-8.40164026752836));
#35931=CARTESIAN_POINT('Ctrl Pts',(-1.51301075899711E-11,-146.229517970998,
-8.40164026751963));
#35932=CARTESIAN_POINT('Ctrl Pts',(-4.85068927010199,-146.054517970998,
-8.4016402675109));
#35933=CARTESIAN_POINT('Ctrl Pts',(-7.27603390513785,-145.879517970998,
-4.20082013374671));
#35934=CARTESIAN_POINT('Ctrl Pts',(-9.70137854017372,-145.704517970998,
1.74701493417668E-11));
#35935=CARTESIAN_POINT('Ctrl Pts',(-7.27603390512272,-145.529517970998,
4.20082013377292));
#35936=CARTESIAN_POINT('Ctrl Pts',(-4.85068927007173,-145.354517970998,
8.40164026752836));
#35937=CARTESIAN_POINT('Ctrl Pts',(1.5129078685785E-11,-145.179517970998,
8.40164026751963));
#35938=CARTESIAN_POINT('Ctrl Pts',(4.85068927010198,-145.004517970998,8.4016402675109));
#35939=CARTESIAN_POINT('Ctrl Pts',(7.27603390513785,-144.829517970998,4.20082013374672));
#35940=CARTESIAN_POINT('Ctrl Pts',(9.70137854017372,-144.654517970998,-1.74689612655491E-11));
#35941=CARTESIAN_POINT('Ctrl Pts',(7.27603390512273,-144.479517970998,-4.20082013377291));
#35942=CARTESIAN_POINT('Ctrl Pts',(4.85068927007173,-144.304517970998,-8.40164026752836));
#35943=CARTESIAN_POINT('Ctrl Pts',(-1.51301075899711E-11,-144.129517970998,
-8.40164026751963));
#35944=CARTESIAN_POINT('Ctrl Pts',(-4.85068927010199,-143.954517970998,
-8.4016402675109));
#35945=CARTESIAN_POINT('Ctrl Pts',(-7.27603390513785,-143.779517970998,
-4.20082013374671));
#35946=CARTESIAN_POINT('Ctrl Pts',(-9.70137854017372,-143.604517970998,
1.74701493417668E-11));
#35947=CARTESIAN_POINT('Ctrl Pts',(-7.27603390512272,-143.429517970998,
4.20082013377292));
#35948=CARTESIAN_POINT('Ctrl Pts',(-4.85068927007173,-143.254517970998,
8.40164026752836));
#35949=CARTESIAN_POINT('Ctrl Pts',(1.5129078685785E-11,-143.079517970998,
8.40164026751963));
#35950=CARTESIAN_POINT('Ctrl Pts',(4.85068927010198,-142.904517970998,8.4016402675109));
#35951=CARTESIAN_POINT('Ctrl Pts',(7.27603390513785,-142.729517970998,4.20082013374672));
#35952=CARTESIAN_POINT('Ctrl Pts',(9.70137854017372,-142.554517970998,-1.74689612655491E-11));
#35953=CARTESIAN_POINT('Ctrl Pts',(7.27603390512273,-142.379517970998,-4.20082013377291));
#35954=CARTESIAN_POINT('Ctrl Pts',(4.85068927007173,-142.204517970998,-8.40164026752836));
#35955=CARTESIAN_POINT('Ctrl Pts',(-1.51301075899711E-11,-142.029517970998,
-8.40164026751963));
#35956=CARTESIAN_POINT('Ctrl Pts',(-4.85068927010199,-141.854517970998,
-8.4016402675109));
#35957=CARTESIAN_POINT('Ctrl Pts',(-7.27603390513785,-141.679517970998,
-4.20082013374671));
#35958=CARTESIAN_POINT('Ctrl Pts',(-9.70137854017372,-141.504517970998,
1.74701493417668E-11));
#35959=CARTESIAN_POINT('Ctrl Pts',(-7.27603390512272,-141.329517970998,
4.20082013377292));
#35960=CARTESIAN_POINT('Ctrl Pts',(-4.85068927007173,-141.154517970998,
8.40164026752836));
#35961=CARTESIAN_POINT('Ctrl Pts',(1.5129078685785E-11,-140.979517970998,
8.40164026751963));
#35962=CARTESIAN_POINT('Ctrl Pts',(4.85068927010198,-140.804517970998,8.4016402675109));
#35963=CARTESIAN_POINT('Ctrl Pts',(7.27603390513785,-140.629517970998,4.20082013374672));
#35964=CARTESIAN_POINT('Ctrl Pts',(9.70137854017372,-140.454517970998,-1.74689612655491E-11));
#35965=CARTESIAN_POINT('Ctrl Pts',(7.27603390512273,-140.279517970998,-4.20082013377291));
#35966=CARTESIAN_POINT('Ctrl Pts',(4.85068927007173,-140.104517970998,-8.40164026752836));
#35967=CARTESIAN_POINT('Ctrl Pts',(-1.51301075899711E-11,-139.929517970998,
-8.40164026751963));
#35968=CARTESIAN_POINT('Ctrl Pts',(-4.85068927010199,-139.754517970998,
-8.4016402675109));
#35969=CARTESIAN_POINT('Ctrl Pts',(-7.27603390513785,-139.579517970998,
-4.20082013374671));
#35970=CARTESIAN_POINT('Ctrl Pts',(-9.70137854017372,-139.404517970998,
1.74701493417668E-11));
#35971=CARTESIAN_POINT('Ctrl Pts',(-7.27603390512272,-139.229517970998,
4.20082013377292));
#35972=CARTESIAN_POINT('Ctrl Pts',(-4.85068927007173,-139.054517970998,
8.40164026752836));
#35973=CARTESIAN_POINT('Ctrl Pts',(1.5129078685785E-11,-138.879517970998,
8.40164026751963));
#35974=CARTESIAN_POINT('Ctrl Pts',(4.85068927010198,-138.704517970998,8.4016402675109));
#35975=CARTESIAN_POINT('Ctrl Pts',(7.27603390513785,-138.529517970998,4.20082013374672));
#35976=CARTESIAN_POINT('Ctrl Pts',(9.70137854017372,-138.354517970998,-1.74689612655491E-11));
#35977=CARTESIAN_POINT('Ctrl Pts',(7.27603390512273,-138.179517970998,-4.20082013377291));
#35978=CARTESIAN_POINT('Ctrl Pts',(4.85068927007173,-138.004517970998,-8.40164026752836));
#35979=CARTESIAN_POINT('Ctrl Pts',(-1.51301075899711E-11,-137.829517970998,
-8.40164026751963));
#35980=CARTESIAN_POINT('Ctrl Pts',(-4.85068927010199,-137.654517970998,
-8.4016402675109));
#35981=CARTESIAN_POINT('Ctrl Pts',(-7.27603390513785,-137.479517970998,
-4.20082013374671));
#35982=CARTESIAN_POINT('Ctrl Pts',(-9.70137854017372,-137.304517970998,
1.74701493417668E-11));
#35983=CARTESIAN_POINT('Ctrl Pts',(-7.27603390512272,-137.129517970998,
4.20082013377292));
#35984=CARTESIAN_POINT('Ctrl Pts',(-4.85068927007173,-136.954517970998,
8.40164026752836));
#35985=CARTESIAN_POINT('Ctrl Pts',(1.5129078685785E-11,-136.779517970998,
8.40164026751963));
#35986=CARTESIAN_POINT('Ctrl Pts',(4.85068927010198,-136.604517970998,8.4016402675109));
#35987=CARTESIAN_POINT('Ctrl Pts',(7.27603390513785,-136.429517970998,4.20082013374672));
#35988=CARTESIAN_POINT('Ctrl Pts',(9.70137854017372,-136.254517970999,-1.74689612655491E-11));
#35989=CARTESIAN_POINT('Ctrl Pts',(7.27603390512273,-136.079517970998,-4.20082013377291));
#35990=CARTESIAN_POINT('Ctrl Pts',(4.85068927007173,-135.904517970998,-8.40164026752836));
#35991=CARTESIAN_POINT('Ctrl Pts',(-1.51301075899711E-11,-135.729517970998,
-8.40164026751963));
#35992=CARTESIAN_POINT('Ctrl Pts',(-4.85068927010199,-135.554517970998,
-8.4016402675109));
#35993=CARTESIAN_POINT('Ctrl Pts',(-7.27603390513785,-135.379517970998,
-4.20082013374671));
#35994=CARTESIAN_POINT('Ctrl Pts',(-9.70137854017372,-135.204517970998,
1.74701493417668E-11));
#35995=CARTESIAN_POINT('Ctrl Pts',(-7.27603390512272,-135.029517970998,
4.20082013377292));
#35996=CARTESIAN_POINT('Ctrl Pts',(-4.85068927007173,-134.854517970998,
8.40164026752836));
#35997=CARTESIAN_POINT('Ctrl Pts',(1.5129078685785E-11,-134.679517970998,
8.40164026751963));
#35998=CARTESIAN_POINT('Ctrl Pts',(4.85068927010198,-134.504517970998,8.4016402675109));
#35999=CARTESIAN_POINT('Ctrl Pts',(7.27603390513785,-134.329517970998,4.20082013374672));
#36000=CARTESIAN_POINT('Ctrl Pts',(9.70137854017372,-134.154517970998,-1.74689612655491E-11));
#36001=CARTESIAN_POINT('Ctrl Pts',(7.27603390512273,-133.979517970998,-4.20082013377291));
#36002=CARTESIAN_POINT('Ctrl Pts',(4.85068927007173,-133.804517970998,-8.40164026752836));
#36003=CARTESIAN_POINT('Ctrl Pts',(-1.51301075899711E-11,-133.629517970998,
-8.40164026751963));
#36004=CARTESIAN_POINT('Ctrl Pts',(-4.85068927010199,-133.454517970998,
-8.4016402675109));
#36005=CARTESIAN_POINT('Ctrl Pts',(-7.27603390513785,-133.279517970998,
-4.20082013374671));
#36006=CARTESIAN_POINT('Ctrl Pts',(-9.70137854017372,-133.104517970998,
1.74701493417668E-11));
#36007=CARTESIAN_POINT('Ctrl Pts',(-7.27603390512272,-132.929517970998,
4.20082013377292));
#36008=CARTESIAN_POINT('Ctrl Pts',(-4.85068927007173,-132.754517970998,
8.40164026752836));
#36009=CARTESIAN_POINT('Ctrl Pts',(1.5129078685785E-11,-132.579517970998,
8.40164026751963));
#36010=CARTESIAN_POINT('Ctrl Pts',(4.85068927010198,-132.404517970998,8.4016402675109));
#36011=CARTESIAN_POINT('Ctrl Pts',(7.27603390513785,-132.229517970998,4.20082013374672));
#36012=CARTESIAN_POINT('Ctrl Pts',(9.70137854017372,-132.054517970998,-1.74689612655491E-11));
#36013=CARTESIAN_POINT('Ctrl Pts',(7.27603390512273,-131.879517970998,-4.20082013377291));
#36014=CARTESIAN_POINT('Ctrl Pts',(4.85068927007173,-131.704517970998,-8.40164026752836));
#36015=CARTESIAN_POINT('Ctrl Pts',(-1.51301075899711E-11,-131.529517970998,
-8.40164026751963));
#36016=CARTESIAN_POINT('Ctrl Pts',(-4.85068927010199,-131.354517970998,
-8.4016402675109));
#36017=CARTESIAN_POINT('Ctrl Pts',(-7.27603390513785,-131.179517970998,
-4.20082013374671));
#36018=CARTESIAN_POINT('Ctrl Pts',(-9.70137854017372,-131.004517970998,
1.74701493417668E-11));
#36019=CARTESIAN_POINT('Ctrl Pts',(-7.27603390512272,-130.829517970998,
4.20082013377292));
#36020=CARTESIAN_POINT('Ctrl Pts',(-4.85068927007173,-130.654517970998,
8.40164026752836));
#36021=CARTESIAN_POINT('Ctrl Pts',(1.5129078685785E-11,-130.479517970998,
8.40164026751963));
#36022=CARTESIAN_POINT('Ctrl Pts',(4.85068927010198,-130.304517970998,8.4016402675109));
#36023=CARTESIAN_POINT('Ctrl Pts',(7.27603390513785,-130.129517970998,4.20082013374672));
#36024=CARTESIAN_POINT('Ctrl Pts',(9.70137854017372,-129.954517970998,-1.74689612655491E-11));
#36025=CARTESIAN_POINT('Ctrl Pts',(7.27603390512273,-129.779517970998,-4.20082013377291));
#36026=CARTESIAN_POINT('Ctrl Pts',(4.85068927007173,-129.604517970998,-8.40164026752836));
#36027=CARTESIAN_POINT('Ctrl Pts',(-1.51301075899711E-11,-129.429517970998,
-8.40164026751963));
#36028=CARTESIAN_POINT('Ctrl Pts',(-4.85068927010199,-129.254517970998,
-8.4016402675109));
#36029=CARTESIAN_POINT('Ctrl Pts',(-7.27603390513785,-129.079517970998,
-4.20082013374671));
#36030=CARTESIAN_POINT('Ctrl Pts',(-9.70137854017372,-128.904517970998,
1.74701493417668E-11));
#36031=CARTESIAN_POINT('Ctrl Pts',(-7.27603390512272,-128.729517970998,
4.20082013377292));
#36032=CARTESIAN_POINT('Ctrl Pts',(-4.85068927007173,-128.554517970998,
8.40164026752836));
#36033=CARTESIAN_POINT('Ctrl Pts',(1.5129078685785E-11,-128.379517970998,
8.40164026751963));
#36034=CARTESIAN_POINT('Ctrl Pts',(4.85068927010198,-128.204517970998,8.4016402675109));
#36035=CARTESIAN_POINT('Ctrl Pts',(7.27603390513785,-128.029517970998,4.20082013374672));
#36036=CARTESIAN_POINT('Ctrl Pts',(9.70137854017372,-127.854517970998,-1.74689612655491E-11));
#36037=CARTESIAN_POINT('Ctrl Pts',(7.27603390512273,-127.679517970998,-4.20082013377291));
#36038=CARTESIAN_POINT('Ctrl Pts',(4.85068927007173,-127.504517970998,-8.40164026752836));
#36039=CARTESIAN_POINT('Ctrl Pts',(-1.51301075899711E-11,-127.329517970998,
-8.40164026751963));
#36040=CARTESIAN_POINT('Ctrl Pts',(-4.85068927010199,-127.154517970998,
-8.4016402675109));
#36041=CARTESIAN_POINT('Ctrl Pts',(-7.27603390513785,-126.979517970998,
-4.20082013374671));
#36042=CARTESIAN_POINT('Ctrl Pts',(-9.70137854017372,-126.804517970998,
1.74701493417668E-11));
#36043=CARTESIAN_POINT('Ctrl Pts',(-7.27603390512272,-126.629517970998,
4.20082013377292));
#36044=CARTESIAN_POINT('Ctrl Pts',(-4.85068927007173,-126.454517970998,
8.40164026752836));
#36045=CARTESIAN_POINT('Ctrl Pts',(1.5129078685785E-11,-126.279517970998,
8.40164026751963));
#36046=CARTESIAN_POINT('Ctrl Pts',(4.85068927010198,-126.104517970998,8.4016402675109));
#36047=CARTESIAN_POINT('Ctrl Pts',(7.27603390513785,-125.929517970998,4.20082013374672));
#36048=CARTESIAN_POINT('Ctrl Pts',(9.70137854017372,-125.754517970998,-1.74689612655491E-11));
#36049=CARTESIAN_POINT('Ctrl Pts',(7.27603390512273,-125.579517970998,-4.20082013377291));
#36050=CARTESIAN_POINT('Ctrl Pts',(4.85068927007173,-125.404517970998,-8.40164026752836));
#36051=CARTESIAN_POINT('Ctrl Pts',(-1.51301075899711E-11,-125.229517970998,
-8.40164026751963));
#36052=CARTESIAN_POINT('Ctrl Pts',(-4.85068927010199,-125.054517970998,
-8.4016402675109));
#36053=CARTESIAN_POINT('Ctrl Pts',(-7.27603390513785,-124.879517970998,
-4.20082013374671));
#36054=CARTESIAN_POINT('Ctrl Pts',(-9.70137854017372,-124.704517970998,
1.74701493417668E-11));
#36055=CARTESIAN_POINT('Ctrl Pts',(-7.27603390512272,-124.529517970998,
4.20082013377292));
#36056=CARTESIAN_POINT('Ctrl Pts',(-4.85068927007173,-124.354517970998,
8.40164026752836));
#36057=CARTESIAN_POINT('Ctrl Pts',(1.5129078685785E-11,-124.179517970998,
8.40164026751963));
#36058=CARTESIAN_POINT('Ctrl Pts',(4.85068927010198,-124.004517970998,8.4016402675109));
#36059=CARTESIAN_POINT('Ctrl Pts',(7.27603390513785,-123.829517970998,4.20082013374672));
#36060=CARTESIAN_POINT('Ctrl Pts',(9.70137854017372,-123.654517970998,-1.74689612655491E-11));
#36061=CARTESIAN_POINT('Ctrl Pts',(7.27603390512273,-123.479517970998,-4.20082013377291));
#36062=CARTESIAN_POINT('Ctrl Pts',(4.85068927007173,-123.304517970998,-8.40164026752836));
#36063=CARTESIAN_POINT('Ctrl Pts',(-1.51301075899711E-11,-123.129517970998,
-8.40164026751963));
#36064=CARTESIAN_POINT('Ctrl Pts',(-4.85068927010199,-122.954517970998,
-8.4016402675109));
#36065=CARTESIAN_POINT('Ctrl Pts',(-7.27603390513785,-122.779517970998,
-4.20082013374671));
#36066=CARTESIAN_POINT('Ctrl Pts',(-9.70137854017372,-122.604517970998,
1.74701493417668E-11));
#36067=CARTESIAN_POINT('Ctrl Pts',(-7.27603390512272,-122.429517970998,
4.20082013377292));
#36068=CARTESIAN_POINT('Ctrl Pts',(-4.85068927007173,-122.254517970998,
8.40164026752836));
#36069=CARTESIAN_POINT('Ctrl Pts',(1.5129078685785E-11,-122.079517970998,
8.40164026751963));
#36070=CARTESIAN_POINT('Ctrl Pts',(4.85068927010198,-121.904517970998,8.4016402675109));
#36071=CARTESIAN_POINT('Ctrl Pts',(7.27603390513785,-121.729517970998,4.20082013374672));
#36072=CARTESIAN_POINT('Ctrl Pts',(9.70137854017372,-121.554517970999,-1.74689612655491E-11));
#36073=CARTESIAN_POINT('Ctrl Pts',(7.27603390512273,-121.379517970998,-4.20082013377291));
#36074=CARTESIAN_POINT('Ctrl Pts',(4.85068927007173,-121.204517970998,-8.40164026752836));
#36075=CARTESIAN_POINT('Ctrl Pts',(-1.51301075899711E-11,-121.029517970998,
-8.40164026751963));
#36076=CARTESIAN_POINT('Ctrl Pts',(-4.85068927010199,-120.854517970999,
-8.4016402675109));
#36077=CARTESIAN_POINT('Ctrl Pts',(-7.27603390513785,-120.679517970999,
-4.20082013374671));
#36078=CARTESIAN_POINT('Ctrl Pts',(-9.70137854017372,-120.504517970999,
1.74701493417668E-11));
#36079=CARTESIAN_POINT('Ctrl Pts',(-7.27603390512272,-120.329517970998,
4.20082013377292));
#36080=CARTESIAN_POINT('Ctrl Pts',(-4.85068927007173,-120.154517970998,
8.40164026752836));
#36081=CARTESIAN_POINT('Ctrl Pts',(1.5129078685785E-11,-119.979517970999,
8.40164026751963));
#36082=CARTESIAN_POINT('Ctrl Pts',(4.85068927010198,-119.804517970999,8.4016402675109));
#36083=CARTESIAN_POINT('Ctrl Pts',(7.27603390513785,-119.629517970998,4.20082013374672));
#36084=CARTESIAN_POINT('Ctrl Pts',(9.70137854017372,-119.454517970998,-1.74689612655491E-11));
#36085=CARTESIAN_POINT('Ctrl Pts',(7.27603390512273,-119.279517970999,-4.20082013377291));
#36086=CARTESIAN_POINT('Ctrl Pts',(4.85068927007173,-119.104517970998,-8.40164026752836));
#36087=CARTESIAN_POINT('Ctrl Pts',(-1.51301075899711E-11,-118.929517970998,
-8.40164026751963));
#36088=CARTESIAN_POINT('Ctrl Pts',(-4.85068927010199,-118.754517970998,
-8.4016402675109));
#36089=CARTESIAN_POINT('Ctrl Pts',(-7.27603390513785,-118.579517970998,
-4.20082013374671));
#36090=CARTESIAN_POINT('Ctrl Pts',(-9.70137854017372,-118.404517970999,
1.74701493417668E-11));
#36091=CARTESIAN_POINT('Ctrl Pts',(-7.27603390512272,-118.229517970998,
4.20082013377292));
#36092=CARTESIAN_POINT('Ctrl Pts',(-4.85068927007173,-118.054517970998,
8.40164026752836));
#36093=CARTESIAN_POINT('Ctrl Pts',(1.5129078685785E-11,-117.879517970999,
8.40164026751963));
#36094=CARTESIAN_POINT('Ctrl Pts',(4.85068927010198,-117.704517970998,8.4016402675109));
#36095=CARTESIAN_POINT('Ctrl Pts',(7.27603390513785,-117.529517970998,4.20082013374672));
#36096=CARTESIAN_POINT('Ctrl Pts',(9.70137854017372,-117.354517970999,-1.74689612655491E-11));
#36097=CARTESIAN_POINT('Ctrl Pts',(7.27603390512273,-117.179517970999,-4.20082013377291));
#36098=CARTESIAN_POINT('Ctrl Pts',(4.85068927007173,-117.004517970999,-8.40164026752836));
#36099=CARTESIAN_POINT('Ctrl Pts',(-1.51301075899711E-11,-116.829517970998,
-8.40164026751963));
#36100=CARTESIAN_POINT('Ctrl Pts',(-4.85068927010199,-116.654517970998,
-8.4016402675109));
#36101=CARTESIAN_POINT('Ctrl Pts',(-7.27603390513785,-116.479517970999,
-4.20082013374671));
#36102=CARTESIAN_POINT('Ctrl Pts',(-9.70137854017372,-116.304517970999,
1.74701493417668E-11));
#36103=CARTESIAN_POINT('Ctrl Pts',(-7.27603390512272,-116.129517970999,
4.20082013377292));
#36104=CARTESIAN_POINT('Ctrl Pts',(-4.85068927007173,-115.954517970998,
8.40164026752836));
#36105=CARTESIAN_POINT('Ctrl Pts',(1.5129078685785E-11,-115.779517970998,
8.40164026751963));
#36106=CARTESIAN_POINT('Ctrl Pts',(4.85068927010198,-115.604517970999,8.4016402675109));
#36107=CARTESIAN_POINT('Ctrl Pts',(7.27603390513785,-115.429517970999,4.20082013374672));
#36108=CARTESIAN_POINT('Ctrl Pts',(9.70137854017372,-115.254517970999,-1.74689612655491E-11));
#36109=CARTESIAN_POINT('Ctrl Pts',(7.27603390512273,-115.079517970998,-4.20082013377291));
#36110=CARTESIAN_POINT('Ctrl Pts',(4.85068927007173,-114.904517970999,-8.40164026752836));
#36111=CARTESIAN_POINT('Ctrl Pts',(-1.51301075899711E-11,-114.729517970999,
-8.40164026751963));
#36112=CARTESIAN_POINT('Ctrl Pts',(-4.85068927010199,-114.554517970999,
-8.4016402675109));
#36113=CARTESIAN_POINT('Ctrl Pts',(-7.27603390513785,-114.379517970999,
-4.20082013374671));
#36114=CARTESIAN_POINT('Ctrl Pts',(-9.70137854017372,-114.204517970999,
1.74701493417668E-11));
#36115=CARTESIAN_POINT('Ctrl Pts',(-7.27603390512272,-114.029517970999,
4.20082013377292));
#36116=CARTESIAN_POINT('Ctrl Pts',(-4.85068927007173,-113.854517970999,
8.40164026752836));
#36117=CARTESIAN_POINT('Ctrl Pts',(1.5129078685785E-11,-113.679517970999,
8.40164026751963));
#36118=CARTESIAN_POINT('Ctrl Pts',(4.85068927010198,-113.504517970999,8.4016402675109));
#36119=CARTESIAN_POINT('Ctrl Pts',(7.27603390513785,-113.329517970999,4.20082013374672));
#36120=CARTESIAN_POINT('Ctrl Pts',(9.70137854017372,-113.154517970999,-1.74689612655491E-11));
#36121=CARTESIAN_POINT('Ctrl Pts',(7.27603390512273,-112.979517970999,-4.20082013377291));
#36122=CARTESIAN_POINT('Ctrl Pts',(4.85068927007173,-112.804517970999,-8.40164026752836));
#36123=CARTESIAN_POINT('Ctrl Pts',(-1.51301075899711E-11,-112.629517970999,
-8.40164026751963));
#36124=CARTESIAN_POINT('Ctrl Pts',(-4.85068927010199,-112.454517970998,
-8.4016402675109));
#36125=CARTESIAN_POINT('Ctrl Pts',(-7.27603390513785,-112.279517970998,
-4.20082013374671));
#36126=CARTESIAN_POINT('Ctrl Pts',(-9.70137854017372,-112.104517970999,
1.74701493417668E-11));
#36127=CARTESIAN_POINT('Ctrl Pts',(-7.27603390512272,-111.929517970999,
4.20082013377292));
#36128=CARTESIAN_POINT('Ctrl Pts',(-4.85068927007173,-111.754517970999,
8.40164026752836));
#36129=CARTESIAN_POINT('Ctrl Pts',(1.5129078685785E-11,-111.579517970999,
8.40164026751963));
#36130=CARTESIAN_POINT('Ctrl Pts',(4.85068927010198,-111.404517970998,8.4016402675109));
#36131=CARTESIAN_POINT('Ctrl Pts',(7.27603390513785,-111.229517970999,4.20082013374672));
#36132=CARTESIAN_POINT('Ctrl Pts',(9.70137854017372,-111.054517970999,-1.74689612655491E-11));
#36133=CARTESIAN_POINT('Ctrl Pts',(7.27603390512273,-110.879517970999,-4.20082013377291));
#36134=CARTESIAN_POINT('Ctrl Pts',(4.85068927007173,-110.704517970999,-8.40164026752836));
#36135=CARTESIAN_POINT('Ctrl Pts',(-1.51301075899711E-11,-110.529517970999,
-8.40164026751963));
#36136=CARTESIAN_POINT('Ctrl Pts',(-4.85068927010199,-110.354517970999,
-8.4016402675109));
#36137=CARTESIAN_POINT('Ctrl Pts',(-7.27603390513785,-110.179517970999,
-4.20082013374671));
#36138=CARTESIAN_POINT('Ctrl Pts',(-9.70137854017372,-110.004517970999,
1.74701493417668E-11));
#36139=CARTESIAN_POINT('Ctrl Pts',(-7.27603390512272,-109.829517970999,
4.20082013377292));
#36140=CARTESIAN_POINT('Ctrl Pts',(-4.85068927007173,-109.654517970999,
8.40164026752836));
#36141=CARTESIAN_POINT('Ctrl Pts',(1.5129078685785E-11,-109.479517970999,
8.40164026751963));
#36142=CARTESIAN_POINT('Ctrl Pts',(4.85068927010198,-109.304517970999,8.4016402675109));
#36143=CARTESIAN_POINT('Ctrl Pts',(7.27603390513785,-109.129517970999,4.20082013374672));
#36144=CARTESIAN_POINT('Ctrl Pts',(9.70137854017372,-108.954517970999,-1.74689612655491E-11));
#36145=CARTESIAN_POINT('Ctrl Pts',(7.27603390512273,-108.779517970999,-4.20082013377291));
#36146=CARTESIAN_POINT('Ctrl Pts',(4.85068927007173,-108.604517970999,-8.40164026752836));
#36147=CARTESIAN_POINT('Ctrl Pts',(-1.51301075899711E-11,-108.429517970999,
-8.40164026751963));
#36148=CARTESIAN_POINT('Ctrl Pts',(-4.85068927010199,-108.254517970999,
-8.4016402675109));
#36149=CARTESIAN_POINT('Ctrl Pts',(-7.27603390513785,-108.079517970999,
-4.20082013374671));
#36150=CARTESIAN_POINT('Ctrl Pts',(-9.70137854017372,-107.904517970999,
1.74701493417668E-11));
#36151=CARTESIAN_POINT('Ctrl Pts',(-7.27603390512272,-107.729517970999,
4.20082013377292));
#36152=CARTESIAN_POINT('Ctrl Pts',(-4.85068927007173,-107.554517970999,
8.40164026752836));
#36153=CARTESIAN_POINT('Ctrl Pts',(1.5129078685785E-11,-107.379517970999,
8.40164026751963));
#36154=CARTESIAN_POINT('Ctrl Pts',(4.85068927010198,-107.204517970999,8.4016402675109));
#36155=CARTESIAN_POINT('Ctrl Pts',(7.27603390513785,-107.029517970999,4.20082013374672));
#36156=CARTESIAN_POINT('Ctrl Pts',(9.70137854017372,-106.854517970999,-1.74689612655491E-11));
#36157=CARTESIAN_POINT('Ctrl Pts',(7.27603390512273,-106.679517970999,-4.20082013377291));
#36158=CARTESIAN_POINT('Ctrl Pts',(4.85068927007173,-106.504517970998,-8.40164026752836));
#36159=CARTESIAN_POINT('Ctrl Pts',(-1.51301075899711E-11,-106.329517970999,
-8.40164026751963));
#36160=CARTESIAN_POINT('Ctrl Pts',(-4.85068927010199,-106.154517970999,
-8.4016402675109));
#36161=CARTESIAN_POINT('Ctrl Pts',(-7.27603390513785,-105.979517970999,
-4.20082013374671));
#36162=CARTESIAN_POINT('Ctrl Pts',(-9.70137854017372,-105.804517970999,
1.74701493417668E-11));
#36163=CARTESIAN_POINT('Ctrl Pts',(-7.27603390512272,-105.629517970999,
4.20082013377292));
#36164=CARTESIAN_POINT('Ctrl Pts',(-4.85068927007173,-105.454517970999,
8.40164026752836));
#36165=CARTESIAN_POINT('Ctrl Pts',(1.5129078685785E-11,-105.279517970999,
8.40164026751963));
#36166=CARTESIAN_POINT('Ctrl Pts',(4.85068927010198,-105.104517970999,8.4016402675109));
#36167=CARTESIAN_POINT('Ctrl Pts',(7.27603390513785,-104.929517970999,4.20082013374672));
#36168=CARTESIAN_POINT('Ctrl Pts',(9.70137854017372,-104.754517970999,-1.74689612655491E-11));
#36169=CARTESIAN_POINT('Ctrl Pts',(7.27603390512273,-104.579517970999,-4.20082013377291));
#36170=CARTESIAN_POINT('Ctrl Pts',(4.85068927007173,-104.404517970999,-8.40164026752836));
#36171=CARTESIAN_POINT('Ctrl Pts',(-1.51301075899711E-11,-104.229517970999,
-8.40164026751963));
#36172=CARTESIAN_POINT('Ctrl Pts',(-4.85068927010199,-104.054517970999,
-8.4016402675109));
#36173=CARTESIAN_POINT('Ctrl Pts',(-7.27603390513785,-103.879517970999,
-4.20082013374671));
#36174=CARTESIAN_POINT('Ctrl Pts',(-9.70137854017372,-103.704517970999,
1.74701493417668E-11));
#36175=CARTESIAN_POINT('Ctrl Pts',(-7.27603390512272,-103.529517970999,
4.20082013377292));
#36176=CARTESIAN_POINT('Ctrl Pts',(-4.85068927007173,-103.354517970999,
8.40164026752836));
#36177=CARTESIAN_POINT('Ctrl Pts',(1.5129078685785E-11,-103.179517970999,
8.40164026751963));
#36178=CARTESIAN_POINT('Ctrl Pts',(4.85068927010198,-103.004517970999,8.4016402675109));
#36179=CARTESIAN_POINT('Ctrl Pts',(7.27603390513785,-102.829517970999,4.20082013374672));
#36180=CARTESIAN_POINT('Ctrl Pts',(9.70137854017372,-102.654517970999,-1.74689612655491E-11));
#36181=CARTESIAN_POINT('Ctrl Pts',(7.27603390512273,-102.479517970999,-4.20082013377291));
#36182=CARTESIAN_POINT('Ctrl Pts',(4.85068927007173,-102.304517970999,-8.40164026752836));
#36183=CARTESIAN_POINT('Ctrl Pts',(-1.51301075899711E-11,-102.129517970999,
-8.40164026751963));
#36184=CARTESIAN_POINT('Ctrl Pts',(-4.85068927010199,-101.954517970999,
-8.4016402675109));
#36185=CARTESIAN_POINT('Ctrl Pts',(-7.27603390513785,-101.779517970999,
-4.20082013374671));
#36186=CARTESIAN_POINT('Ctrl Pts',(-9.70137854017372,-101.604517970999,
1.74701493417668E-11));
#36187=CARTESIAN_POINT('Ctrl Pts',(-7.27603390512272,-101.429517970999,
4.20082013377292));
#36188=CARTESIAN_POINT('Ctrl Pts',(-4.85068927007173,-101.254517970999,
8.40164026752836));
#36189=CARTESIAN_POINT('Ctrl Pts',(1.5129078685785E-11,-101.079517970999,
8.40164026751963));
#36190=CARTESIAN_POINT('Ctrl Pts',(4.85068927010198,-100.904517970999,8.4016402675109));
#36191=CARTESIAN_POINT('Ctrl Pts',(7.27603390513785,-100.729517970999,4.20082013374672));
#36192=CARTESIAN_POINT('Ctrl Pts',(9.70137854017372,-100.554517970999,-1.74689612655491E-11));
#36193=CARTESIAN_POINT('Ctrl Pts',(7.27603390512273,-100.379517970999,-4.20082013377291));
#36194=CARTESIAN_POINT('Ctrl Pts',(4.85068927007173,-100.204517970999,-8.40164026752836));
#36195=CARTESIAN_POINT('Ctrl Pts',(-1.51301075899711E-11,-100.029517970999,
-8.40164026751963));
#36196=CARTESIAN_POINT('Ctrl Pts',(-4.85068927010199,-99.8545179709986,
-8.4016402675109));
#36197=CARTESIAN_POINT('Ctrl Pts',(-7.27603390513785,-99.6795179709985,
-4.20082013374671));
#36198=CARTESIAN_POINT('Ctrl Pts',(-9.70137854017372,-99.5045179709985,
1.74701493417668E-11));
#36199=CARTESIAN_POINT('Ctrl Pts',(-7.27603390512272,-99.3295179709985,
4.20082013377292));
#36200=CARTESIAN_POINT('Ctrl Pts',(-4.85068927007173,-99.1545179709985,
8.40164026752836));
#36201=CARTESIAN_POINT('Ctrl Pts',(1.5129078685785E-11,-98.9795179709985,
8.40164026751963));
#36202=CARTESIAN_POINT('Ctrl Pts',(4.85068927010198,-98.8045179709985,8.4016402675109));
#36203=CARTESIAN_POINT('Ctrl Pts',(7.27603390513785,-98.6295179709985,4.20082013374672));
#36204=CARTESIAN_POINT('Ctrl Pts',(9.70137854017372,-98.4545179709986,-1.74689612655491E-11));
#36205=CARTESIAN_POINT('Ctrl Pts',(7.27603390512273,-98.2795179709986,-4.20082013377291));
#36206=CARTESIAN_POINT('Ctrl Pts',(4.85068927007173,-98.1045179709986,-8.40164026752836));
#36207=CARTESIAN_POINT('Ctrl Pts',(-1.51301075899711E-11,-97.9295179709985,
-8.40164026751963));
#36208=CARTESIAN_POINT('Ctrl Pts',(-4.85068927010199,-97.7545179709985,
-8.4016402675109));
#36209=CARTESIAN_POINT('Ctrl Pts',(-7.27603390513785,-97.5795179709986,
-4.20082013374671));
#36210=CARTESIAN_POINT('Ctrl Pts',(-9.70137854017372,-97.4045179709985,
1.74701493417668E-11));
#36211=CARTESIAN_POINT('Ctrl Pts',(-7.27603390512272,-97.2295179709985,
4.20082013377292));
#36212=CARTESIAN_POINT('Ctrl Pts',(-4.85068927007173,-97.0545179709985,
8.40164026752836));
#36213=CARTESIAN_POINT('Ctrl Pts',(1.5129078685785E-11,-96.8795179709986,
8.40164026751963));
#36214=CARTESIAN_POINT('Ctrl Pts',(4.85068927010198,-96.7045179709986,8.4016402675109));
#36215=CARTESIAN_POINT('Ctrl Pts',(7.27603390513785,-96.5295179709985,4.20082013374672));
#36216=CARTESIAN_POINT('Ctrl Pts',(9.70137854017372,-96.3545179709985,-1.74689612655491E-11));
#36217=CARTESIAN_POINT('Ctrl Pts',(7.27603390512273,-96.1795179709985,-4.20082013377291));
#36218=CARTESIAN_POINT('Ctrl Pts',(4.85068927007173,-96.0045179709986,-8.40164026752836));
#36219=CARTESIAN_POINT('Ctrl Pts',(-1.51301075899711E-11,-95.8295179709985,
-8.40164026751963));
#36220=CARTESIAN_POINT('Ctrl Pts',(-4.85068927010199,-95.6545179709985,
-8.4016402675109));
#36221=CARTESIAN_POINT('Ctrl Pts',(-7.27603390513785,-95.4795179709985,
-4.20082013374671));
#36222=CARTESIAN_POINT('Ctrl Pts',(-9.70137854017372,-95.3045179709986,
1.74701493417668E-11));
#36223=CARTESIAN_POINT('Ctrl Pts',(-7.27603390512272,-95.1295179709986,
4.20082013377292));
#36224=CARTESIAN_POINT('Ctrl Pts',(-4.85068927007173,-94.9545179709986,
8.40164026752836));
#36225=CARTESIAN_POINT('Ctrl Pts',(1.5129078685785E-11,-94.7795179709985,
8.40164026751963));
#36226=CARTESIAN_POINT('Ctrl Pts',(4.85068927010198,-94.6045179709986,8.4016402675109));
#36227=CARTESIAN_POINT('Ctrl Pts',(7.27603390513785,-94.4295179709985,4.20082013374672));
#36228=CARTESIAN_POINT('Ctrl Pts',(9.70137854017372,-94.2545179709985,-1.74689612655491E-11));
#36229=CARTESIAN_POINT('Ctrl Pts',(7.27603390512273,-94.0795179709986,-4.20082013377291));
#36230=CARTESIAN_POINT('Ctrl Pts',(4.85068927007173,-93.9045179709986,-8.40164026752836));
#36231=CARTESIAN_POINT('Ctrl Pts',(-1.51301075899711E-11,-93.7295179709986,
-8.40164026751963));
#36232=CARTESIAN_POINT('Ctrl Pts',(-4.85068927010199,-93.5545179709985,
-8.4016402675109));
#36233=CARTESIAN_POINT('Ctrl Pts',(-7.27603390513785,-93.3795179709985,
-4.20082013374671));
#36234=CARTESIAN_POINT('Ctrl Pts',(-9.70137854017372,-93.2045179709986,
1.74701493417668E-11));
#36235=CARTESIAN_POINT('Ctrl Pts',(-7.27603390512272,-93.0295179709986,
4.20082013377292));
#36236=CARTESIAN_POINT('Ctrl Pts',(-4.85068927007173,-92.8545179709985,
8.40164026752836));
#36237=CARTESIAN_POINT('Ctrl Pts',(1.5129078685785E-11,-92.6795179709985,
8.40164026751963));
#36238=CARTESIAN_POINT('Ctrl Pts',(4.85068927010198,-92.5045179709985,8.4016402675109));
#36239=CARTESIAN_POINT('Ctrl Pts',(7.27603390513785,-92.3295179709986,4.20082013374672));
#36240=CARTESIAN_POINT('Ctrl Pts',(9.70137854017372,-92.1545179709986,-1.74689612655491E-11));
#36241=CARTESIAN_POINT('Ctrl Pts',(7.27603390512273,-91.9795179709986,-4.20082013377291));
#36242=CARTESIAN_POINT('Ctrl Pts',(4.85068927007173,-91.8045179709985,-8.40164026752836));
#36243=CARTESIAN_POINT('Ctrl Pts',(-1.51301075899711E-11,-91.6295179709986,
-8.40164026751963));
#36244=CARTESIAN_POINT('Ctrl Pts',(-4.85068927010199,-91.4545179709986,
-8.4016402675109));
#36245=CARTESIAN_POINT('Ctrl Pts',(-7.27603390513785,-91.2795179709986,
-4.20082013374671));
#36246=CARTESIAN_POINT('Ctrl Pts',(-9.70137854017372,-91.1045179709985,
1.74701493417668E-11));
#36247=CARTESIAN_POINT('Ctrl Pts',(-7.27603390512272,-90.9295179709986,
4.20082013377292));
#36248=CARTESIAN_POINT('Ctrl Pts',(-4.85068927007173,-90.7545179709986,
8.40164026752836));
#36249=CARTESIAN_POINT('Ctrl Pts',(1.5129078685785E-11,-90.5795179709986,
8.40164026751963));
#36250=CARTESIAN_POINT('Ctrl Pts',(4.85068927010198,-90.4045179709985,8.4016402675109));
#36251=CARTESIAN_POINT('Ctrl Pts',(7.27603390513785,-90.2295179709986,4.20082013374672));
#36252=CARTESIAN_POINT('Ctrl Pts',(9.70137854017372,-90.0545179709986,-1.74689612655491E-11));
#36253=CARTESIAN_POINT('Ctrl Pts',(7.27603390512273,-89.8795179709985,-4.20082013377291));
#36254=CARTESIAN_POINT('Ctrl Pts',(4.85068927007173,-89.7045179709986,-8.40164026752836));
#36255=CARTESIAN_POINT('Ctrl Pts',(-1.51301075899711E-11,-89.5295179709986,
-8.40164026751963));
#36256=CARTESIAN_POINT('Ctrl Pts',(-4.85068927010199,-89.3545179709986,
-8.4016402675109));
#36257=CARTESIAN_POINT('Ctrl Pts',(-7.27603390513785,-89.1795179709986,
-4.20082013374671));
#36258=CARTESIAN_POINT('Ctrl Pts',(-9.70137854017372,-89.0045179709985,
1.74701493417668E-11));
#36259=CARTESIAN_POINT('Ctrl Pts',(-7.27603390512272,-88.8295179709986,
4.20082013377292));
#36260=CARTESIAN_POINT('Ctrl Pts',(-4.85068927007173,-88.6545179709986,
8.40164026752836));
#36261=CARTESIAN_POINT('Ctrl Pts',(1.5129078685785E-11,-88.4795179709986,
8.40164026751963));
#36262=CARTESIAN_POINT('Ctrl Pts',(4.85068927010198,-88.3045179709985,8.4016402675109));
#36263=CARTESIAN_POINT('Ctrl Pts',(7.27603390513785,-88.1295179709985,4.20082013374672));
#36264=CARTESIAN_POINT('Ctrl Pts',(9.70137854017372,-87.9545179709986,-1.74689612655491E-11));
#36265=CARTESIAN_POINT('Ctrl Pts',(7.27603390512273,-87.7795179709986,-4.20082013377291));
#36266=CARTESIAN_POINT('Ctrl Pts',(4.85068927007173,-87.6045179709986,-8.40164026752836));
#36267=CARTESIAN_POINT('Ctrl Pts',(-1.51301075899711E-11,-87.4295179709986,
-8.40164026751963));
#36268=CARTESIAN_POINT('Ctrl Pts',(-4.85068927010199,-87.2545179709986,
-8.4016402675109));
#36269=CARTESIAN_POINT('Ctrl Pts',(-7.27603390513785,-87.0795179709986,
-4.20082013374671));
#36270=CARTESIAN_POINT('Ctrl Pts',(-9.70137854017372,-86.9045179709986,
1.74701493417668E-11));
#36271=CARTESIAN_POINT('Ctrl Pts',(-7.27603390512272,-86.7295179709986,
4.20082013377292));
#36272=CARTESIAN_POINT('Ctrl Pts',(-4.85068927007173,-86.5545179709986,
8.40164026752836));
#36273=CARTESIAN_POINT('Ctrl Pts',(1.5129078685785E-11,-86.3795179709986,
8.40164026751963));
#36274=CARTESIAN_POINT('Ctrl Pts',(4.85068927010198,-86.2045179709986,8.4016402675109));
#36275=CARTESIAN_POINT('Ctrl Pts',(7.27603390513785,-86.0295179709986,4.20082013374672));
#36276=CARTESIAN_POINT('Ctrl Pts',(9.70137854017372,-85.8545179709986,-1.74689612655491E-11));
#36277=CARTESIAN_POINT('Ctrl Pts',(7.27603390512273,-85.6795179709986,-4.20082013377291));
#36278=CARTESIAN_POINT('Ctrl Pts',(4.85068927007173,-85.5045179709986,-8.40164026752836));
#36279=CARTESIAN_POINT('Ctrl Pts',(-1.51301075899711E-11,-85.3295179709986,
-8.40164026751963));
#36280=CARTESIAN_POINT('Ctrl Pts',(-4.85068927010199,-85.1545179709986,
-8.4016402675109));
#36281=CARTESIAN_POINT('Ctrl Pts',(-7.27603390513785,-84.9795179709986,
-4.20082013374671));
#36282=CARTESIAN_POINT('Ctrl Pts',(-9.70137854017372,-84.8045179709986,
1.74701493417668E-11));
#36283=CARTESIAN_POINT('Ctrl Pts',(-7.27603390512272,-84.6295179709986,
4.20082013377292));
#36284=CARTESIAN_POINT('Ctrl Pts',(-4.85068927007173,-84.4545179709986,
8.40164026752836));
#36285=CARTESIAN_POINT('Ctrl Pts',(1.5129078685785E-11,-84.2795179709986,
8.40164026751963));
#36286=CARTESIAN_POINT('Ctrl Pts',(4.85068927010198,-84.1045179709986,8.4016402675109));
#36287=CARTESIAN_POINT('Ctrl Pts',(7.27603390513785,-83.9295179709986,4.20082013374672));
#36288=CARTESIAN_POINT('Ctrl Pts',(9.70137854017372,-83.7545179709985,-1.74689612655491E-11));
#36289=CARTESIAN_POINT('Ctrl Pts',(7.27603390512273,-83.5795179709986,-4.20082013377291));
#36290=CARTESIAN_POINT('Ctrl Pts',(4.85068927007173,-83.4045179709986,-8.40164026752836));
#36291=CARTESIAN_POINT('Ctrl Pts',(-1.51301075899711E-11,-83.2295179709986,
-8.40164026751963));
#36292=CARTESIAN_POINT('Ctrl Pts',(-4.85068927010199,-83.0545179709986,
-8.4016402675109));
#36293=CARTESIAN_POINT('Ctrl Pts',(-7.27603390513785,-82.8795179709986,
-4.20082013374671));
#36294=CARTESIAN_POINT('Ctrl Pts',(-9.70137854017372,-82.7045179709986,
1.74701493417668E-11));
#36295=CARTESIAN_POINT('Ctrl Pts',(-7.27603390512272,-82.5295179709986,
4.20082013377292));
#36296=CARTESIAN_POINT('Ctrl Pts',(-4.85068927007173,-82.3545179709986,
8.40164026752836));
#36297=CARTESIAN_POINT('Ctrl Pts',(1.5129078685785E-11,-82.1795179709986,
8.40164026751963));
#36298=CARTESIAN_POINT('Ctrl Pts',(4.85068927010198,-82.0045179709986,8.4016402675109));
#36299=CARTESIAN_POINT('Ctrl Pts',(7.27603390513785,-81.8295179709986,4.20082013374672));
#36300=CARTESIAN_POINT('Ctrl Pts',(9.70137854017372,-81.6545179709986,-1.74689612655491E-11));
#36301=CARTESIAN_POINT('Ctrl Pts',(7.27603390512273,-81.4795179709986,-4.20082013377291));
#36302=CARTESIAN_POINT('Ctrl Pts',(4.85068927007173,-81.3045179709986,-8.40164026752836));
#36303=CARTESIAN_POINT('Ctrl Pts',(-1.51301075899711E-11,-81.1295179709986,
-8.40164026751963));
#36304=CARTESIAN_POINT('Ctrl Pts',(-4.85068927010199,-80.9545179709986,
-8.4016402675109));
#36305=CARTESIAN_POINT('Ctrl Pts',(-7.27603390513785,-80.7795179709986,
-4.20082013374671));
#36306=CARTESIAN_POINT('Ctrl Pts',(-9.70137854017372,-80.6045179709986,
1.74701493417668E-11));
#36307=CARTESIAN_POINT('Ctrl Pts',(-7.27603390512272,-80.4295179709986,
4.20082013377292));
#36308=CARTESIAN_POINT('Ctrl Pts',(-4.85068927007173,-80.2545179709986,
8.40164026752836));
#36309=CARTESIAN_POINT('Ctrl Pts',(1.5129078685785E-11,-80.0795179709986,
8.40164026751963));
#36310=CARTESIAN_POINT('Ctrl Pts',(4.85068927010198,-79.9045179709986,8.4016402675109));
#36311=CARTESIAN_POINT('Ctrl Pts',(7.27603390513785,-79.7295179709986,4.20082013374672));
#36312=CARTESIAN_POINT('Ctrl Pts',(9.70137854017372,-79.5545179709986,-1.74689612655491E-11));
#36313=CARTESIAN_POINT('Ctrl Pts',(7.27603390512273,-79.3795179709986,-4.20082013377291));
#36314=CARTESIAN_POINT('Ctrl Pts',(4.85068927007173,-79.2045179709986,-8.40164026752836));
#36315=CARTESIAN_POINT('Ctrl Pts',(-1.51301075899711E-11,-79.0295179709986,
-8.40164026751963));
#36316=CARTESIAN_POINT('Ctrl Pts',(-4.85068927010199,-78.8545179709986,
-8.4016402675109));
#36317=CARTESIAN_POINT('Ctrl Pts',(-7.27603390513785,-78.6795179709986,
-4.20082013374671));
#36318=CARTESIAN_POINT('Ctrl Pts',(-9.70137854017372,-78.5045179709986,
1.74701493417668E-11));
#36319=CARTESIAN_POINT('Ctrl Pts',(-7.27603390512272,-78.3295179709986,
4.20082013377292));
#36320=CARTESIAN_POINT('Ctrl Pts',(-4.85068927007173,-78.1545179709986,
8.40164026752836));
#36321=CARTESIAN_POINT('Ctrl Pts',(1.5129078685785E-11,-77.9795179709986,
8.40164026751963));
#36322=CARTESIAN_POINT('Ctrl Pts',(4.85068927010198,-77.8045179709986,8.4016402675109));
#36323=CARTESIAN_POINT('Ctrl Pts',(7.27603390513785,-77.6295179709986,4.20082013374672));
#36324=CARTESIAN_POINT('Ctrl Pts',(9.70137854017372,-77.4545179709986,-1.74689612655491E-11));
#36325=CARTESIAN_POINT('Ctrl Pts',(7.27603390512273,-77.2795179709986,-4.20082013377291));
#36326=CARTESIAN_POINT('Ctrl Pts',(4.85068927007173,-77.1045179709986,-8.40164026752836));
#36327=CARTESIAN_POINT('Ctrl Pts',(-1.51301075899711E-11,-76.9295179709986,
-8.40164026751963));
#36328=CARTESIAN_POINT('Ctrl Pts',(-4.85068927010199,-76.7545179709986,
-8.4016402675109));
#36329=CARTESIAN_POINT('Ctrl Pts',(-7.27603390513785,-76.5795179709986,
-4.20082013374671));
#36330=CARTESIAN_POINT('Ctrl Pts',(-9.70137854017372,-76.4045179709986,
1.74701493417668E-11));
#36331=CARTESIAN_POINT('Ctrl Pts',(-7.27603390512272,-76.2295179709986,
4.20082013377292));
#36332=CARTESIAN_POINT('Ctrl Pts',(-4.85068927007173,-76.0545179709986,
8.40164026752836));
#36333=CARTESIAN_POINT('Ctrl Pts',(1.5129078685785E-11,-75.8795179709986,
8.40164026751963));
#36334=CARTESIAN_POINT('Ctrl Pts',(4.85068927010198,-75.7045179709986,8.4016402675109));
#36335=CARTESIAN_POINT('Ctrl Pts',(7.27603390513785,-75.5295179709986,4.20082013374672));
#36336=CARTESIAN_POINT('Ctrl Pts',(9.70137854017372,-75.3545179709986,-1.74689612655491E-11));
#36337=CARTESIAN_POINT('Ctrl Pts',(7.27603390512273,-75.1795179709986,-4.20082013377291));
#36338=CARTESIAN_POINT('Ctrl Pts',(4.85068927007173,-75.0045179709986,-8.40164026752836));
#36339=CARTESIAN_POINT('Ctrl Pts',(-1.51301075899711E-11,-74.8295179709986,
-8.40164026751963));
#36340=CARTESIAN_POINT('Ctrl Pts',(-4.85068927010199,-74.6545179709986,
-8.4016402675109));
#36341=CARTESIAN_POINT('Ctrl Pts',(-7.27603390513785,-74.4795179709986,
-4.20082013374671));
#36342=CARTESIAN_POINT('Ctrl Pts',(-9.70137854017372,-74.3045179709986,
1.74701493417668E-11));
#36343=CARTESIAN_POINT('Ctrl Pts',(-7.27603390512272,-74.1295179709986,
4.20082013377292));
#36344=CARTESIAN_POINT('Ctrl Pts',(-4.85068927007173,-73.9545179709986,
8.40164026752836));
#36345=CARTESIAN_POINT('Ctrl Pts',(1.5129078685785E-11,-73.7795179709986,
8.40164026751963));
#36346=CARTESIAN_POINT('Ctrl Pts',(4.85068927010198,-73.6045179709986,8.4016402675109));
#36347=CARTESIAN_POINT('Ctrl Pts',(7.27603390513785,-73.4295179709986,4.20082013374672));
#36348=CARTESIAN_POINT('Ctrl Pts',(9.70137854017372,-73.2545179709986,-1.74689612655491E-11));
#36349=CARTESIAN_POINT('Ctrl Pts',(7.27603390512273,-73.0795179709986,-4.20082013377291));
#36350=CARTESIAN_POINT('Ctrl Pts',(4.85068927007173,-72.9045179709986,-8.40164026752836));
#36351=CARTESIAN_POINT('Ctrl Pts',(-1.51301075899711E-11,-72.7295179709986,
-8.40164026751963));
#36352=CARTESIAN_POINT('Ctrl Pts',(-4.85068927010199,-72.5545179709986,
-8.4016402675109));
#36353=CARTESIAN_POINT('Ctrl Pts',(-7.27603390513785,-72.3795179709986,
-4.20082013374671));
#36354=CARTESIAN_POINT('Ctrl Pts',(-9.70137854017372,-72.2045179709986,
1.74701493417668E-11));
#36355=CARTESIAN_POINT('Ctrl Pts',(-7.27603390512272,-72.0295179709986,
4.20082013377292));
#36356=CARTESIAN_POINT('Ctrl Pts',(-4.85068927007173,-71.8545179709986,
8.40164026752836));
#36357=CARTESIAN_POINT('Ctrl Pts',(1.5129078685785E-11,-71.6795179709986,
8.40164026751963));
#36358=CARTESIAN_POINT('Ctrl Pts',(4.85068927010198,-71.5045179709986,8.4016402675109));
#36359=CARTESIAN_POINT('Ctrl Pts',(7.27603390513785,-71.3295179709986,4.20082013374672));
#36360=CARTESIAN_POINT('Ctrl Pts',(9.70137854017372,-71.1545179709986,-1.74689612655491E-11));
#36361=CARTESIAN_POINT('Ctrl Pts',(7.27603390512273,-70.9795179709986,-4.20082013377291));
#36362=CARTESIAN_POINT('Ctrl Pts',(4.85068927007173,-70.8045179709986,-8.40164026752836));
#36363=CARTESIAN_POINT('Ctrl Pts',(-1.51301075899711E-11,-70.6295179709986,
-8.40164026751963));
#36364=CARTESIAN_POINT('Ctrl Pts',(-4.85068927010199,-70.4545179709986,
-8.4016402675109));
#36365=CARTESIAN_POINT('Ctrl Pts',(-7.27603390513785,-70.2795179709986,
-4.20082013374671));
#36366=CARTESIAN_POINT('Ctrl Pts',(-9.70137854017372,-70.1045179709986,
1.74701493417668E-11));
#36367=CARTESIAN_POINT('Ctrl Pts',(-7.27603390512272,-69.9295179709986,
4.20082013377292));
#36368=CARTESIAN_POINT('Ctrl Pts',(-4.85068927007173,-69.7545179709986,
8.40164026752836));
#36369=CARTESIAN_POINT('Ctrl Pts',(1.5129078685785E-11,-69.5795179709986,
8.40164026751963));
#36370=CARTESIAN_POINT('Ctrl Pts',(4.85068927010198,-69.4045179709986,8.4016402675109));
#36371=CARTESIAN_POINT('Ctrl Pts',(7.27603390513785,-69.2295179709986,4.20082013374672));
#36372=CARTESIAN_POINT('Ctrl Pts',(9.70137854017372,-69.0545179709986,-1.74689612655491E-11));
#36373=CARTESIAN_POINT('Ctrl Pts',(7.27603390512273,-68.8795179709986,-4.20082013377291));
#36374=CARTESIAN_POINT('Ctrl Pts',(4.85068927007173,-68.7045179709986,-8.40164026752836));
#36375=CARTESIAN_POINT('Ctrl Pts',(-1.51301075899711E-11,-68.5295179709986,
-8.40164026751963));
#36376=CARTESIAN_POINT('Ctrl Pts',(-4.85068927010199,-68.3545179709986,
-8.4016402675109));
#36377=CARTESIAN_POINT('Ctrl Pts',(-7.27603390513785,-68.1795179709986,
-4.20082013374671));
#36378=CARTESIAN_POINT('Ctrl Pts',(-9.70137854017372,-68.0045179709986,
1.74701493417668E-11));
#36379=CARTESIAN_POINT('Ctrl Pts',(-7.27603390512272,-67.8295179709986,
4.20082013377292));
#36380=CARTESIAN_POINT('Ctrl Pts',(-4.85068927007173,-67.6545179709986,
8.40164026752836));
#36381=CARTESIAN_POINT('Ctrl Pts',(1.5129078685785E-11,-67.4795179709986,
8.40164026751963));
#36382=CARTESIAN_POINT('Ctrl Pts',(4.85068927010198,-67.3045179709986,8.4016402675109));
#36383=CARTESIAN_POINT('Ctrl Pts',(7.27603390513785,-67.1295179709986,4.20082013374672));
#36384=CARTESIAN_POINT('Ctrl Pts',(9.70137854017372,-66.9545179709986,-1.74689612655491E-11));
#36385=CARTESIAN_POINT('Ctrl Pts',(7.27603390512273,-66.7795179709986,-4.20082013377291));
#36386=CARTESIAN_POINT('Ctrl Pts',(4.85068927007173,-66.6045179709986,-8.40164026752836));
#36387=CARTESIAN_POINT('Ctrl Pts',(-1.51301075899711E-11,-66.4295179709986,
-8.40164026751963));
#36388=CARTESIAN_POINT('Ctrl Pts',(-4.85068927010199,-66.2545179709986,
-8.4016402675109));
#36389=CARTESIAN_POINT('Ctrl Pts',(-7.27603390513785,-66.0795179709986,
-4.20082013374671));
#36390=CARTESIAN_POINT('Ctrl Pts',(-9.70137854017372,-65.9045179709986,
1.74701493417668E-11));
#36391=CARTESIAN_POINT('Ctrl Pts',(-7.27603390512272,-65.7295179709986,
4.20082013377292));
#36392=CARTESIAN_POINT('Ctrl Pts',(-4.85068927007173,-65.5545179709986,
8.40164026752836));
#36393=CARTESIAN_POINT('Ctrl Pts',(1.5129078685785E-11,-65.3795179709986,
8.40164026751963));
#36394=CARTESIAN_POINT('Ctrl Pts',(4.85068927010198,-65.2045179709986,8.4016402675109));
#36395=CARTESIAN_POINT('Ctrl Pts',(7.27603390513785,-65.0295179709986,4.20082013374672));
#36396=CARTESIAN_POINT('Ctrl Pts',(9.70137854017372,-64.8545179709986,-1.74689612655491E-11));
#36397=CARTESIAN_POINT('Ctrl Pts',(7.27603390512273,-64.6795179709986,-4.20082013377291));
#36398=CARTESIAN_POINT('Ctrl Pts',(4.85068927007173,-64.5045179709986,-8.40164026752836));
#36399=CARTESIAN_POINT('Ctrl Pts',(-1.51301075899711E-11,-64.3295179709986,
-8.40164026751963));
#36400=CARTESIAN_POINT('Ctrl Pts',(-4.85068927010199,-64.1545179709986,
-8.4016402675109));
#36401=CARTESIAN_POINT('Ctrl Pts',(-7.27603390513785,-63.9795179709986,
-4.20082013374671));
#36402=CARTESIAN_POINT('Ctrl Pts',(-9.70137854017372,-63.8045179709986,
1.74701493417668E-11));
#36403=CARTESIAN_POINT('Ctrl Pts',(-7.27603390512272,-63.6295179709986,
4.20082013377292));
#36404=CARTESIAN_POINT('Ctrl Pts',(-4.85068927007173,-63.4545179709986,
8.40164026752836));
#36405=CARTESIAN_POINT('Ctrl Pts',(1.5129078685785E-11,-63.2795179709986,
8.40164026751963));
#36406=CARTESIAN_POINT('Ctrl Pts',(4.85068927010198,-63.1045179709986,8.4016402675109));
#36407=CARTESIAN_POINT('Ctrl Pts',(7.27603390513785,-62.9295179709986,4.20082013374672));
#36408=CARTESIAN_POINT('Ctrl Pts',(9.70137854017372,-62.7545179709986,-1.74689612655491E-11));
#36409=CARTESIAN_POINT('Ctrl Pts',(7.27603390512273,-62.5795179709986,-4.20082013377291));
#36410=CARTESIAN_POINT('Ctrl Pts',(4.85068927007173,-62.4045179709986,-8.40164026752836));
#36411=CARTESIAN_POINT('Ctrl Pts',(-1.51301075899711E-11,-62.2295179709986,
-8.40164026751963));
#36412=CARTESIAN_POINT('Ctrl Pts',(-4.85068927010199,-62.0545179709986,
-8.4016402675109));
#36413=CARTESIAN_POINT('Ctrl Pts',(-7.27603390513785,-61.8795179709986,
-4.20082013374671));
#36414=CARTESIAN_POINT('Ctrl Pts',(-9.70137854017372,-61.7045179709986,
1.74701493417668E-11));
#36415=CARTESIAN_POINT('Ctrl Pts',(-7.27603390512272,-61.5295179709986,
4.20082013377292));
#36416=CARTESIAN_POINT('Ctrl Pts',(-4.85068927007173,-61.3545179709986,
8.40164026752836));
#36417=CARTESIAN_POINT('Ctrl Pts',(1.5129078685785E-11,-61.1795179709986,
8.40164026751963));
#36418=CARTESIAN_POINT('Ctrl Pts',(4.85068927010198,-61.0045179709986,8.4016402675109));
#36419=CARTESIAN_POINT('Ctrl Pts',(7.27603390513785,-60.8295179709986,4.20082013374672));
#36420=CARTESIAN_POINT('Ctrl Pts',(9.70137854017372,-60.6545179709986,-1.74689612655491E-11));
#36421=CARTESIAN_POINT('Ctrl Pts',(7.27603390512273,-60.4795179709986,-4.20082013377291));
#36422=CARTESIAN_POINT('Ctrl Pts',(4.85068927007173,-60.3045179709986,-8.40164026752836));
#36423=CARTESIAN_POINT('Ctrl Pts',(-1.51301075899711E-11,-60.1295179709986,
-8.40164026751963));
#36424=CARTESIAN_POINT('Ctrl Pts',(-4.85068927010199,-59.9545179709986,
-8.4016402675109));
#36425=CARTESIAN_POINT('Ctrl Pts',(-7.27603390513785,-59.7795179709986,
-4.20082013374671));
#36426=CARTESIAN_POINT('Ctrl Pts',(-9.70137854017372,-59.6045179709986,
1.74701493417668E-11));
#36427=CARTESIAN_POINT('Ctrl Pts',(-7.27603390512272,-59.4295179709986,
4.20082013377292));
#36428=CARTESIAN_POINT('Ctrl Pts',(-4.85068927007173,-59.2545179709986,
8.40164026752836));
#36429=CARTESIAN_POINT('Ctrl Pts',(1.5129078685785E-11,-59.0795179709986,
8.40164026751963));
#36430=CARTESIAN_POINT('Ctrl Pts',(4.85068927010198,-58.9045179709986,8.4016402675109));
#36431=CARTESIAN_POINT('Ctrl Pts',(7.27603390513785,-58.7295179709986,4.20082013374672));
#36432=CARTESIAN_POINT('Ctrl Pts',(9.70137854017372,-58.5545179709986,-1.74689612655491E-11));
#36433=CARTESIAN_POINT('Ctrl Pts',(7.27603390512273,-58.3795179709986,-4.20082013377291));
#36434=CARTESIAN_POINT('Ctrl Pts',(4.85068927007173,-58.2045179709986,-8.40164026752836));
#36435=CARTESIAN_POINT('Ctrl Pts',(-1.51301075899711E-11,-58.0295179709986,
-8.40164026751963));
#36436=CARTESIAN_POINT('Ctrl Pts',(-4.85068927010199,-57.8545179709986,
-8.4016402675109));
#36437=CARTESIAN_POINT('Ctrl Pts',(-7.27603390513785,-57.6795179709986,
-4.20082013374671));
#36438=CARTESIAN_POINT('Ctrl Pts',(-9.70137854017372,-57.5045179709986,
1.74701493417668E-11));
#36439=CARTESIAN_POINT('Ctrl Pts',(-7.27603390512272,-57.3295179709986,
4.20082013377292));
#36440=CARTESIAN_POINT('Ctrl Pts',(-4.85068927007173,-57.1545179709986,
8.40164026752836));
#36441=CARTESIAN_POINT('Ctrl Pts',(1.5129078685785E-11,-56.9795179709986,
8.40164026751963));
#36442=CARTESIAN_POINT('Ctrl Pts',(4.85068927010198,-56.8045179709986,8.4016402675109));
#36443=CARTESIAN_POINT('Ctrl Pts',(7.27603390513785,-56.6295179709986,4.20082013374672));
#36444=CARTESIAN_POINT('Ctrl Pts',(9.70137854017372,-56.4545179709986,-1.74689612655491E-11));
#36445=CARTESIAN_POINT('Ctrl Pts',(7.27603390512273,-56.2795179709986,-4.20082013377291));
#36446=CARTESIAN_POINT('Ctrl Pts',(4.85068927007173,-56.1045179709986,-8.40164026752836));
#36447=CARTESIAN_POINT('Ctrl Pts',(-1.51301075899711E-11,-55.9295179709986,
-8.40164026751963));
#36448=CARTESIAN_POINT('Ctrl Pts',(-4.85068927010199,-55.7545179709987,
-8.4016402675109));
#36449=CARTESIAN_POINT('Ctrl Pts',(-7.27603390513785,-55.5795179709986,
-4.20082013374671));
#36450=CARTESIAN_POINT('Ctrl Pts',(-9.70137854017372,-55.4045179709986,
1.74701493417668E-11));
#36451=CARTESIAN_POINT('Ctrl Pts',(-7.27603390512272,-55.2295179709986,
4.20082013377292));
#36452=CARTESIAN_POINT('Ctrl Pts',(-4.85068927007173,-55.0545179709987,
8.40164026752836));
#36453=CARTESIAN_POINT('Ctrl Pts',(1.5129078685785E-11,-54.8795179709986,
8.40164026751963));
#36454=CARTESIAN_POINT('Ctrl Pts',(4.85068927010198,-54.7045179709987,8.4016402675109));
#36455=CARTESIAN_POINT('Ctrl Pts',(7.27603390513785,-54.5295179709986,4.20082013374672));
#36456=CARTESIAN_POINT('Ctrl Pts',(9.70137854017372,-54.3545179709986,-1.74689612655491E-11));
#36457=CARTESIAN_POINT('Ctrl Pts',(7.27603390512273,-54.1795179709986,-4.20082013377291));
#36458=CARTESIAN_POINT('Ctrl Pts',(4.85068927007173,-54.0045179709987,-8.40164026752836));
#36459=CARTESIAN_POINT('Ctrl Pts',(-1.51301075899711E-11,-53.8295179709986,
-8.40164026751963));
#36460=CARTESIAN_POINT('Ctrl Pts',(-4.85068927010199,-53.6545179709986,
-8.4016402675109));
#36461=CARTESIAN_POINT('Ctrl Pts',(-7.27603390513785,-53.4795179709987,
-4.20082013374671));
#36462=CARTESIAN_POINT('Ctrl Pts',(-9.70137854017372,-53.3045179709987,
1.74701493417668E-11));
#36463=CARTESIAN_POINT('Ctrl Pts',(-7.27603390512272,-53.1295179709986,
4.20082013377292));
#36464=CARTESIAN_POINT('Ctrl Pts',(-4.85068927007173,-52.9545179709987,
8.40164026752836));
#36465=CARTESIAN_POINT('Ctrl Pts',(1.5129078685785E-11,-52.7795179709986,
8.40164026751963));
#36466=CARTESIAN_POINT('Ctrl Pts',(4.85068927010198,-52.6045179709986,8.4016402675109));
#36467=CARTESIAN_POINT('Ctrl Pts',(7.27603390513785,-52.4295179709987,4.20082013374672));
#36468=CARTESIAN_POINT('Ctrl Pts',(9.70137854017372,-52.2545179709986,-1.74689612655491E-11));
#36469=CARTESIAN_POINT('Ctrl Pts',(7.27603390512273,-52.0795179709986,-4.20082013377291));
#36470=CARTESIAN_POINT('Ctrl Pts',(4.85068927007173,-51.9045179709987,-8.40164026752836));
#36471=CARTESIAN_POINT('Ctrl Pts',(-1.51301075899711E-11,-51.7295179709986,
-8.40164026751963));
#36472=CARTESIAN_POINT('Ctrl Pts',(-4.85068927010199,-51.5545179709986,
-8.4016402675109));
#36473=CARTESIAN_POINT('Ctrl Pts',(-7.27603390513785,-51.3795179709987,
-4.20082013374671));
#36474=CARTESIAN_POINT('Ctrl Pts',(-9.70137854017372,-51.2045179709987,
1.74701493417668E-11));
#36475=CARTESIAN_POINT('Ctrl Pts',(-7.27603390512272,-51.0295179709986,
4.20082013377292));
#36476=CARTESIAN_POINT('Ctrl Pts',(-4.85068927007173,-50.8545179709987,
8.40164026752836));
#36477=CARTESIAN_POINT('Ctrl Pts',(1.5129078685785E-11,-50.6795179709987,
8.40164026751963));
#36478=CARTESIAN_POINT('Ctrl Pts',(4.85068927010198,-50.5045179709986,8.4016402675109));
#36479=CARTESIAN_POINT('Ctrl Pts',(7.27603390513785,-50.3295179709987,4.20082013374672));
#36480=CARTESIAN_POINT('Ctrl Pts',(9.70137854017372,-50.1545179709987,-1.74689612655491E-11));
#36481=CARTESIAN_POINT('Ctrl Pts',(7.27603390512273,-49.9795179709986,-4.20082013377291));
#36482=CARTESIAN_POINT('Ctrl Pts',(4.85068927007173,-49.8045179709986,-8.40164026752836));
#36483=CARTESIAN_POINT('Ctrl Pts',(-1.51301075899711E-11,-49.6295179709987,
-8.40164026751963));
#36484=CARTESIAN_POINT('Ctrl Pts',(-4.85068927010199,-49.4545179709986,
-8.4016402675109));
#36485=CARTESIAN_POINT('Ctrl Pts',(-7.27603390513785,-49.2795179709986,
-4.20082013374671));
#36486=CARTESIAN_POINT('Ctrl Pts',(-9.70137854017372,-49.1045179709987,
1.74701493417668E-11));
#36487=CARTESIAN_POINT('Ctrl Pts',(-7.27603390512272,-48.9295179709987,
4.20082013377292));
#36488=CARTESIAN_POINT('Ctrl Pts',(-4.85068927007173,-48.7545179709986,
8.40164026752836));
#36489=CARTESIAN_POINT('Ctrl Pts',(1.5129078685785E-11,-48.5795179709987,
8.40164026751963));
#36490=CARTESIAN_POINT('Ctrl Pts',(4.85068927010198,-48.4045179709987,8.4016402675109));
#36491=CARTESIAN_POINT('Ctrl Pts',(7.27603390513785,-48.2295179709986,4.20082013374672));
#36492=CARTESIAN_POINT('Ctrl Pts',(9.70137854017372,-48.0545179709987,-1.74689612655491E-11));
#36493=CARTESIAN_POINT('Ctrl Pts',(7.27603390512273,-47.8795179709987,-4.20082013377291));
#36494=CARTESIAN_POINT('Ctrl Pts',(4.85068927007173,-47.7045179709986,-8.40164026752836));
#36495=CARTESIAN_POINT('Ctrl Pts',(-1.51301075899711E-11,-47.5295179709987,
-8.40164026751963));
#36496=CARTESIAN_POINT('Ctrl Pts',(-4.85068927010199,-47.3545179709987,
-8.4016402675109));
#36497=CARTESIAN_POINT('Ctrl Pts',(-7.27603390513785,-47.1795179709986,
-4.20082013374671));
#36498=CARTESIAN_POINT('Ctrl Pts',(-9.70137854017372,-47.0045179709987,
1.74701493417668E-11));
#36499=CARTESIAN_POINT('Ctrl Pts',(-7.27603390512272,-46.8295179709987,
4.20082013377292));
#36500=CARTESIAN_POINT('Ctrl Pts',(-4.85068927007173,-46.6545179709987,
8.40164026752836));
#36501=CARTESIAN_POINT('Ctrl Pts',(1.5129078685785E-11,-46.4795179709987,
8.40164026751963));
#36502=CARTESIAN_POINT('Ctrl Pts',(4.85068927010198,-46.3045179709987,8.4016402675109));
#36503=CARTESIAN_POINT('Ctrl Pts',(7.27603390513785,-46.1295179709986,4.20082013374672));
#36504=CARTESIAN_POINT('Ctrl Pts',(9.70137854017372,-45.9545179709987,-1.74689612655491E-11));
#36505=CARTESIAN_POINT('Ctrl Pts',(7.27603390512273,-45.7795179709987,-4.20082013377291));
#36506=CARTESIAN_POINT('Ctrl Pts',(4.85068927007173,-45.6045179709986,-8.40164026752836));
#36507=CARTESIAN_POINT('Ctrl Pts',(-1.51301075899711E-11,-45.4295179709987,
-8.40164026751963));
#36508=CARTESIAN_POINT('Ctrl Pts',(-4.85068927010199,-45.2545179709987,
-8.4016402675109));
#36509=CARTESIAN_POINT('Ctrl Pts',(-7.27603390513785,-45.0795179709987,
-4.20082013374671));
#36510=CARTESIAN_POINT('Ctrl Pts',(-9.70137854017372,-44.9045179709986,
1.74701493417668E-11));
#36511=CARTESIAN_POINT('Ctrl Pts',(-7.27603390512272,-44.7295179709987,
4.20082013377292));
#36512=CARTESIAN_POINT('Ctrl Pts',(-4.85068927007173,-44.5545179709987,
8.40164026752836));
#36513=CARTESIAN_POINT('Ctrl Pts',(1.5129078685785E-11,-44.3795179709986,
8.40164026751963));
#36514=CARTESIAN_POINT('Ctrl Pts',(4.85068927010198,-44.2045179709987,8.4016402675109));
#36515=CARTESIAN_POINT('Ctrl Pts',(7.27603390513785,-44.0295179709987,4.20082013374672));
#36516=CARTESIAN_POINT('Ctrl Pts',(9.70137854017372,-43.8545179709986,-1.74689612655491E-11));
#36517=CARTESIAN_POINT('Ctrl Pts',(7.27603390512273,-43.6795179709987,-4.20082013377291));
#36518=CARTESIAN_POINT('Ctrl Pts',(4.85068927007173,-43.5045179709987,-8.40164026752836));
#36519=CARTESIAN_POINT('Ctrl Pts',(-1.51301075899711E-11,-43.3295179709987,
-8.40164026751963));
#36520=CARTESIAN_POINT('',(-5.67113674141202,-212.63,6.19885209091279));
#36521=CARTESIAN_POINT('Ctrl Pts',(-5.67113674141202,-212.63,6.19885209091279));
#36522=CARTESIAN_POINT('Ctrl Pts',(-3.26337288082243,-212.49725180682,8.40164026752551));
#36523=CARTESIAN_POINT('Ctrl Pts',(1.5129078685785E-11,-212.379517970998,
8.40164026751963));
#36524=CARTESIAN_POINT('Ctrl Pts',(4.85068927010198,-212.204517970998,8.4016402675109));
#36525=CARTESIAN_POINT('Ctrl Pts',(7.27603390513785,-212.029517970998,4.20082013374672));
#36526=CARTESIAN_POINT('Ctrl Pts',(9.70137854017372,-211.854517970998,-1.74689612655491E-11));
#36527=CARTESIAN_POINT('Ctrl Pts',(7.27603390512273,-211.679517970998,-4.20082013377291));
#36528=CARTESIAN_POINT('Ctrl Pts',(4.85068927007173,-211.504517970998,-8.40164026752836));
#36529=CARTESIAN_POINT('Ctrl Pts',(-1.51280497815988E-11,-211.329517970998,
-8.40164026751963));
#36530=CARTESIAN_POINT('Ctrl Pts',(-4.85068927010198,-211.154517970998,
-8.4016402675109));
#36531=CARTESIAN_POINT('Ctrl Pts',(-7.27603390513785,-210.979517970998,
-4.20082013374672));
#36532=CARTESIAN_POINT('Ctrl Pts',(-9.70137854017372,-210.804517970998,
1.74591566342707E-11));
#36533=CARTESIAN_POINT('Ctrl Pts',(-7.27603390512273,-210.629517970998,
4.20082013377291));
#36534=CARTESIAN_POINT('Ctrl Pts',(-4.85068927007174,-210.454517970998,
8.40164026752836));
#36535=CARTESIAN_POINT('Ctrl Pts',(1.51270208774127E-11,-210.279517970998,
8.40164026751963));
#36536=CARTESIAN_POINT('Ctrl Pts',(4.85068927010198,-210.104517970998,8.4016402675109));
#36537=CARTESIAN_POINT('Ctrl Pts',(7.27603390513785,-209.929517970998,4.20082013374672));
#36538=CARTESIAN_POINT('Ctrl Pts',(9.70137854017372,-209.754517970998,-1.74665851131138E-11));
#36539=CARTESIAN_POINT('Ctrl Pts',(7.27603390512273,-209.579517970998,-4.20082013377291));
#36540=CARTESIAN_POINT('Ctrl Pts',(4.85068927007174,-209.404517970998,-8.40164026752836));
#36541=CARTESIAN_POINT('Ctrl Pts',(-1.51259919732266E-11,-209.229517970998,
-8.40164026751963));
#36542=CARTESIAN_POINT('Ctrl Pts',(-4.85068927010198,-209.054517970998,
-8.4016402675109));
#36543=CARTESIAN_POINT('Ctrl Pts',(-7.27603390513785,-208.879517970998,
-4.20082013374672));
#36544=CARTESIAN_POINT('Ctrl Pts',(-9.70137854017372,-208.704517970998,
1.74481639267747E-11));
#36545=CARTESIAN_POINT('Ctrl Pts',(-7.27603390512273,-208.529517970998,
4.20082013377291));
#36546=CARTESIAN_POINT('Ctrl Pts',(-4.85068927007174,-208.354517970998,
8.40164026752836));
#36547=CARTESIAN_POINT('Ctrl Pts',(1.51100387578891E-11,-208.179517970998,
8.40164026751963));
#36548=CARTESIAN_POINT('Ctrl Pts',(4.85068927010198,-208.004517970998,8.4016402675109));
#36549=CARTESIAN_POINT('Ctrl Pts',(7.27603390513784,-207.829517970998,4.20082013374673));
#36550=CARTESIAN_POINT('Ctrl Pts',(9.70137854017372,-207.654517970998,-1.74469758505571E-11));
#36551=CARTESIAN_POINT('Ctrl Pts',(7.27603390512273,-207.479517970998,-4.2008201337729));
#36552=CARTESIAN_POINT('Ctrl Pts',(4.85068927007176,-207.304517970998,-8.40164026752835));
#36553=CARTESIAN_POINT('Ctrl Pts',(-1.51239341648544E-11,-207.129517970998,
-8.40164026751963));
#36554=CARTESIAN_POINT('Ctrl Pts',(-4.85068927010198,-206.954517970998,
-8.4016402675109));
#36555=CARTESIAN_POINT('Ctrl Pts',(-7.27603390513784,-206.779517970998,
-4.20082013374673));
#36556=CARTESIAN_POINT('Ctrl Pts',(-9.70137854017372,-206.604517970998,
1.74457877743394E-11));
#36557=CARTESIAN_POINT('Ctrl Pts',(-7.27603390512273,-206.429517970998,
4.20082013377289));
#36558=CARTESIAN_POINT('Ctrl Pts',(-4.85068927007176,-206.254517970998,
8.40164026752835));
#36559=CARTESIAN_POINT('Ctrl Pts',(1.51229052606682E-11,-206.079517970998,
8.40164026751963));
#36560=CARTESIAN_POINT('Ctrl Pts',(4.85068927010198,-205.904517970998,8.4016402675109));
#36561=CARTESIAN_POINT('Ctrl Pts',(7.27603390513784,-205.729517970998,4.20082013374673));
#36562=CARTESIAN_POINT('Ctrl Pts',(9.70137854017372,-205.554517970998,-1.74445996981217E-11));
#36563=CARTESIAN_POINT('Ctrl Pts',(7.27603390512273,-205.379517970998,-4.20082013377289));
#36564=CARTESIAN_POINT('Ctrl Pts',(4.85068927007176,-205.204517970998,-8.40164026752835));
#36565=CARTESIAN_POINT('Ctrl Pts',(-1.51218763564821E-11,-205.029517970998,
-8.40164026751963));
#36566=CARTESIAN_POINT('Ctrl Pts',(-4.85068927010197,-204.854517970998,
-8.4016402675109));
#36567=CARTESIAN_POINT('Ctrl Pts',(-7.27603390513784,-204.679517970998,
-4.20082013374673));
#36568=CARTESIAN_POINT('Ctrl Pts',(-9.70137854017372,-204.504517970998,
1.74434116219041E-11));
#36569=CARTESIAN_POINT('Ctrl Pts',(-7.27603390512274,-204.329517970998,
4.20082013377289));
#36570=CARTESIAN_POINT('Ctrl Pts',(-4.85068927007176,-204.154517970998,
8.40164026752834));
#36571=CARTESIAN_POINT('Ctrl Pts',(1.50909988299932E-11,-203.979517970998,
8.40164026751963));
#36572=CARTESIAN_POINT('Ctrl Pts',(4.85068927010197,-203.804517970998,8.4016402675109));
#36573=CARTESIAN_POINT('Ctrl Pts',(7.27603390513784,-203.629517970998,4.20082013374673));
#36574=CARTESIAN_POINT('Ctrl Pts',(9.70137854017372,-203.454517970998,-1.74422235456864E-11));
#36575=CARTESIAN_POINT('Ctrl Pts',(7.27603390512274,-203.279517970998,-4.20082013377289));
#36576=CARTESIAN_POINT('Ctrl Pts',(4.85068927007176,-203.104517970998,-8.40164026752834));
#36577=CARTESIAN_POINT('Ctrl Pts',(-1.50899699258071E-11,-202.929517970998,
-8.40164026751963));
#36578=CARTESIAN_POINT('Ctrl Pts',(-4.85068927010197,-202.754517970998,
-8.4016402675109));
#36579=CARTESIAN_POINT('Ctrl Pts',(-7.27603390513784,-202.579517970998,
-4.20082013374673));
#36580=CARTESIAN_POINT('Ctrl Pts',(-9.70137854017372,-202.404517970998,
1.74065692492259E-11));
#36581=CARTESIAN_POINT('Ctrl Pts',(-7.27603390512274,-202.229517970998,
4.20082013377289));
#36582=CARTESIAN_POINT('Ctrl Pts',(-4.85068927007173,-202.054517970998,
8.40164026752836));
#36583=CARTESIAN_POINT('Ctrl Pts',(1.5088941021621E-11,-201.879517970998,
8.40164026751963));
#36584=CARTESIAN_POINT('Ctrl Pts',(4.85068927010197,-201.704517970998,8.4016402675109));
#36585=CARTESIAN_POINT('Ctrl Pts',(7.27603390513783,-201.529517970998,4.20082013374676));
#36586=CARTESIAN_POINT('Ctrl Pts',(9.70137854017372,-201.354517970998,-1.74398473932511E-11));
#36587=CARTESIAN_POINT('Ctrl Pts',(7.27603390512275,-201.179517970998,-4.20082013377287));
#36588=CARTESIAN_POINT('Ctrl Pts',(4.85068927007176,-201.004517970998,-8.40164026752834));
#36589=CARTESIAN_POINT('Ctrl Pts',(-1.51177607397376E-11,-200.829517970998,
-8.40164026751963));
#36590=CARTESIAN_POINT('Ctrl Pts',(-4.85068927010194,-200.654517970998,
-8.40164026751092));
#36591=CARTESIAN_POINT('Ctrl Pts',(-7.27603390513784,-200.479517970998,
-4.20082013374673));
#36592=CARTESIAN_POINT('Ctrl Pts',(-9.70137854017372,-200.304517970998,
1.74041930967906E-11));
#36593=CARTESIAN_POINT('Ctrl Pts',(-7.27603390512274,-200.129517970998,
4.20082013377289));
#36594=CARTESIAN_POINT('Ctrl Pts',(-4.85068927007174,-199.954517970998,
8.40164026752836));
#36595=CARTESIAN_POINT('Ctrl Pts',(1.50868832132487E-11,-199.779517970998,
8.40164026751963));
#36596=CARTESIAN_POINT('Ctrl Pts',(4.85068927010197,-199.604517970998,8.4016402675109));
#36597=CARTESIAN_POINT('Ctrl Pts',(7.27603390513783,-199.429517970998,4.20082013374676));
#36598=CARTESIAN_POINT('Ctrl Pts',(9.70137854017372,-199.254517970998,-1.74374712408158E-11));
#36599=CARTESIAN_POINT('Ctrl Pts',(7.27603390512275,-199.079517970998,-4.20082013377286));
#36600=CARTESIAN_POINT('Ctrl Pts',(4.85068927007177,-198.904517970998,-8.40164026752834));
#36601=CARTESIAN_POINT('Ctrl Pts',(-1.51157029313654E-11,-198.729517970998,
-8.40164026751963));
#36602=CARTESIAN_POINT('Ctrl Pts',(-4.85068927010194,-198.554517970998,
-8.40164026751092));
#36603=CARTESIAN_POINT('Ctrl Pts',(-7.27603390513784,-198.379517970998,
-4.20082013374673));
#36604=CARTESIAN_POINT('Ctrl Pts',(-9.70137854017372,-198.204517970998,
1.74018169443553E-11));
#36605=CARTESIAN_POINT('Ctrl Pts',(-7.27603390512274,-198.029517970998,
4.20082013377289));
#36606=CARTESIAN_POINT('Ctrl Pts',(-4.8506892700718,-197.854517970998,8.40164026752832));
#36607=CARTESIAN_POINT('Ctrl Pts',(1.50848254048765E-11,-197.679517970998,
8.40164026751963));
#36608=CARTESIAN_POINT('Ctrl Pts',(4.85068927010197,-197.504517970998,8.4016402675109));
#36609=CARTESIAN_POINT('Ctrl Pts',(7.27603390513782,-197.329517970998,4.20082013374676));
#36610=CARTESIAN_POINT('Ctrl Pts',(9.70137854017372,-197.154517970998,-1.74350950883805E-11));
#36611=CARTESIAN_POINT('Ctrl Pts',(7.27603390512276,-196.979517970998,-4.20082013377286));
#36612=CARTESIAN_POINT('Ctrl Pts',(4.85068927007177,-196.804517970998,-8.40164026752834));
#36613=CARTESIAN_POINT('Ctrl Pts',(-1.51136451229931E-11,-196.629517970998,
-8.40164026751963));
#36614=CARTESIAN_POINT('Ctrl Pts',(-4.85068927010194,-196.454517970998,
-8.40164026751092));
#36615=CARTESIAN_POINT('Ctrl Pts',(-7.27603390513784,-196.279517970998,
-4.20082013374673));
#36616=CARTESIAN_POINT('Ctrl Pts',(-9.70137854017372,-196.104517970998,
1.739944079192E-11));
#36617=CARTESIAN_POINT('Ctrl Pts',(-7.27603390512274,-195.929517970998,
4.20082013377289));
#36618=CARTESIAN_POINT('Ctrl Pts',(-4.8506892700718,-195.754517970998,8.40164026752832));
#36619=CARTESIAN_POINT('Ctrl Pts',(1.50827675965043E-11,-195.579517970998,
8.40164026751963));
#36620=CARTESIAN_POINT('Ctrl Pts',(4.85068927010196,-195.404517970998,8.40164026751091));
#36621=CARTESIAN_POINT('Ctrl Pts',(7.27603390513782,-195.229517970998,4.20082013374676));
#36622=CARTESIAN_POINT('Ctrl Pts',(9.70137854017372,-195.054517970998,-1.74327189359452E-11));
#36623=CARTESIAN_POINT('Ctrl Pts',(7.27603390512276,-194.879517970998,-4.20082013377286));
#36624=CARTESIAN_POINT('Ctrl Pts',(4.85068927007177,-194.704517970998,-8.40164026752834));
#36625=CARTESIAN_POINT('Ctrl Pts',(-1.50518900700154E-11,-194.529517970998,
-8.40164026751963));
#36626=CARTESIAN_POINT('Ctrl Pts',(-4.85068927010193,-194.354517970998,
-8.40164026751092));
#36627=CARTESIAN_POINT('Ctrl Pts',(-7.27603390513784,-194.179517970998,
-4.20082013374674));
#36628=CARTESIAN_POINT('Ctrl Pts',(-9.70137854017372,-194.004517970998,
1.73970646394847E-11));
#36629=CARTESIAN_POINT('Ctrl Pts',(-7.27603390512274,-193.829517970998,
4.20082013377288));
#36630=CARTESIAN_POINT('Ctrl Pts',(-4.8506892700718,-193.654517970998,8.40164026752832));
#36631=CARTESIAN_POINT('Ctrl Pts',(1.5080709788132E-11,-193.479517970998,
8.40164026751963));
#36632=CARTESIAN_POINT('Ctrl Pts',(4.8506892701019,-193.304517970998,8.40164026751094));
#36633=CARTESIAN_POINT('Ctrl Pts',(7.27603390513782,-193.129517970998,4.20082013374676));
#36634=CARTESIAN_POINT('Ctrl Pts',(9.70137854017372,-192.954517970998,-1.74303427835099E-11));
#36635=CARTESIAN_POINT('Ctrl Pts',(7.27603390512276,-192.779517970998,-4.20082013377286));
#36636=CARTESIAN_POINT('Ctrl Pts',(4.85068927007177,-192.604517970998,-8.40164026752834));
#36637=CARTESIAN_POINT('Ctrl Pts',(-1.50498322616431E-11,-192.429517970998,
-8.40164026751963));
#36638=CARTESIAN_POINT('Ctrl Pts',(-4.85068927010193,-192.254517970998,
-8.40164026751093));
#36639=CARTESIAN_POINT('Ctrl Pts',(-7.27603390513784,-192.079517970998,
-4.20082013374674));
#36640=CARTESIAN_POINT('Ctrl Pts',(-9.70137854017372,-191.904517970998,
1.73946884870493E-11));
#36641=CARTESIAN_POINT('Ctrl Pts',(-7.27603390512274,-191.729517970998,
4.20082013377288));
#36642=CARTESIAN_POINT('Ctrl Pts',(-4.85068927007174,-191.554517970998,
8.40164026752836));
#36643=CARTESIAN_POINT('Ctrl Pts',(1.50189547351542E-11,-191.379517970998,
8.40164026751963));
#36644=CARTESIAN_POINT('Ctrl Pts',(4.8506892701019,-191.204517970998,8.40164026751094));
#36645=CARTESIAN_POINT('Ctrl Pts',(7.27603390513782,-191.029517970998,4.20082013374676));
#36646=CARTESIAN_POINT('Ctrl Pts',(9.70137854017372,-190.854517970998,-1.74279666310746E-11));
#36647=CARTESIAN_POINT('Ctrl Pts',(7.27603390512273,-190.679517970998,-4.20082013377291));
#36648=CARTESIAN_POINT('Ctrl Pts',(4.85068927007184,-190.504517970998,-8.4016402675283));
#36649=CARTESIAN_POINT('Ctrl Pts',(-1.50477744532709E-11,-190.329517970998,
-8.40164026751963));
#36650=CARTESIAN_POINT('Ctrl Pts',(-4.85068927010193,-190.154517970998,
-8.40164026751093));
#36651=CARTESIAN_POINT('Ctrl Pts',(-7.27603390513784,-189.979517970998,
-4.20082013374674));
#36652=CARTESIAN_POINT('Ctrl Pts',(-9.70137854017372,-189.804517970998,
1.74612447750998E-11));
#36653=CARTESIAN_POINT('Ctrl Pts',(-7.27603390512277,-189.629517970998,
4.20082013377283));
#36654=CARTESIAN_POINT('Ctrl Pts',(-4.8506892700718,-189.454517970998,8.40164026752832));
#36655=CARTESIAN_POINT('Ctrl Pts',(1.50765941713875E-11,-189.279517970998,
8.40164026751963));
#36656=CARTESIAN_POINT('Ctrl Pts',(4.85068927010196,-189.104517970998,8.40164026751091));
#36657=CARTESIAN_POINT('Ctrl Pts',(7.27603390513779,-188.929517970998,4.20082013374682));
#36658=CARTESIAN_POINT('Ctrl Pts',(9.70137854017372,-188.754517970998,-1.73566580381535E-11));
#36659=CARTESIAN_POINT('Ctrl Pts',(7.27603390512276,-188.579517970998,-4.20082013377285));
#36660=CARTESIAN_POINT('Ctrl Pts',(4.85068927007178,-188.404517970998,-8.40164026752834));
#36661=CARTESIAN_POINT('Ctrl Pts',(-1.51054138895042E-11,-188.229517970998,
-8.40164026751963));
#36662=CARTESIAN_POINT('Ctrl Pts',(-4.85068927010187,-188.054517970998,
-8.40164026751096));
#36663=CARTESIAN_POINT('Ctrl Pts',(-7.27603390513781,-187.879517970998,
-4.20082013374679));
#36664=CARTESIAN_POINT('Ctrl Pts',(-9.70137854017372,-187.704517970998,
1.73899361821787E-11));
#36665=CARTESIAN_POINT('Ctrl Pts',(-7.27603390512274,-187.529517970998,
4.20082013377288));
#36666=CARTESIAN_POINT('Ctrl Pts',(-4.85068927007175,-187.354517970998,
8.40164026752835));
#36667=CARTESIAN_POINT('Ctrl Pts',(1.50148391184097E-11,-187.179517970998,
8.40164026751963));
#36668=CARTESIAN_POINT('Ctrl Pts',(4.8506892701019,-187.004517970998,8.40164026751095));
#36669=CARTESIAN_POINT('Ctrl Pts',(7.27603390513782,-186.829517970998,4.20082013374677));
#36670=CARTESIAN_POINT('Ctrl Pts',(9.70137854017372,-186.654517970998,-1.7423214326204E-11));
#36671=CARTESIAN_POINT('Ctrl Pts',(7.27603390512273,-186.479517970998,-4.2008201337729));
#36672=CARTESIAN_POINT('Ctrl Pts',(4.85068927007184,-186.304517970998,-8.4016402675283));
#36673=CARTESIAN_POINT('Ctrl Pts',(-1.50436588365264E-11,-186.129517970998,
-8.40164026751963));
#36674=CARTESIAN_POINT('Ctrl Pts',(-4.85068927010193,-185.954517970998,
-8.40164026751093));
#36675=CARTESIAN_POINT('Ctrl Pts',(-7.27603390513783,-185.779517970998,
-4.20082013374674));
#36676=CARTESIAN_POINT('Ctrl Pts',(-9.70137854017372,-185.604517970998,
1.73186275892576E-11));
#36677=CARTESIAN_POINT('Ctrl Pts',(-7.27603390512277,-185.429517970998,
4.20082013377283));
#36678=CARTESIAN_POINT('Ctrl Pts',(-4.85068927007181,-185.254517970998,
8.40164026752832));
#36679=CARTESIAN_POINT('Ctrl Pts',(1.5072478554643E-11,-185.079517970998,
8.40164026751963));
#36680=CARTESIAN_POINT('Ctrl Pts',(4.85068927010196,-184.904517970998,8.40164026751091));
#36681=CARTESIAN_POINT('Ctrl Pts',(7.27603390513779,-184.729517970998,4.20082013374682));
#36682=CARTESIAN_POINT('Ctrl Pts',(9.70137854017372,-184.554517970998,-1.73519057332829E-11));
#36683=CARTESIAN_POINT('Ctrl Pts',(7.27603390512276,-184.379517970998,-4.20082013377285));
#36684=CARTESIAN_POINT('Ctrl Pts',(4.85068927007178,-184.204517970998,-8.40164026752833));
#36685=CARTESIAN_POINT('Ctrl Pts',(-1.51012982727597E-11,-184.029517970998,
-8.40164026751963));
#36686=CARTESIAN_POINT('Ctrl Pts',(-4.85068927010186,-183.854517970998,
-8.40164026751097));
#36687=CARTESIAN_POINT('Ctrl Pts',(-7.2760339051378,-183.679517970998,-4.2008201337468));
#36688=CARTESIAN_POINT('Ctrl Pts',(-9.70137854017372,-183.504517970998,
1.73851838773081E-11));
#36689=CARTESIAN_POINT('Ctrl Pts',(-7.27603390512275,-183.329517970998,
4.20082013377288));
#36690=CARTESIAN_POINT('Ctrl Pts',(-4.85068927007175,-183.154517970998,
8.40164026752835));
#36691=CARTESIAN_POINT('Ctrl Pts',(1.50107235016652E-11,-182.979517970998,
8.40164026751963));
#36692=CARTESIAN_POINT('Ctrl Pts',(4.85068927010189,-182.804517970998,8.40164026751095));
#36693=CARTESIAN_POINT('Ctrl Pts',(7.27603390513782,-182.629517970998,4.20082013374677));
#36694=CARTESIAN_POINT('Ctrl Pts',(9.70137854017372,-182.454517970998,-1.74184620213334E-11));
#36695=CARTESIAN_POINT('Ctrl Pts',(7.27603390512279,-182.279517970998,-4.2008201337728));
#36696=CARTESIAN_POINT('Ctrl Pts',(4.85068927007184,-182.104517970998,-8.4016402675283));
#36697=CARTESIAN_POINT('Ctrl Pts',(-1.50395432197819E-11,-181.929517970998,
-8.40164026751963));
#36698=CARTESIAN_POINT('Ctrl Pts',(-4.85068927010192,-181.754517970998,
-8.40164026751093));
#36699=CARTESIAN_POINT('Ctrl Pts',(-7.27603390513783,-181.579517970998,
-4.20082013374675));
#36700=CARTESIAN_POINT('Ctrl Pts',(-9.70137854017372,-181.404517970998,
1.7313875284387E-11));
#36701=CARTESIAN_POINT('Ctrl Pts',(-7.27603390512278,-181.229517970998,
4.20082013377282));
#36702=CARTESIAN_POINT('Ctrl Pts',(-4.85068927007181,-181.054517970998,
8.40164026752832));
#36703=CARTESIAN_POINT('Ctrl Pts',(1.50683629378986E-11,-180.879517970998,
8.40164026751963));
#36704=CARTESIAN_POINT('Ctrl Pts',(4.85068927010195,-180.704517970998,8.40164026751092));
#36705=CARTESIAN_POINT('Ctrl Pts',(7.27603390513779,-180.529517970998,4.20082013374683));
#36706=CARTESIAN_POINT('Ctrl Pts',(9.70137854017372,-180.354517970998,-1.73471534284123E-11));
#36707=CARTESIAN_POINT('Ctrl Pts',(7.27603390512276,-180.179517970998,-4.20082013377285));
#36708=CARTESIAN_POINT('Ctrl Pts',(4.85068927007178,-180.004517970998,-8.40164026752833));
#36709=CARTESIAN_POINT('Ctrl Pts',(-1.50971826560152E-11,-179.829517970998,
-8.40164026751963));
#36710=CARTESIAN_POINT('Ctrl Pts',(-4.85068927010186,-179.654517970998,
-8.40164026751097));
#36711=CARTESIAN_POINT('Ctrl Pts',(-7.2760339051378,-179.479517970998,-4.2008201337468));
#36712=CARTESIAN_POINT('Ctrl Pts',(-9.70137854017372,-179.304517970998,
1.73804315724375E-11));
#36713=CARTESIAN_POINT('Ctrl Pts',(-7.27603390512275,-179.129517970998,
4.20082013377287));
#36714=CARTESIAN_POINT('Ctrl Pts',(-4.85068927007188,-178.954517970998,
8.40164026752828));
#36715=CARTESIAN_POINT('Ctrl Pts',(1.50066078849208E-11,-178.779517970998,
8.40164026751963));
#36716=CARTESIAN_POINT('Ctrl Pts',(4.85068927010189,-178.604517970998,8.40164026751095));
#36717=CARTESIAN_POINT('Ctrl Pts',(7.27603390513782,-178.429517970998,4.20082013374678));
#36718=CARTESIAN_POINT('Ctrl Pts',(9.70137854017372,-178.254517970998,-1.74137097164627E-11));
#36719=CARTESIAN_POINT('Ctrl Pts',(7.27603390512279,-178.079517970998,-4.20082013377279));
#36720=CARTESIAN_POINT('Ctrl Pts',(4.85068927007185,-177.904517970998,-8.4016402675283));
#36721=CARTESIAN_POINT('Ctrl Pts',(-1.50354276030374E-11,-177.729517970998,
-8.40164026751963));
#36722=CARTESIAN_POINT('Ctrl Pts',(-4.85068927010192,-177.554517970998,
-8.40164026751093));
#36723=CARTESIAN_POINT('Ctrl Pts',(-7.27603390513783,-177.379517970998,
-4.20082013374675));
#36724=CARTESIAN_POINT('Ctrl Pts',(-9.70137854017372,-177.204517970998,
1.73091229795164E-11));
#36725=CARTESIAN_POINT('Ctrl Pts',(-7.27603390512278,-177.029517970998,
4.20082013377282));
#36726=CARTESIAN_POINT('Ctrl Pts',(-4.85068927007182,-176.854517970998,
8.40164026752831));
#36727=CARTESIAN_POINT('Ctrl Pts',(1.50642473211541E-11,-176.679517970998,
8.40164026751963));
#36728=CARTESIAN_POINT('Ctrl Pts',(4.85068927010183,-176.504517970998,8.40164026751099));
#36729=CARTESIAN_POINT('Ctrl Pts',(7.27603390513778,-176.329517970998,4.20082013374683));
#36730=CARTESIAN_POINT('Ctrl Pts',(9.70137854017372,-176.154517970998,-1.73424011235416E-11));
#36731=CARTESIAN_POINT('Ctrl Pts',(7.27603390512277,-175.979517970998,-4.20082013377284));
#36732=CARTESIAN_POINT('Ctrl Pts',(4.85068927007179,-175.804517970998,-8.40164026752833));
#36733=CARTESIAN_POINT('Ctrl Pts',(-1.49736725500596E-11,-175.629517970998,
-8.40164026751963));
#36734=CARTESIAN_POINT('Ctrl Pts',(-4.85068927010185,-175.454517970998,
-8.40164026751097));
#36735=CARTESIAN_POINT('Ctrl Pts',(-7.2760339051378,-175.279517970998,-4.2008201337468));
#36736=CARTESIAN_POINT('Ctrl Pts',(-9.70137854017372,-175.104517970998,
1.73756792675669E-11));
#36737=CARTESIAN_POINT('Ctrl Pts',(-7.27603390512275,-174.929517970998,
4.20082013377287));
#36738=CARTESIAN_POINT('Ctrl Pts',(-4.85068927007188,-174.754517970998,
8.40164026752828));
#36739=CARTESIAN_POINT('Ctrl Pts',(1.50024922681763E-11,-174.579517970998,
8.40164026751963));
#36740=CARTESIAN_POINT('Ctrl Pts',(4.85068927010188,-174.404517970998,8.40164026751095));
#36741=CARTESIAN_POINT('Ctrl Pts',(7.27603390513781,-174.229517970998,4.20082013374678));
#36742=CARTESIAN_POINT('Ctrl Pts',(9.70137854017372,-174.054517970998,-1.74089574115921E-11));
#36743=CARTESIAN_POINT('Ctrl Pts',(7.2760339051228,-173.879517970998,-4.20082013377279));
#36744=CARTESIAN_POINT('Ctrl Pts',(4.85068927007185,-173.704517970998,-8.4016402675283));
#36745=CARTESIAN_POINT('Ctrl Pts',(-1.50313119862929E-11,-173.529517970998,
-8.40164026751963));
#36746=CARTESIAN_POINT('Ctrl Pts',(-4.85068927010191,-173.354517970998,
-8.40164026751094));
#36747=CARTESIAN_POINT('Ctrl Pts',(-7.27603390513777,-173.179517970998,
-4.20082013374686));
#36748=CARTESIAN_POINT('Ctrl Pts',(-9.70137854017372,-173.004517970998,
1.73043706746458E-11));
#36749=CARTESIAN_POINT('Ctrl Pts',(-7.27603390512278,-172.829517970998,
4.20082013377282));
#36750=CARTESIAN_POINT('Ctrl Pts',(-4.85068927007182,-172.654517970998,
8.40164026752831));
#36751=CARTESIAN_POINT('Ctrl Pts',(1.50601317044096E-11,-172.479517970998,
8.40164026751963));
#36752=CARTESIAN_POINT('Ctrl Pts',(4.85068927010182,-172.304517970998,8.40164026751099));
#36753=CARTESIAN_POINT('Ctrl Pts',(7.27603390513778,-172.129517970998,4.20082013374683));
#36754=CARTESIAN_POINT('Ctrl Pts',(9.70137854017372,-171.954517970998,-1.7337648818671E-11));
#36755=CARTESIAN_POINT('Ctrl Pts',(7.27603390512277,-171.779517970998,-4.20082013377284));
#36756=CARTESIAN_POINT('Ctrl Pts',(4.85068927007179,-171.604517970998,-8.40164026752833));
#36757=CARTESIAN_POINT('Ctrl Pts',(-1.49695569333151E-11,-171.429517970998,
-8.40164026751963));
#36758=CARTESIAN_POINT('Ctrl Pts',(-4.85068927010185,-171.254517970998,
-8.40164026751097));
#36759=CARTESIAN_POINT('Ctrl Pts',(-7.2760339051378,-171.079517970998,-4.20082013374681));
#36760=CARTESIAN_POINT('Ctrl Pts',(-9.70137854017372,-170.904517970998,
1.73709269626963E-11));
#36761=CARTESIAN_POINT('Ctrl Pts',(-7.27603390512275,-170.729517970998,
4.20082013377287));
#36762=CARTESIAN_POINT('Ctrl Pts',(-4.85068927007176,-170.554517970998,
8.40164026752834));
#36763=CARTESIAN_POINT('Ctrl Pts',(1.49983766514318E-11,-170.379517970998,
8.40164026751963));
#36764=CARTESIAN_POINT('Ctrl Pts',(4.85068927010176,-170.204517970998,8.40164026751102));
#36765=CARTESIAN_POINT('Ctrl Pts',(7.27603390513781,-170.029517970998,4.20082013374678));
#36766=CARTESIAN_POINT('Ctrl Pts',(9.70137854017372,-169.854517970998,-1.72663402257499E-11));
#36767=CARTESIAN_POINT('Ctrl Pts',(7.27603390512274,-169.679517970998,-4.20082013377289));
#36768=CARTESIAN_POINT('Ctrl Pts',(4.85068927007186,-169.504517970998,-8.40164026752829));
#36769=CARTESIAN_POINT('Ctrl Pts',(-1.49078018803373E-11,-169.329517970998,
-8.40164026751963));
#36770=CARTESIAN_POINT('Ctrl Pts',(-4.85068927010191,-169.154517970998,
-8.40164026751094));
#36771=CARTESIAN_POINT('Ctrl Pts',(-7.27603390513777,-168.979517970998,
-4.20082013374686));
#36772=CARTESIAN_POINT('Ctrl Pts',(-9.70137854017372,-168.804517970998,
1.74374832507468E-11));
#36773=CARTESIAN_POINT('Ctrl Pts',(-7.27603390512278,-168.629517970998,
4.20082013377281));
#36774=CARTESIAN_POINT('Ctrl Pts',(-4.85068927007195,-168.454517970998,
8.40164026752824));
#36775=CARTESIAN_POINT('Ctrl Pts',(1.50560160876651E-11,-168.279517970998,
8.40164026751963));
#36776=CARTESIAN_POINT('Ctrl Pts',(4.85068927010182,-168.104517970998,8.40164026751099));
#36777=CARTESIAN_POINT('Ctrl Pts',(7.27603390513784,-167.929517970998,4.20082013374673));
#36778=CARTESIAN_POINT('Ctrl Pts',(9.70137854017372,-167.754517970998,-1.73328965138004E-11));
#36779=CARTESIAN_POINT('Ctrl Pts',(7.27603390512283,-167.579517970998,-4.20082013377273));
#36780=CARTESIAN_POINT('Ctrl Pts',(4.8506892700718,-167.404517970998,-8.40164026752832));
#36781=CARTESIAN_POINT('Ctrl Pts',(-1.49654413165707E-11,-167.229517970998,
-8.40164026751963));
#36782=CARTESIAN_POINT('Ctrl Pts',(-4.85068927010197,-167.054517970998,
-8.4016402675109));
#36783=CARTESIAN_POINT('Ctrl Pts',(-7.27603390513779,-166.879517970998,
-4.20082013374681));
#36784=CARTESIAN_POINT('Ctrl Pts',(-9.70137854017372,-166.704517970998,
1.72283097768541E-11));
#36785=CARTESIAN_POINT('Ctrl Pts',(-7.27603390512276,-166.529517970998,
4.20082013377286));
#36786=CARTESIAN_POINT('Ctrl Pts',(-4.85068927007189,-166.354517970998,
8.40164026752827));
#36787=CARTESIAN_POINT('Ctrl Pts',(1.51136555238984E-11,-166.179517970998,
8.40164026751963));
#36788=CARTESIAN_POINT('Ctrl Pts',(4.85068927010188,-166.004517970998,8.40164026751096));
#36789=CARTESIAN_POINT('Ctrl Pts',(7.27603390513775,-165.829517970998,4.20082013374689));
#36790=CARTESIAN_POINT('Ctrl Pts',(9.70137854017372,-165.654517970998,-1.73994528018509E-11));
#36791=CARTESIAN_POINT('Ctrl Pts',(7.2760339051228,-165.479517970998,-4.20082013377278));
#36792=CARTESIAN_POINT('Ctrl Pts',(4.85068927007198,-165.304517970998,-8.40164026752822));
#36793=CARTESIAN_POINT('Ctrl Pts',(-1.5023080752804E-11,-165.129517970998,
-8.40164026751963));
#36794=CARTESIAN_POINT('Ctrl Pts',(-4.85068927010179,-164.954517970998,
-8.40164026751101));
#36795=CARTESIAN_POINT('Ctrl Pts',(-7.27603390513782,-164.779517970998,
-4.20082013374676));
#36796=CARTESIAN_POINT('Ctrl Pts',(-9.70137854017372,-164.604517970998,
1.72948660649045E-11));
#36797=CARTESIAN_POINT('Ctrl Pts',(-7.27603390512285,-164.429517970998,
4.20082013377271));
#36798=CARTESIAN_POINT('Ctrl Pts',(-4.85068927007183,-164.254517970998,
8.40164026752831));
#36799=CARTESIAN_POINT('Ctrl Pts',(1.49325059817095E-11,-164.079517970998,
8.40164026751963));
#36800=CARTESIAN_POINT('Ctrl Pts',(4.85068927010193,-163.904517970998,8.40164026751092));
#36801=CARTESIAN_POINT('Ctrl Pts',(7.27603390513778,-163.729517970998,4.20082013374684));
#36802=CARTESIAN_POINT('Ctrl Pts',(9.70137854017372,-163.554517970998,-1.71902793279582E-11));
#36803=CARTESIAN_POINT('Ctrl Pts',(7.27603390512277,-163.379517970998,-4.20082013377283));
#36804=CARTESIAN_POINT('Ctrl Pts',(4.85068927007192,-163.204517970998,-8.40164026752825));
#36805=CARTESIAN_POINT('Ctrl Pts',(-1.50807201890373E-11,-163.029517970998,
-8.40164026751963));
#36806=CARTESIAN_POINT('Ctrl Pts',(-4.85068927010184,-162.854517970998,
-8.40164026751098));
#36807=CARTESIAN_POINT('Ctrl Pts',(-7.27603390513773,-162.679517970998,
-4.20082013374692));
#36808=CARTESIAN_POINT('Ctrl Pts',(-9.70137854017372,-162.504517970998,
1.7361422352955E-11));
#36809=CARTESIAN_POINT('Ctrl Pts',(-7.27603390512282,-162.329517970998,
4.20082013377275));
#36810=CARTESIAN_POINT('Ctrl Pts',(-4.85068927007177,-162.154517970998,
8.40164026752834));
#36811=CARTESIAN_POINT('Ctrl Pts',(1.49901454179428E-11,-161.979517970998,
8.40164026751963));
#36812=CARTESIAN_POINT('Ctrl Pts',(4.85068927010175,-161.804517970998,8.40164026751103));
#36813=CARTESIAN_POINT('Ctrl Pts',(7.27603390513781,-161.629517970998,4.20082013374679));
#36814=CARTESIAN_POINT('Ctrl Pts',(9.70137854017372,-161.454517970998,-1.72568356160087E-11));
#36815=CARTESIAN_POINT('Ctrl Pts',(7.27603390512274,-161.279517970998,-4.20082013377288));
#36816=CARTESIAN_POINT('Ctrl Pts',(4.85068927007186,-161.104517970998,-8.40164026752829));
#36817=CARTESIAN_POINT('Ctrl Pts',(-1.48995706468484E-11,-160.929517970998,
-8.40164026751963));
#36818=CARTESIAN_POINT('Ctrl Pts',(-4.8506892701019,-160.754517970998,-8.40164026751094));
#36819=CARTESIAN_POINT('Ctrl Pts',(-7.27603390513776,-160.579517970998,
-4.20082013374687));
#36820=CARTESIAN_POINT('Ctrl Pts',(-9.70137854017372,-160.404517970998,
1.74279786410055E-11));
#36821=CARTESIAN_POINT('Ctrl Pts',(-7.27603390512279,-160.229517970998,
4.2008201337728));
#36822=CARTESIAN_POINT('Ctrl Pts',(-4.85068927007195,-160.054517970998,
8.40164026752823));
#36823=CARTESIAN_POINT('Ctrl Pts',(1.50477848541761E-11,-159.879517970998,
8.40164026751963));
#36824=CARTESIAN_POINT('Ctrl Pts',(4.85068927010181,-159.704517970998,8.401640267511));
#36825=CARTESIAN_POINT('Ctrl Pts',(7.27603390513784,-159.529517970998,4.20082013374674));
#36826=CARTESIAN_POINT('Ctrl Pts',(9.70137854017372,-159.354517970998,-1.73233919040592E-11));
#36827=CARTESIAN_POINT('Ctrl Pts',(7.27603390512283,-159.179517970998,-4.20082013377273));
#36828=CARTESIAN_POINT('Ctrl Pts',(4.8506892700718,-159.004517970998,-8.40164026752832));
#36829=CARTESIAN_POINT('Ctrl Pts',(-1.49572100830817E-11,-158.829517970998,
-8.40164026751963));
#36830=CARTESIAN_POINT('Ctrl Pts',(-4.85068927010172,-158.654517970998,
-8.40164026751105));
#36831=CARTESIAN_POINT('Ctrl Pts',(-7.27603390513779,-158.479517970998,
-4.20082013374682));
#36832=CARTESIAN_POINT('Ctrl Pts',(-9.70137854017372,-158.304517970998,
1.72188051671128E-11));
#36833=CARTESIAN_POINT('Ctrl Pts',(-7.27603390512276,-158.129517970998,
4.20082013377285));
#36834=CARTESIAN_POINT('Ctrl Pts',(-4.8506892700719,-157.954517970998,8.40164026752827));
#36835=CARTESIAN_POINT('Ctrl Pts',(1.48666353119872E-11,-157.779517970998,
8.40164026751963));
#36836=CARTESIAN_POINT('Ctrl Pts',(4.85068927010187,-157.604517970998,8.40164026751096));
#36837=CARTESIAN_POINT('Ctrl Pts',(7.27603390513774,-157.429517970998,4.2008201337469));
#36838=CARTESIAN_POINT('Ctrl Pts',(9.70137854017372,-157.254517970998,-1.73899481921097E-11));
#36839=CARTESIAN_POINT('Ctrl Pts',(7.27603390512281,-157.079517970998,-4.20082013377278));
#36840=CARTESIAN_POINT('Ctrl Pts',(4.85068927007199,-156.904517970998,-8.40164026752822));
#36841=CARTESIAN_POINT('Ctrl Pts',(-1.5014849519315E-11,-156.729517970998,
-8.40164026751963));
#36842=CARTESIAN_POINT('Ctrl Pts',(-4.85068927010178,-156.554517970998,
-8.40164026751101));
#36843=CARTESIAN_POINT('Ctrl Pts',(-7.27603390513782,-156.379517970998,
-4.20082013374677));
#36844=CARTESIAN_POINT('Ctrl Pts',(-9.70137854017372,-156.204517970998,
1.72853614551633E-11));
#36845=CARTESIAN_POINT('Ctrl Pts',(-7.27603390512285,-156.029517970998,
4.2008201337727));
#36846=CARTESIAN_POINT('Ctrl Pts',(-4.85068927007184,-155.854517970998,
8.4016402675283));
#36847=CARTESIAN_POINT('Ctrl Pts',(1.49242747482206E-11,-155.679517970998,
8.40164026751963));
#36848=CARTESIAN_POINT('Ctrl Pts',(4.85068927010193,-155.504517970998,8.40164026751093));
#36849=CARTESIAN_POINT('Ctrl Pts',(7.27603390513778,-155.329517970998,4.20082013374685));
#36850=CARTESIAN_POINT('Ctrl Pts',(9.70137854017372,-155.154517970998,-1.7180774718217E-11));
#36851=CARTESIAN_POINT('Ctrl Pts',(7.27603390512277,-154.979517970998,-4.20082013377283));
#36852=CARTESIAN_POINT('Ctrl Pts',(4.85068927007193,-154.804517970998,-8.40164026752825));
#36853=CARTESIAN_POINT('Ctrl Pts',(-1.50724889555483E-11,-154.629517970998,
-8.40164026751963));
#36854=CARTESIAN_POINT('Ctrl Pts',(-4.85068927010184,-154.454517970998,
-8.40164026751098));
#36855=CARTESIAN_POINT('Ctrl Pts',(-7.27603390513773,-154.279517970998,
-4.20082013374692));
#36856=CARTESIAN_POINT('Ctrl Pts',(-9.70137854017372,-154.104517970998,
1.73519177432138E-11));
#36857=CARTESIAN_POINT('Ctrl Pts',(-7.27603390512282,-153.929517970998,
4.20082013377275));
#36858=CARTESIAN_POINT('Ctrl Pts',(-4.85068927007178,-153.754517970998,
8.40164026752833));
#36859=CARTESIAN_POINT('Ctrl Pts',(1.49819141844539E-11,-153.579517970998,
8.40164026751963));
#36860=CARTESIAN_POINT('Ctrl Pts',(4.85068927010175,-153.404517970998,8.40164026751103));
#36861=CARTESIAN_POINT('Ctrl Pts',(7.2760339051378,-153.229517970998,4.2008201337468));
#36862=CARTESIAN_POINT('Ctrl Pts',(9.70137854017372,-153.054517970998,-1.72473310062675E-11));
#36863=CARTESIAN_POINT('Ctrl Pts',(7.27603390512275,-152.879517970998,-4.20082013377288));
#36864=CARTESIAN_POINT('Ctrl Pts',(4.85068927007187,-152.704517970998,-8.40164026752828));
#36865=CARTESIAN_POINT('Ctrl Pts',(-1.48913394133594E-11,-152.529517970998,
-8.40164026751963));
#36866=CARTESIAN_POINT('Ctrl Pts',(-4.85068927010189,-152.354517970998,
-8.40164026751095));
#36867=CARTESIAN_POINT('Ctrl Pts',(-7.27603390513776,-152.179517970998,
-4.20082013374688));
#36868=CARTESIAN_POINT('Ctrl Pts',(-9.70137854017372,-152.004517970998,
1.71427442693211E-11));
#36869=CARTESIAN_POINT('Ctrl Pts',(-7.27603390512279,-151.829517970998,
4.2008201337728));
#36870=CARTESIAN_POINT('Ctrl Pts',(-4.85068927007196,-151.654517970998,
8.40164026752823));
#36871=CARTESIAN_POINT('Ctrl Pts',(1.50395536206872E-11,-151.479517970998,
8.40164026751963));
#36872=CARTESIAN_POINT('Ctrl Pts',(4.8506892701018,-151.304517970998,8.401640267511));
#36873=CARTESIAN_POINT('Ctrl Pts',(7.27603390513771,-151.129517970998,4.20082013374695));
#36874=CARTESIAN_POINT('Ctrl Pts',(9.70137854017372,-150.954517970998,-1.73138872943179E-11));
#36875=CARTESIAN_POINT('Ctrl Pts',(7.27603390512284,-150.779517970998,-4.20082013377272));
#36876=CARTESIAN_POINT('Ctrl Pts',(4.85068927007181,-150.604517970998,-8.40164026752832));
#36877=CARTESIAN_POINT('Ctrl Pts',(-1.49489788495927E-11,-150.429517970998,
-8.40164026751963));
#36878=CARTESIAN_POINT('Ctrl Pts',(-4.85068927010171,-150.254517970998,
-8.40164026751105));
#36879=CARTESIAN_POINT('Ctrl Pts',(-7.27603390513779,-150.079517970998,
-4.20082013374683));
#36880=CARTESIAN_POINT('Ctrl Pts',(-9.70137854017372,-149.904517970998,
1.72093005573716E-11));
#36881=CARTESIAN_POINT('Ctrl Pts',(-7.27603390512276,-149.729517970998,
4.20082013377285));
#36882=CARTESIAN_POINT('Ctrl Pts',(-4.8506892700719,-149.554517970998,8.40164026752826));
#36883=CARTESIAN_POINT('Ctrl Pts',(1.48584040784983E-11,-149.379517970998,
8.40164026751963));
#36884=CARTESIAN_POINT('Ctrl Pts',(4.85068927010186,-149.204517970998,8.40164026751097));
#36885=CARTESIAN_POINT('Ctrl Pts',(7.27603390513774,-149.029517970998,4.2008201337469));
#36886=CARTESIAN_POINT('Ctrl Pts',(9.70137854017372,-148.854517970998,-1.73804435823684E-11));
#36887=CARTESIAN_POINT('Ctrl Pts',(7.27603390512281,-148.679517970998,-4.20082013377277));
#36888=CARTESIAN_POINT('Ctrl Pts',(4.85068927007199,-148.504517970998,-8.40164026752821));
#36889=CARTESIAN_POINT('Ctrl Pts',(-1.5006618285826E-11,-148.329517970998,
-8.40164026751963));
#36890=CARTESIAN_POINT('Ctrl Pts',(-4.85068927010177,-148.154517970998,
-8.40164026751102));
#36891=CARTESIAN_POINT('Ctrl Pts',(-7.27603390513782,-147.979517970998,
-4.20082013374678));
#36892=CARTESIAN_POINT('Ctrl Pts',(-9.70137854017372,-147.804517970998,
1.72758568454221E-11));
#36893=CARTESIAN_POINT('Ctrl Pts',(-7.27603390512285,-147.629517970998,
4.20082013377269));
#36894=CARTESIAN_POINT('Ctrl Pts',(-4.85068927007185,-147.454517970998,
8.4016402675283));
#36895=CARTESIAN_POINT('Ctrl Pts',(1.49160435147316E-11,-147.279517970998,
8.40164026751963));
#36896=CARTESIAN_POINT('Ctrl Pts',(4.85068927010192,-147.104517970998,8.40164026751093));
#36897=CARTESIAN_POINT('Ctrl Pts',(7.27603390513777,-146.929517970998,4.20082013374685));
#36898=CARTESIAN_POINT('Ctrl Pts',(9.70137854017372,-146.754517970998,-1.71712701084757E-11));
#36899=CARTESIAN_POINT('Ctrl Pts',(7.27603390512278,-146.579517970998,-4.20082013377282));
#36900=CARTESIAN_POINT('Ctrl Pts',(4.85068927007194,-146.404517970998,-8.40164026752825));
#36901=CARTESIAN_POINT('Ctrl Pts',(-1.50642577220594E-11,-146.229517970998,
-8.40164026751963));
#36902=CARTESIAN_POINT('Ctrl Pts',(-4.85068927010183,-146.054517970998,
-8.40164026751099));
#36903=CARTESIAN_POINT('Ctrl Pts',(-7.27603390513773,-145.879517970998,
-4.20082013374693));
#36904=CARTESIAN_POINT('Ctrl Pts',(-9.70137854017372,-145.704517970998,
1.73424131334726E-11));
#36905=CARTESIAN_POINT('Ctrl Pts',(-7.27603390512282,-145.529517970998,
4.20082013377274));
#36906=CARTESIAN_POINT('Ctrl Pts',(-4.85068927007203,-145.354517970998,
8.40164026752819));
#36907=CARTESIAN_POINT('Ctrl Pts',(1.49736829509649E-11,-145.179517970998,
8.40164026751963));
#36908=CARTESIAN_POINT('Ctrl Pts',(4.85068927010174,-145.004517970998,8.40164026751104));
#36909=CARTESIAN_POINT('Ctrl Pts',(7.2760339051378,-144.829517970998,4.2008201337468));
#36910=CARTESIAN_POINT('Ctrl Pts',(9.70137854017372,-144.654517970998,-1.72378263965262E-11));
#36911=CARTESIAN_POINT('Ctrl Pts',(7.27603390512287,-144.479517970998,-4.20082013377266));
#36912=CARTESIAN_POINT('Ctrl Pts',(4.85068927007188,-144.304517970998,-8.40164026752828));
#36913=CARTESIAN_POINT('Ctrl Pts',(-1.48831081798705E-11,-144.129517970998,
-8.40164026751963));
#36914=CARTESIAN_POINT('Ctrl Pts',(-4.85068927010188,-143.954517970998,
-8.40164026751095));
#36915=CARTESIAN_POINT('Ctrl Pts',(-7.27603390513775,-143.779517970998,
-4.20082013374688));
#36916=CARTESIAN_POINT('Ctrl Pts',(-9.70137854017372,-143.604517970998,
1.71332396595799E-11));
#36917=CARTESIAN_POINT('Ctrl Pts',(-7.2760339051228,-143.429517970998,4.20082013377279));
#36918=CARTESIAN_POINT('Ctrl Pts',(-4.85068927007197,-143.254517970998,
8.40164026752823));
#36919=CARTESIAN_POINT('Ctrl Pts',(1.50313223871982E-11,-143.079517970998,
8.40164026751963));
#36920=CARTESIAN_POINT('Ctrl Pts',(4.85068927010179,-142.904517970998,8.401640267511));
#36921=CARTESIAN_POINT('Ctrl Pts',(7.27603390513771,-142.729517970998,4.20082013374696));
#36922=CARTESIAN_POINT('Ctrl Pts',(9.70137854017372,-142.554517970998,-1.73043826845767E-11));
#36923=CARTESIAN_POINT('Ctrl Pts',(7.27603390512284,-142.379517970998,-4.20082013377271));
#36924=CARTESIAN_POINT('Ctrl Pts',(4.85068927007182,-142.204517970998,-8.40164026752831));
#36925=CARTESIAN_POINT('Ctrl Pts',(-1.49407476161038E-11,-142.029517970998,
-8.40164026751963));
#36926=CARTESIAN_POINT('Ctrl Pts',(-4.8506892701017,-141.854517970998,-8.40164026751106));
#36927=CARTESIAN_POINT('Ctrl Pts',(-7.27603390513778,-141.679517970998,
-4.20082013374683));
#36928=CARTESIAN_POINT('Ctrl Pts',(-9.70137854017372,-141.504517970998,
1.71997959476304E-11));
#36929=CARTESIAN_POINT('Ctrl Pts',(-7.27603390512277,-141.329517970998,
4.20082013377284));
#36930=CARTESIAN_POINT('Ctrl Pts',(-4.85068927007191,-141.154517970998,
8.40164026752826));
#36931=CARTESIAN_POINT('Ctrl Pts',(1.48501728450093E-11,-140.979517970998,
8.40164026751963));
#36932=CARTESIAN_POINT('Ctrl Pts',(4.85068927010185,-140.804517970998,8.40164026751097));
#36933=CARTESIAN_POINT('Ctrl Pts',(7.27603390513774,-140.629517970998,4.20082013374691));
#36934=CARTESIAN_POINT('Ctrl Pts',(9.70137854017372,-140.454517970998,-1.73709389726272E-11));
#36935=CARTESIAN_POINT('Ctrl Pts',(7.27603390512281,-140.279517970998,-4.20082013377276));
#36936=CARTESIAN_POINT('Ctrl Pts',(4.850689270072,-140.104517970998,-8.40164026752821));
#36937=CARTESIAN_POINT('Ctrl Pts',(-1.49983870523371E-11,-139.929517970998,
-8.40164026751963));
#36938=CARTESIAN_POINT('Ctrl Pts',(-4.85068927010176,-139.754517970998,
-8.40164026751102));
#36939=CARTESIAN_POINT('Ctrl Pts',(-7.27603390513769,-139.579517970998,
-4.20082013374699));
#36940=CARTESIAN_POINT('Ctrl Pts',(-9.70137854017372,-139.404517970998,
1.72663522356809E-11));
#36941=CARTESIAN_POINT('Ctrl Pts',(-7.27603390512286,-139.229517970998,
4.20082013377268));
#36942=CARTESIAN_POINT('Ctrl Pts',(-4.85068927007186,-139.054517970998,
8.40164026752829));
#36943=CARTESIAN_POINT('Ctrl Pts',(1.49078122812426E-11,-138.879517970998,
8.40164026751963));
#36944=CARTESIAN_POINT('Ctrl Pts',(4.85068927010167,-138.704517970998,8.40164026751108));
#36945=CARTESIAN_POINT('Ctrl Pts',(7.27603390513777,-138.529517970998,4.20082013374686));
#36946=CARTESIAN_POINT('Ctrl Pts',(9.70137854017372,-138.354517970998,-1.71617654987345E-11));
#36947=CARTESIAN_POINT('Ctrl Pts',(7.27603390512278,-138.179517970998,-4.20082013377281));
#36948=CARTESIAN_POINT('Ctrl Pts',(4.85068927007195,-138.004517970998,-8.40164026752824));
#36949=CARTESIAN_POINT('Ctrl Pts',(-1.48172375101482E-11,-137.829517970998,
-8.40164026751963));
#36950=CARTESIAN_POINT('Ctrl Pts',(-4.85068927010182,-137.654517970998,
-8.40164026751099));
#36951=CARTESIAN_POINT('Ctrl Pts',(-7.27603390513772,-137.479517970998,
-4.20082013374694));
#36952=CARTESIAN_POINT('Ctrl Pts',(-9.70137854017372,-137.304517970998,
1.73329085237313E-11));
#36953=CARTESIAN_POINT('Ctrl Pts',(-7.27603390512283,-137.129517970998,
4.20082013377273));
#36954=CARTESIAN_POINT('Ctrl Pts',(-4.85068927007204,-136.954517970998,
8.40164026752819));
#36955=CARTESIAN_POINT('Ctrl Pts',(1.49654517174759E-11,-136.779517970998,
8.40164026751963));
#36956=CARTESIAN_POINT('Ctrl Pts',(4.85068927010173,-136.604517970998,8.40164026751104));
#36957=CARTESIAN_POINT('Ctrl Pts',(7.27603390513779,-136.429517970998,4.20082013374681));
#36958=CARTESIAN_POINT('Ctrl Pts',(9.70137854017372,-136.254517970999,-1.7228321786785E-11));
#36959=CARTESIAN_POINT('Ctrl Pts',(7.27603390512287,-136.079517970998,-4.20082013377265));
#36960=CARTESIAN_POINT('Ctrl Pts',(4.85068927007189,-135.904517970998,-8.40164026752827));
#36961=CARTESIAN_POINT('Ctrl Pts',(-1.48748769463815E-11,-135.729517970998,
-8.40164026751963));
#36962=CARTESIAN_POINT('Ctrl Pts',(-4.85068927010188,-135.554517970998,
-8.40164026751096));
#36963=CARTESIAN_POINT('Ctrl Pts',(-7.27603390513775,-135.379517970998,
-4.20082013374689));
#36964=CARTESIAN_POINT('Ctrl Pts',(-9.70137854017372,-135.204517970998,
1.71237350498386E-11));
#36965=CARTESIAN_POINT('Ctrl Pts',(-7.2760339051228,-135.029517970998,4.20082013377278));
#36966=CARTESIAN_POINT('Ctrl Pts',(-4.85068927007198,-134.854517970998,
8.40164026752822));
#36967=CARTESIAN_POINT('Ctrl Pts',(1.50230911537093E-11,-134.679517970998,
8.40164026751963));
#36968=CARTESIAN_POINT('Ctrl Pts',(4.85068927010179,-134.504517970998,8.40164026751101));
#36969=CARTESIAN_POINT('Ctrl Pts',(7.2760339051377,-134.329517970998,4.20082013374697));
#36970=CARTESIAN_POINT('Ctrl Pts',(9.70137854017372,-134.154517970998,-1.72948780748355E-11));
#36971=CARTESIAN_POINT('Ctrl Pts',(7.27603390512285,-133.979517970998,-4.20082013377271));
#36972=CARTESIAN_POINT('Ctrl Pts',(4.85068927007183,-133.804517970998,-8.40164026752831));
#36973=CARTESIAN_POINT('Ctrl Pts',(-1.49325163826148E-11,-133.629517970998,
-8.40164026751963));
#36974=CARTESIAN_POINT('Ctrl Pts',(-4.85068927010169,-133.454517970998,
-8.40164026751106));
#36975=CARTESIAN_POINT('Ctrl Pts',(-7.27603390513778,-133.279517970998,
-4.20082013374684));
#36976=CARTESIAN_POINT('Ctrl Pts',(-9.70137854017372,-133.104517970998,
1.71902913378891E-11));
#36977=CARTESIAN_POINT('Ctrl Pts',(-7.27603390512289,-132.929517970998,
4.20082013377263));
#36978=CARTESIAN_POINT('Ctrl Pts',(-4.85068927007192,-132.754517970998,
8.40164026752825));
#36979=CARTESIAN_POINT('Ctrl Pts',(1.48419416115203E-11,-132.579517970998,
8.40164026751963));
#36980=CARTESIAN_POINT('Ctrl Pts',(4.85068927010184,-132.404517970998,8.40164026751098));
#36981=CARTESIAN_POINT('Ctrl Pts',(7.27603390513773,-132.229517970998,4.20082013374692));
#36982=CARTESIAN_POINT('Ctrl Pts',(9.70137854017372,-132.054517970998,-1.70857046009428E-11));
#36983=CARTESIAN_POINT('Ctrl Pts',(7.27603390512282,-131.879517970998,-4.20082013377275));
#36984=CARTESIAN_POINT('Ctrl Pts',(4.85068927007201,-131.704517970998,-8.4016402675282));
#36985=CARTESIAN_POINT('Ctrl Pts',(-1.49901558188481E-11,-131.529517970998,
-8.40164026751963));
#36986=CARTESIAN_POINT('Ctrl Pts',(-4.85068927010175,-131.354517970998,
-8.40164026751103));
#36987=CARTESIAN_POINT('Ctrl Pts',(-7.27603390513769,-131.179517970998,
-4.200820133747));
#36988=CARTESIAN_POINT('Ctrl Pts',(-9.70137854017372,-131.004517970998,
1.72568476259396E-11));
#36989=CARTESIAN_POINT('Ctrl Pts',(-7.27603390512286,-130.829517970998,
4.20082013377267));
#36990=CARTESIAN_POINT('Ctrl Pts',(-4.85068927007186,-130.654517970998,
8.40164026752829));
#36991=CARTESIAN_POINT('Ctrl Pts',(1.48995810477537E-11,-130.479517970998,
8.40164026751963));
#36992=CARTESIAN_POINT('Ctrl Pts',(4.85068927010166,-130.304517970998,8.40164026751108));
#36993=CARTESIAN_POINT('Ctrl Pts',(7.27603390513776,-130.129517970998,4.20082013374687));
#36994=CARTESIAN_POINT('Ctrl Pts',(9.70137854017372,-129.954517970998,-1.71522608889933E-11));
#36995=CARTESIAN_POINT('Ctrl Pts',(7.27603390512279,-129.779517970998,-4.2008201337728));
#36996=CARTESIAN_POINT('Ctrl Pts',(4.85068927007195,-129.604517970998,-8.40164026752823));
#36997=CARTESIAN_POINT('Ctrl Pts',(-1.48090062766592E-11,-129.429517970998,
-8.40164026751963));
#36998=CARTESIAN_POINT('Ctrl Pts',(-4.85068927010181,-129.254517970998,
-8.401640267511));
#36999=CARTESIAN_POINT('Ctrl Pts',(-7.27603390513772,-129.079517970998,
-4.20082013374695));
#37000=CARTESIAN_POINT('Ctrl Pts',(-9.70137854017372,-128.904517970998,
1.73234039139901E-11));
#37001=CARTESIAN_POINT('Ctrl Pts',(-7.27603390512283,-128.729517970998,
4.20082013377273));
#37002=CARTESIAN_POINT('Ctrl Pts',(-4.85068927007204,-128.554517970998,
8.40164026752818));
#37003=CARTESIAN_POINT('Ctrl Pts',(1.4957220483987E-11,-128.379517970998,
8.40164026751963));
#37004=CARTESIAN_POINT('Ctrl Pts',(4.85068927010172,-128.204517970998,8.40164026751105));
#37005=CARTESIAN_POINT('Ctrl Pts',(7.27603390513779,-128.029517970998,4.20082013374682));
#37006=CARTESIAN_POINT('Ctrl Pts',(9.70137854017372,-127.854517970998,-1.72188171770438E-11));
#37007=CARTESIAN_POINT('Ctrl Pts',(7.27603390512276,-127.679517970998,-4.20082013377285));
#37008=CARTESIAN_POINT('Ctrl Pts',(4.85068927007213,-127.504517970998,-8.40164026752813));
#37009=CARTESIAN_POINT('Ctrl Pts',(-1.48666457128925E-11,-127.329517970998,
-8.40164026751963));
#37010=CARTESIAN_POINT('Ctrl Pts',(-4.85068927010187,-127.154517970998,
-8.40164026751096));
#37011=CARTESIAN_POINT('Ctrl Pts',(-7.27603390513763,-126.979517970998,
-4.2008201337471));
#37012=CARTESIAN_POINT('Ctrl Pts',(-9.70137854017372,-126.804517970998,
1.71142304400974E-11));
#37013=CARTESIAN_POINT('Ctrl Pts',(-7.27603390512281,-126.629517970998,
4.20082013377278));
#37014=CARTESIAN_POINT('Ctrl Pts',(-4.85068927007175,-126.454517970998,
8.40164026752835));
#37015=CARTESIAN_POINT('Ctrl Pts',(1.47760709417981E-11,-126.279517970998,
8.40164026751963));
#37016=CARTESIAN_POINT('Ctrl Pts',(4.85068927010178,-126.104517970998,8.40164026751101));
#37017=CARTESIAN_POINT('Ctrl Pts',(7.27603390513782,-125.929517970998,4.20082013374677));
#37018=CARTESIAN_POINT('Ctrl Pts',(9.70137854017372,-125.754517970998,-1.70096437031511E-11));
#37019=CARTESIAN_POINT('Ctrl Pts',(7.27603390512285,-125.579517970998,-4.2008201337727));
#37020=CARTESIAN_POINT('Ctrl Pts',(4.85068927007184,-125.404517970998,-8.4016402675283));
#37021=CARTESIAN_POINT('Ctrl Pts',(-1.46854961707036E-11,-125.229517970998,
-8.40164026751963));
#37022=CARTESIAN_POINT('Ctrl Pts',(-4.85068927010169,-125.054517970998,
-8.40164026751107));
#37023=CARTESIAN_POINT('Ctrl Pts',(-7.27603390513778,-124.879517970998,
-4.20082013374685));
#37024=CARTESIAN_POINT('Ctrl Pts',(-9.70137854017372,-124.704517970998,
1.74565164900911E-11));
#37025=CARTESIAN_POINT('Ctrl Pts',(-7.27603390512289,-124.529517970998,
4.20082013377262));
#37026=CARTESIAN_POINT('Ctrl Pts',(-4.85068927007193,-124.354517970998,
8.40164026752825));
#37027=CARTESIAN_POINT('Ctrl Pts',(1.50724993564536E-11,-124.179517970998,
8.40164026751963));
#37028=CARTESIAN_POINT('Ctrl Pts',(4.8506892701016,-124.004517970998,8.40164026751112));
#37029=CARTESIAN_POINT('Ctrl Pts',(7.27603390513773,-123.829517970998,4.20082013374692));
#37030=CARTESIAN_POINT('Ctrl Pts',(9.70137854017372,-123.654517970998,-1.73519297531447E-11));
#37031=CARTESIAN_POINT('Ctrl Pts',(7.27603390512294,-123.479517970998,-4.20082013377254));
#37032=CARTESIAN_POINT('Ctrl Pts',(4.85068927007202,-123.304517970998,-8.4016402675282));
#37033=CARTESIAN_POINT('Ctrl Pts',(-1.49819245853592E-11,-123.129517970998,
-8.40164026751963));
#37034=CARTESIAN_POINT('Ctrl Pts',(-4.85068927010151,-122.954517970998,
-8.40164026751117));
#37035=CARTESIAN_POINT('Ctrl Pts',(-7.27603390513768,-122.779517970998,
-4.200820133747));
#37036=CARTESIAN_POINT('Ctrl Pts',(-9.70137854017372,-122.604517970998,
1.72473430161984E-11));
#37037=CARTESIAN_POINT('Ctrl Pts',(-7.27603390512275,-122.429517970998,
4.20082013377288));
#37038=CARTESIAN_POINT('Ctrl Pts',(-4.85068927007211,-122.254517970998,
8.40164026752814));
#37039=CARTESIAN_POINT('Ctrl Pts',(1.48913498142647E-11,-122.079517970998,
8.40164026751963));
#37040=CARTESIAN_POINT('Ctrl Pts',(4.85068927010189,-121.904517970998,8.40164026751095));
#37041=CARTESIAN_POINT('Ctrl Pts',(7.27603390513764,-121.729517970998,4.20082013374708));
#37042=CARTESIAN_POINT('Ctrl Pts',(9.70137854017372,-121.554517970999,-1.7142756279252E-11));
#37043=CARTESIAN_POINT('Ctrl Pts',(7.27603390512279,-121.379517970998,-4.2008201337728));
#37044=CARTESIAN_POINT('Ctrl Pts',(4.8506892700722,-121.204517970998,-8.40164026752809));
#37045=CARTESIAN_POINT('Ctrl Pts',(-1.48007750431702E-11,-121.029517970998,
-8.40164026751963));
#37046=CARTESIAN_POINT('Ctrl Pts',(-4.8506892701018,-120.854517970999,-8.401640267511));
#37047=CARTESIAN_POINT('Ctrl Pts',(-7.27603390513783,-120.679517970999,
-4.20082013374675));
#37048=CARTESIAN_POINT('Ctrl Pts',(-9.70137854017372,-120.504517970999,
1.70381695423057E-11));
#37049=CARTESIAN_POINT('Ctrl Pts',(-7.27603390512284,-120.329517970998,
4.20082013377272));
#37050=CARTESIAN_POINT('Ctrl Pts',(-4.85068927007181,-120.154517970998,
8.40164026752832));
#37051=CARTESIAN_POINT('Ctrl Pts',(1.47102002720758E-11,-119.979517970999,
8.40164026751963));
#37052=CARTESIAN_POINT('Ctrl Pts',(4.85068927010171,-119.804517970999,8.40164026751105));
#37053=CARTESIAN_POINT('Ctrl Pts',(7.27603390513779,-119.629517970998,4.20082013374683));
#37054=CARTESIAN_POINT('Ctrl Pts',(9.70137854017372,-119.454517970998,-1.69335828053594E-11));
#37055=CARTESIAN_POINT('Ctrl Pts',(7.27603390512288,-119.279517970999,-4.20082013377264));
#37056=CARTESIAN_POINT('Ctrl Pts',(4.8506892700719,-119.104517970999,-8.40164026752826));
#37057=CARTESIAN_POINT('Ctrl Pts',(-1.50972034578258E-11,-118.929517970998,
-8.40164026751963));
#37058=CARTESIAN_POINT('Ctrl Pts',(-4.85068927010162,-118.754517970998,
-8.40164026751111));
#37059=CARTESIAN_POINT('Ctrl Pts',(-7.27603390513774,-118.579517970998,
-4.2008201337469));
#37060=CARTESIAN_POINT('Ctrl Pts',(-9.70137854017372,-118.404517970999,
1.73804555922994E-11));
#37061=CARTESIAN_POINT('Ctrl Pts',(-7.27603390512293,-118.229517970998,
4.20082013377256));
#37062=CARTESIAN_POINT('Ctrl Pts',(-4.85068927007199,-118.054517970998,
8.40164026752821));
#37063=CARTESIAN_POINT('Ctrl Pts',(1.50066286867313E-11,-117.879517970999,
8.40164026751963));
#37064=CARTESIAN_POINT('Ctrl Pts',(4.85068927010153,-117.704517970998,8.40164026751116));
#37065=CARTESIAN_POINT('Ctrl Pts',(7.2760339051377,-117.529517970998,4.20082013374698));
#37066=CARTESIAN_POINT('Ctrl Pts',(9.70137854017372,-117.354517970999,-1.7275868855353E-11));
#37067=CARTESIAN_POINT('Ctrl Pts',(7.27603390512297,-117.179517970999,-4.20082013377248));
#37068=CARTESIAN_POINT('Ctrl Pts',(4.85068927007208,-117.004517970999,-8.40164026752816));
#37069=CARTESIAN_POINT('Ctrl Pts',(-1.49160539156369E-11,-116.829517970998,
-8.40164026751963));
#37070=CARTESIAN_POINT('Ctrl Pts',(-4.85068927010192,-116.654517970998,
-8.40164026751093));
#37071=CARTESIAN_POINT('Ctrl Pts',(-7.27603390513765,-116.479517970999,
-4.20082013374706));
#37072=CARTESIAN_POINT('Ctrl Pts',(-9.70137854017372,-116.304517970999,
1.71712821184067E-11));
#37073=CARTESIAN_POINT('Ctrl Pts',(-7.27603390512278,-116.129517970999,
4.20082013377282));
#37074=CARTESIAN_POINT('Ctrl Pts',(-4.85068927007218,-115.954517970998,
8.40164026752811));
#37075=CARTESIAN_POINT('Ctrl Pts',(1.48254791445424E-11,-115.779517970998,
8.40164026751963));
#37076=CARTESIAN_POINT('Ctrl Pts',(4.85068927010183,-115.604517970999,8.40164026751099));
#37077=CARTESIAN_POINT('Ctrl Pts',(7.27603390513761,-115.429517970999,4.20082013374714));
#37078=CARTESIAN_POINT('Ctrl Pts',(9.70137854017372,-115.254517970999,-1.70666953814603E-11));
#37079=CARTESIAN_POINT('Ctrl Pts',(7.27603390512282,-115.079517970998,-4.20082013377274));
#37080=CARTESIAN_POINT('Ctrl Pts',(4.85068927007179,-114.904517970999,-8.40164026752833));
#37081=CARTESIAN_POINT('Ctrl Pts',(-1.4734904373448E-11,-114.729517970999,
-8.40164026751963));
#37082=CARTESIAN_POINT('Ctrl Pts',(-4.85068927010174,-114.554517970999,
-8.40164026751104));
#37083=CARTESIAN_POINT('Ctrl Pts',(-7.2760339051378,-114.379517970999,-4.2008201337468));
#37084=CARTESIAN_POINT('Ctrl Pts',(-9.70137854017372,-114.204517970999,
1.6962108644514E-11));
#37085=CARTESIAN_POINT('Ctrl Pts',(-7.27603390512287,-114.029517970999,
4.20082013377266));
#37086=CARTESIAN_POINT('Ctrl Pts',(-4.85068927007188,-113.854517970998,
8.40164026752828));
#37087=CARTESIAN_POINT('Ctrl Pts',(1.46443296023535E-11,-113.679517970999,
8.40164026751963));
#37088=CARTESIAN_POINT('Ctrl Pts',(4.85068927010165,-113.504517970999,8.40164026751109));
#37089=CARTESIAN_POINT('Ctrl Pts',(7.27603390513775,-113.329517970999,4.20082013374688));
#37090=CARTESIAN_POINT('Ctrl Pts',(9.70137854017372,-113.154517970999,-1.7408981431454E-11));
#37091=CARTESIAN_POINT('Ctrl Pts',(7.27603390512292,-112.979517970999,-4.20082013377258));
#37092=CARTESIAN_POINT('Ctrl Pts',(4.85068927007197,-112.804517970999,-8.40164026752823));
#37093=CARTESIAN_POINT('Ctrl Pts',(-1.50313327881035E-11,-112.629517970999,
-8.40164026751963));
#37094=CARTESIAN_POINT('Ctrl Pts',(-4.85068927010155,-112.454517970999,
-8.40164026751114));
#37095=CARTESIAN_POINT('Ctrl Pts',(-7.27603390513771,-112.279517970998,
-4.20082013374696));
#37096=CARTESIAN_POINT('Ctrl Pts',(-9.70137854017372,-112.104517970999,
1.73043946945076E-11));
#37097=CARTESIAN_POINT('Ctrl Pts',(-7.27603390512296,-111.929517970999,
4.2008201337725));
#37098=CARTESIAN_POINT('Ctrl Pts',(-4.85068927007206,-111.754517970999,
8.40164026752817));
#37099=CARTESIAN_POINT('Ctrl Pts',(1.49407580170091E-11,-111.579517970999,
8.40164026751963));
#37100=CARTESIAN_POINT('Ctrl Pts',(4.85068927010194,-111.404517970998,8.40164026751092));
#37101=CARTESIAN_POINT('Ctrl Pts',(7.27603390513766,-111.229517970999,4.20082013374704));
#37102=CARTESIAN_POINT('Ctrl Pts',(9.70137854017372,-111.054517970999,-1.71998079575613E-11));
#37103=CARTESIAN_POINT('Ctrl Pts',(7.27603390512277,-110.879517970999,-4.20082013377284));
#37104=CARTESIAN_POINT('Ctrl Pts',(4.85068927007215,-110.704517970999,-8.40164026752812));
#37105=CARTESIAN_POINT('Ctrl Pts',(-1.48501832459146E-11,-110.529517970999,
-8.40164026751963));
#37106=CARTESIAN_POINT('Ctrl Pts',(-4.85068927010185,-110.354517970999,
-8.40164026751097));
#37107=CARTESIAN_POINT('Ctrl Pts',(-7.27603390513762,-110.179517970999,
-4.20082013374712));
#37108=CARTESIAN_POINT('Ctrl Pts',(-9.70137854017372,-110.004517970999,
1.7095221220615E-11));
#37109=CARTESIAN_POINT('Ctrl Pts',(-7.27603390512281,-109.829517970999,
4.20082013377276));
#37110=CARTESIAN_POINT('Ctrl Pts',(-4.85068927007224,-109.654517970999,
8.40164026752807));
#37111=CARTESIAN_POINT('Ctrl Pts',(1.47596084748201E-11,-109.479517970999,
8.40164026751963));
#37112=CARTESIAN_POINT('Ctrl Pts',(4.85068927010176,-109.304517970999,8.40164026751102));
#37113=CARTESIAN_POINT('Ctrl Pts',(7.27603390513781,-109.129517970999,4.20082013374678));
#37114=CARTESIAN_POINT('Ctrl Pts',(9.70137854017372,-108.954517970999,-1.69906344836686E-11));
#37115=CARTESIAN_POINT('Ctrl Pts',(7.27603390512286,-108.779517970999,-4.20082013377268));
#37116=CARTESIAN_POINT('Ctrl Pts',(4.85068927007186,-108.604517970999,-8.40164026752829));
#37117=CARTESIAN_POINT('Ctrl Pts',(-1.46690337037257E-11,-108.429517970999,
-8.40164026751963));
#37118=CARTESIAN_POINT('Ctrl Pts',(-4.85068927010167,-108.254517970999,
-8.40164026751108));
#37119=CARTESIAN_POINT('Ctrl Pts',(-7.27603390513777,-108.079517970999,
-4.20082013374686));
#37120=CARTESIAN_POINT('Ctrl Pts',(-9.70137854017372,-107.904517970999,
1.68860477467223E-11));
#37121=CARTESIAN_POINT('Ctrl Pts',(-7.2760339051229,-107.729517970999,4.2008201337726));
#37122=CARTESIAN_POINT('Ctrl Pts',(-4.85068927007195,-107.554517970999,
8.40164026752824));
#37123=CARTESIAN_POINT('Ctrl Pts',(1.50560368894757E-11,-107.379517970999,
8.40164026751963));
#37124=CARTESIAN_POINT('Ctrl Pts',(4.85068927010158,-107.204517970999,8.40164026751113));
#37125=CARTESIAN_POINT('Ctrl Pts',(7.27603390513772,-107.029517970999,4.20082013374694));
#37126=CARTESIAN_POINT('Ctrl Pts',(9.70137854017372,-106.854517970999,-1.73329205336623E-11));
#37127=CARTESIAN_POINT('Ctrl Pts',(7.27603390512295,-106.679517970999,-4.20082013377253));
#37128=CARTESIAN_POINT('Ctrl Pts',(4.85068927007204,-106.504517970998,-8.40164026752819));
#37129=CARTESIAN_POINT('Ctrl Pts',(-1.49654621183812E-11,-106.329517970999,
-8.40164026751963));
#37130=CARTESIAN_POINT('Ctrl Pts',(-4.85068927010149,-106.154517970999,
-8.40164026751118));
#37131=CARTESIAN_POINT('Ctrl Pts',(-7.27603390513768,-105.979517970999,
-4.20082013374702));
#37132=CARTESIAN_POINT('Ctrl Pts',(-9.70137854017372,-105.804517970999,
1.72283337967159E-11));
#37133=CARTESIAN_POINT('Ctrl Pts',(-7.27603390512276,-105.629517970999,
4.20082013377286));
#37134=CARTESIAN_POINT('Ctrl Pts',(-4.85068927007213,-105.454517970999,
8.40164026752814));
#37135=CARTESIAN_POINT('Ctrl Pts',(1.48748873472868E-11,-105.279517970999,
8.40164026751963));
#37136=CARTESIAN_POINT('Ctrl Pts',(4.85068927010188,-105.104517970999,8.40164026751096));
#37137=CARTESIAN_POINT('Ctrl Pts',(7.27603390513763,-104.929517970999,4.2008201337471));
#37138=CARTESIAN_POINT('Ctrl Pts',(9.70137854017372,-104.754517970999,-1.71237470597696E-11));
#37139=CARTESIAN_POINT('Ctrl Pts',(7.2760339051228,-104.579517970999,-4.20082013377278));
#37140=CARTESIAN_POINT('Ctrl Pts',(4.85068927007222,-104.404517970999,-8.40164026752808));
#37141=CARTESIAN_POINT('Ctrl Pts',(-1.47843125761923E-11,-104.229517970999,
-8.40164026751963));
#37142=CARTESIAN_POINT('Ctrl Pts',(-4.85068927010179,-104.054517970999,
-8.40164026751101));
#37143=CARTESIAN_POINT('Ctrl Pts',(-7.27603390513758,-103.879517970999,
-4.20082013374717));
#37144=CARTESIAN_POINT('Ctrl Pts',(-9.70137854017372,-103.704517970999,
1.70191603228232E-11));
#37145=CARTESIAN_POINT('Ctrl Pts',(-7.27603390512285,-103.529517970999,
4.20082013377271));
#37146=CARTESIAN_POINT('Ctrl Pts',(-4.85068927007183,-103.354517970999,
8.40164026752831));
#37147=CARTESIAN_POINT('Ctrl Pts',(1.46937378050979E-11,-103.179517970999,
8.40164026751963));
#37148=CARTESIAN_POINT('Ctrl Pts',(4.85068927010169,-103.004517970999,8.40164026751106));
#37149=CARTESIAN_POINT('Ctrl Pts',(7.27603390513778,-102.829517970999,4.20082013374684));
#37150=CARTESIAN_POINT('Ctrl Pts',(9.70137854017372,-102.654517970999,-1.69145735858769E-11));
#37151=CARTESIAN_POINT('Ctrl Pts',(7.27603390512289,-102.479517970999,-4.20082013377263));
#37152=CARTESIAN_POINT('Ctrl Pts',(4.85068927007192,-102.304517970999,-8.40164026752825));
#37153=CARTESIAN_POINT('Ctrl Pts',(-1.46031630340034E-11,-102.129517970999,
-8.40164026751963));
#37154=CARTESIAN_POINT('Ctrl Pts',(-4.8506892701016,-101.954517970999,-8.40164026751111));
#37155=CARTESIAN_POINT('Ctrl Pts',(-7.27603390513773,-101.779517970999,
-4.20082013374692));
#37156=CARTESIAN_POINT('Ctrl Pts',(-9.70137854017372,-101.604517970999,
1.73614463728169E-11));
#37157=CARTESIAN_POINT('Ctrl Pts',(-7.27603390512294,-101.429517970999,
4.20082013377255));
#37158=CARTESIAN_POINT('Ctrl Pts',(-4.85068927007201,-101.254517970999,
8.4016402675282));
#37159=CARTESIAN_POINT('Ctrl Pts',(1.49901662197534E-11,-101.079517970999,
8.40164026751963));
#37160=CARTESIAN_POINT('Ctrl Pts',(4.85068927010151,-100.904517970999,8.40164026751117));
#37161=CARTESIAN_POINT('Ctrl Pts',(7.27603390513769,-100.729517970999,4.200820133747));
#37162=CARTESIAN_POINT('Ctrl Pts',(9.70137854017372,-100.554517970999,-1.72568596358705E-11));
#37163=CARTESIAN_POINT('Ctrl Pts',(7.27603390512298,-100.379517970999,-4.20082013377247));
#37164=CARTESIAN_POINT('Ctrl Pts',(4.8506892700721,-100.204517970999,-8.40164026752815));
#37165=CARTESIAN_POINT('Ctrl Pts',(-1.48995914486589E-11,-100.029517970999,
-8.40164026751963));
#37166=CARTESIAN_POINT('Ctrl Pts',(-4.8506892701019,-99.8545179709985,-8.40164026751094));
#37167=CARTESIAN_POINT('Ctrl Pts',(-7.27603390513764,-99.6795179709985,
-4.20082013374707));
#37168=CARTESIAN_POINT('Ctrl Pts',(-9.70137854017372,-99.5045179709985,
1.71522728989242E-11));
#37169=CARTESIAN_POINT('Ctrl Pts',(-7.27603390512279,-99.3295179709985,
4.2008201337728));
#37170=CARTESIAN_POINT('Ctrl Pts',(-4.85068927007219,-99.1545179709985,
8.4016402675281));
#37171=CARTESIAN_POINT('Ctrl Pts',(1.48090166775645E-11,-98.9795179709985,
8.40164026751963));
#37172=CARTESIAN_POINT('Ctrl Pts',(4.85068927010181,-98.8045179709985,8.401640267511));
#37173=CARTESIAN_POINT('Ctrl Pts',(7.2760339051376,-98.6295179709985,4.20082013374715));
#37174=CARTESIAN_POINT('Ctrl Pts',(9.70137854017372,-98.4545179709986,-1.70476861619779E-11));
#37175=CARTESIAN_POINT('Ctrl Pts',(7.27603390512283,-98.2795179709986,-4.20082013377273));
#37176=CARTESIAN_POINT('Ctrl Pts',(4.85068927007228,-98.1045179709985,-8.40164026752804));
#37177=CARTESIAN_POINT('Ctrl Pts',(-1.471844190647E-11,-97.9295179709985,
-8.40164026751963));
#37178=CARTESIAN_POINT('Ctrl Pts',(-4.85068927010172,-97.7545179709985,
-8.40164026751105));
#37179=CARTESIAN_POINT('Ctrl Pts',(-7.27603390513779,-97.5795179709986,
-4.20082013374682));
#37180=CARTESIAN_POINT('Ctrl Pts',(-9.70137854017372,-97.4045179709985,
1.69430994250315E-11));
#37181=CARTESIAN_POINT('Ctrl Pts',(-7.27603390512288,-97.2295179709985,
4.20082013377265));
#37182=CARTESIAN_POINT('Ctrl Pts',(-4.8506892700719,-97.0545179709985,8.40164026752827));
#37183=CARTESIAN_POINT('Ctrl Pts',(1.46278671353756E-11,-96.8795179709986,
8.40164026751963));
#37184=CARTESIAN_POINT('Ctrl Pts',(4.85068927010163,-96.7045179709986,8.4016402675111));
#37185=CARTESIAN_POINT('Ctrl Pts',(7.27603390513774,-96.5295179709985,4.2008201337469));
#37186=CARTESIAN_POINT('Ctrl Pts',(9.70137854017372,-96.3545179709985,-1.68385126880852E-11));
#37187=CARTESIAN_POINT('Ctrl Pts',(7.27603390512292,-96.1795179709985,-4.20082013377257));
#37188=CARTESIAN_POINT('Ctrl Pts',(4.85068927007199,-96.0045179709986,-8.40164026752822));
#37189=CARTESIAN_POINT('Ctrl Pts',(-1.50148703211256E-11,-95.8295179709985,
-8.40164026751963));
#37190=CARTESIAN_POINT('Ctrl Pts',(-4.85068927010154,-95.6545179709985,
-8.40164026751115));
#37191=CARTESIAN_POINT('Ctrl Pts',(-7.2760339051377,-95.4795179709985,-4.20082013374698));
#37192=CARTESIAN_POINT('Ctrl Pts',(-9.70137854017372,-95.3045179709985,
1.72853854750252E-11));
#37193=CARTESIAN_POINT('Ctrl Pts',(-7.27603390512297,-95.1295179709986,
4.20082013377249));
#37194=CARTESIAN_POINT('Ctrl Pts',(-4.85068927007208,-94.9545179709986,
8.40164026752816));
#37195=CARTESIAN_POINT('Ctrl Pts',(1.49242955500311E-11,-94.7795179709985,
8.40164026751963));
#37196=CARTESIAN_POINT('Ctrl Pts',(4.85068927010145,-94.6045179709986,8.40164026751121));
#37197=CARTESIAN_POINT('Ctrl Pts',(7.27603390513766,-94.4295179709985,4.20082013374705));
#37198=CARTESIAN_POINT('Ctrl Pts',(9.70137854017372,-94.2545179709985,-1.71807987380788E-11));
#37199=CARTESIAN_POINT('Ctrl Pts',(7.27603390512277,-94.0795179709986,-4.20082013377283));
#37200=CARTESIAN_POINT('Ctrl Pts',(4.85068927007217,-93.9045179709986,-8.40164026752811));
#37201=CARTESIAN_POINT('Ctrl Pts',(-1.48337207789367E-11,-93.7295179709986,
-8.40164026751963));
#37202=CARTESIAN_POINT('Ctrl Pts',(-4.85068927010184,-93.5545179709985,
-8.40164026751098));
#37203=CARTESIAN_POINT('Ctrl Pts',(-7.27603390513761,-93.3795179709985,
-4.20082013374713));
#37204=CARTESIAN_POINT('Ctrl Pts',(-9.70137854017372,-93.2045179709986,
1.70762120011325E-11));
#37205=CARTESIAN_POINT('Ctrl Pts',(-7.27603390512282,-93.0295179709986,
4.20082013377275));
#37206=CARTESIAN_POINT('Ctrl Pts',(-4.85068927007226,-92.8545179709985,
8.40164026752806));
#37207=CARTESIAN_POINT('Ctrl Pts',(1.47431460078422E-11,-92.6795179709985,
8.40164026751963));
#37208=CARTESIAN_POINT('Ctrl Pts',(4.85068927010175,-92.5045179709985,8.40164026751103));
#37209=CARTESIAN_POINT('Ctrl Pts',(7.2760339051378,-92.3295179709986,4.2008201337468));
#37210=CARTESIAN_POINT('Ctrl Pts',(9.70137854017372,-92.1545179709986,-1.69716252641861E-11));
#37211=CARTESIAN_POINT('Ctrl Pts',(7.27603390512287,-91.9795179709986,-4.20082013377267));
#37212=CARTESIAN_POINT('Ctrl Pts',(4.85068927007187,-91.8045179709985,-8.40164026752828));
#37213=CARTESIAN_POINT('Ctrl Pts',(-1.46525712367478E-11,-91.6295179709986,
-8.40164026751963));
#37214=CARTESIAN_POINT('Ctrl Pts',(-4.85068927010165,-91.4545179709986,
-8.40164026751109));
#37215=CARTESIAN_POINT('Ctrl Pts',(-7.27603390513776,-91.2795179709986,
-4.20082013374688));
#37216=CARTESIAN_POINT('Ctrl Pts',(-9.70137854017372,-91.1045179709986,
1.68670385272398E-11));
#37217=CARTESIAN_POINT('Ctrl Pts',(-7.27603390512291,-90.9295179709986,
4.20082013377259));
#37218=CARTESIAN_POINT('Ctrl Pts',(-4.85068927007196,-90.7545179709986,
8.40164026752823));
#37219=CARTESIAN_POINT('Ctrl Pts',(1.45619964656533E-11,-90.5795179709986,
8.40164026751963));
#37220=CARTESIAN_POINT('Ctrl Pts',(4.85068927010157,-90.4045179709985,8.40164026751114));
#37221=CARTESIAN_POINT('Ctrl Pts',(7.27603390513771,-90.2295179709986,4.20082013374695));
#37222=CARTESIAN_POINT('Ctrl Pts',(9.70137854017372,-90.0545179709986,-1.73139113141798E-11));
#37223=CARTESIAN_POINT('Ctrl Pts',(7.27603390512296,-89.8795179709985,-4.20082013377251));
#37224=CARTESIAN_POINT('Ctrl Pts',(4.85068927007205,-89.7045179709986,-8.40164026752818));
#37225=CARTESIAN_POINT('Ctrl Pts',(-1.49489996514033E-11,-89.5295179709986,
-8.40164026751963));
#37226=CARTESIAN_POINT('Ctrl Pts',(-4.85068927010147,-89.3545179709986,
-8.40164026751119));
#37227=CARTESIAN_POINT('Ctrl Pts',(-7.27603390513767,-89.1795179709986,
-4.20082013374703));
#37228=CARTESIAN_POINT('Ctrl Pts',(-9.70137854017372,-89.0045179709985,
1.72093245772335E-11));
#37229=CARTESIAN_POINT('Ctrl Pts',(-7.276033905123,-88.8295179709986,4.20082013377243));
#37230=CARTESIAN_POINT('Ctrl Pts',(-4.85068927007214,-88.6545179709986,
8.40164026752813));
#37231=CARTESIAN_POINT('Ctrl Pts',(1.48584248803088E-11,-88.4795179709986,
8.40164026751963));
#37232=CARTESIAN_POINT('Ctrl Pts',(4.85068927010186,-88.3045179709985,8.40164026751097));
#37233=CARTESIAN_POINT('Ctrl Pts',(7.27603390513762,-88.1295179709985,4.20082013374711));
#37234=CARTESIAN_POINT('Ctrl Pts',(9.70137854017372,-87.9545179709986,-1.71047378402871E-11));
#37235=CARTESIAN_POINT('Ctrl Pts',(7.27603390512281,-87.7795179709986,-4.20082013377277));
#37236=CARTESIAN_POINT('Ctrl Pts',(4.85068927007223,-87.6045179709986,-8.40164026752807));
#37237=CARTESIAN_POINT('Ctrl Pts',(-1.47678501092144E-11,-87.4295179709986,
-8.40164026751963));
#37238=CARTESIAN_POINT('Ctrl Pts',(-4.85068927010177,-87.2545179709985,
-8.40164026751102));
#37239=CARTESIAN_POINT('Ctrl Pts',(-7.27603390513758,-87.0795179709986,
-4.20082013374719));
#37240=CARTESIAN_POINT('Ctrl Pts',(-9.70137854017372,-86.9045179709986,
1.70001511033408E-11));
#37241=CARTESIAN_POINT('Ctrl Pts',(-7.27603390512285,-86.7295179709986,
4.20082013377269));
#37242=CARTESIAN_POINT('Ctrl Pts',(-4.85068927007185,-86.5545179709986,
8.4016402675283));
#37243=CARTESIAN_POINT('Ctrl Pts',(1.46772753381199E-11,-86.3795179709986,
8.40164026751963));
#37244=CARTESIAN_POINT('Ctrl Pts',(4.85068927010168,-86.2045179709986,8.40164026751107));
#37245=CARTESIAN_POINT('Ctrl Pts',(7.27603390513777,-86.0295179709986,4.20082013374685));
#37246=CARTESIAN_POINT('Ctrl Pts',(9.70137854017372,-85.8545179709986,-1.68955643663944E-11));
#37247=CARTESIAN_POINT('Ctrl Pts',(7.2760339051229,-85.6795179709986,-4.20082013377261));
#37248=CARTESIAN_POINT('Ctrl Pts',(4.85068927007194,-85.5045179709986,-8.40164026752825));
#37249=CARTESIAN_POINT('Ctrl Pts',(-1.45867005670255E-11,-85.3295179709986,
-8.40164026751963));
#37250=CARTESIAN_POINT('Ctrl Pts',(-4.85068927010159,-85.1545179709986,
-8.40164026751112));
#37251=CARTESIAN_POINT('Ctrl Pts',(-7.27603390513773,-84.9795179709986,
-4.20082013374693));
#37252=CARTESIAN_POINT('Ctrl Pts',(-9.70137854017372,-84.8045179709986,
1.67909776294481E-11));
#37253=CARTESIAN_POINT('Ctrl Pts',(-7.27603390512294,-84.6295179709986,
4.20082013377253));
#37254=CARTESIAN_POINT('Ctrl Pts',(-4.85068927007203,-84.4545179709986,
8.40164026752819));
#37255=CARTESIAN_POINT('Ctrl Pts',(1.49737037527755E-11,-84.2795179709986,
8.40164026751963));
#37256=CARTESIAN_POINT('Ctrl Pts',(4.8506892701015,-84.1045179709986,8.40164026751117));
#37257=CARTESIAN_POINT('Ctrl Pts',(7.27603390513768,-83.9295179709986,4.20082013374701));
#37258=CARTESIAN_POINT('Ctrl Pts',(9.70137854017372,-83.7545179709986,-1.72378504163881E-11));
#37259=CARTESIAN_POINT('Ctrl Pts',(7.27603390512299,-83.5795179709986,-4.20082013377245));
#37260=CARTESIAN_POINT('Ctrl Pts',(4.85068927007212,-83.4045179709986,-8.40164026752814));
#37261=CARTESIAN_POINT('Ctrl Pts',(-1.4883128981681E-11,-83.2295179709986,
-8.40164026751963));
#37262=CARTESIAN_POINT('Ctrl Pts',(-4.85068927010141,-83.0545179709986,
-8.40164026751123));
#37263=CARTESIAN_POINT('Ctrl Pts',(-7.27603390513763,-82.8795179709986,
-4.20082013374709));
#37264=CARTESIAN_POINT('Ctrl Pts',(-9.70137854017372,-82.7045179709986,
1.71332636794417E-11));
#37265=CARTESIAN_POINT('Ctrl Pts',(-7.2760339051228,-82.5295179709986,4.20082013377279));
#37266=CARTESIAN_POINT('Ctrl Pts',(-4.85068927007221,-82.3545179709986,
8.40164026752809));
#37267=CARTESIAN_POINT('Ctrl Pts',(1.47925542105866E-11,-82.1795179709986,
8.40164026751963));
#37268=CARTESIAN_POINT('Ctrl Pts',(4.85068927010179,-82.0045179709986,8.401640267511));
#37269=CARTESIAN_POINT('Ctrl Pts',(7.27603390513759,-81.8295179709986,4.20082013374717));
#37270=CARTESIAN_POINT('Ctrl Pts',(9.70137854017372,-81.6545179709986,-1.70286769424954E-11));
#37271=CARTESIAN_POINT('Ctrl Pts',(7.27603390512284,-81.4795179709986,-4.20082013377271));
#37272=CARTESIAN_POINT('Ctrl Pts',(4.8506892700723,-81.3045179709986,-8.40164026752804));
#37273=CARTESIAN_POINT('Ctrl Pts',(-1.47019794394921E-11,-81.1295179709986,
-8.40164026751963));
#37274=CARTESIAN_POINT('Ctrl Pts',(-4.8506892701017,-80.9545179709986,-8.40164026751106));
#37275=CARTESIAN_POINT('Ctrl Pts',(-7.27603390513778,-80.7795179709986,
-4.20082013374683));
#37276=CARTESIAN_POINT('Ctrl Pts',(-9.70137854017372,-80.6045179709986,
1.69240902055491E-11));
#37277=CARTESIAN_POINT('Ctrl Pts',(-7.27603390512289,-80.4295179709986,
4.20082013377263));
#37278=CARTESIAN_POINT('Ctrl Pts',(-4.85068927007191,-80.2545179709986,
8.40164026752826));
#37279=CARTESIAN_POINT('Ctrl Pts',(1.46114046683977E-11,-80.0795179709986,
8.40164026751963));
#37280=CARTESIAN_POINT('Ctrl Pts',(4.85068927010161,-79.9045179709986,8.40164026751111));
#37281=CARTESIAN_POINT('Ctrl Pts',(7.27603390513774,-79.7295179709986,4.20082013374691));
#37282=CARTESIAN_POINT('Ctrl Pts',(9.70137854017372,-79.5545179709986,-1.68195034686027E-11));
#37283=CARTESIAN_POINT('Ctrl Pts',(7.27603390512293,-79.3795179709986,-4.20082013377256));
#37284=CARTESIAN_POINT('Ctrl Pts',(4.850689270072,-79.2045179709986,-8.40164026752821));
#37285=CARTESIAN_POINT('Ctrl Pts',(-1.49984078541476E-11,-79.0295179709986,
-8.40164026751963));
#37286=CARTESIAN_POINT('Ctrl Pts',(-4.85068927010152,-78.8545179709986,
-8.40164026751116));
#37287=CARTESIAN_POINT('Ctrl Pts',(-7.27603390513769,-78.6795179709986,
-4.20082013374699));
#37288=CARTESIAN_POINT('Ctrl Pts',(-9.70137854017372,-78.5045179709986,
1.72663762555427E-11));
#37289=CARTESIAN_POINT('Ctrl Pts',(-7.27603390512298,-78.3295179709986,
4.20082013377248));
#37290=CARTESIAN_POINT('Ctrl Pts',(-4.85068927007209,-78.1545179709986,
8.40164026752815));
#37291=CARTESIAN_POINT('Ctrl Pts',(1.49078330830532E-11,-77.9795179709986,
8.40164026751963));
#37292=CARTESIAN_POINT('Ctrl Pts',(4.85068927010143,-77.8045179709986,8.40164026751122));
#37293=CARTESIAN_POINT('Ctrl Pts',(7.27603390513765,-77.6295179709986,4.20082013374707));
#37294=CARTESIAN_POINT('Ctrl Pts',(9.70137854017372,-77.4545179709986,-1.71617895185964E-11));
#37295=CARTESIAN_POINT('Ctrl Pts',(7.27603390512302,-77.2795179709986,-4.2008201337724));
#37296=CARTESIAN_POINT('Ctrl Pts',(4.85068927007219,-77.1045179709986,-8.4016402675281));
#37297=CARTESIAN_POINT('Ctrl Pts',(-1.48172583119587E-11,-76.9295179709986,
-8.40164026751963));
#37298=CARTESIAN_POINT('Ctrl Pts',(-4.85068927010182,-76.7545179709986,
-8.40164026751099));
#37299=CARTESIAN_POINT('Ctrl Pts',(-7.2760339051376,-76.5795179709986,-4.20082013374715));
#37300=CARTESIAN_POINT('Ctrl Pts',(-9.70137854017372,-76.4045179709986,
1.705720278165E-11));
#37301=CARTESIAN_POINT('Ctrl Pts',(-7.27603390512283,-76.2295179709986,
4.20082013377273));
#37302=CARTESIAN_POINT('Ctrl Pts',(-4.85068927007227,-76.0545179709986,
8.40164026752805));
#37303=CARTESIAN_POINT('Ctrl Pts',(1.47266835408643E-11,-75.8795179709986,
8.40164026751963));
#37304=CARTESIAN_POINT('Ctrl Pts',(4.85068927010173,-75.7045179709986,8.40164026751104));
#37305=CARTESIAN_POINT('Ctrl Pts',(7.27603390513756,-75.5295179709986,4.20082013374722));
#37306=CARTESIAN_POINT('Ctrl Pts',(9.70137854017372,-75.3545179709986,-1.69526160447037E-11));
#37307=CARTESIAN_POINT('Ctrl Pts',(7.27603390512287,-75.1795179709986,-4.20082013377265));
#37308=CARTESIAN_POINT('Ctrl Pts',(4.85068927007189,-75.0045179709986,-8.40164026752827));
#37309=CARTESIAN_POINT('Ctrl Pts',(-1.46361087697698E-11,-74.8295179709986,
-8.40164026751963));
#37310=CARTESIAN_POINT('Ctrl Pts',(-4.85068927010164,-74.6545179709986,
-8.40164026751109));
#37311=CARTESIAN_POINT('Ctrl Pts',(-7.27603390513775,-74.4795179709986,
-4.20082013374689));
#37312=CARTESIAN_POINT('Ctrl Pts',(-9.70137854017372,-74.3045179709986,
1.68480293077573E-11));
#37313=CARTESIAN_POINT('Ctrl Pts',(-7.27603390512292,-74.1295179709986,
4.20082013377258));
#37314=CARTESIAN_POINT('Ctrl Pts',(-4.85068927007198,-73.9545179709986,
8.40164026752822));
#37315=CARTESIAN_POINT('Ctrl Pts',(1.45455339986754E-11,-73.7795179709986,
8.40164026751963));
#37316=CARTESIAN_POINT('Ctrl Pts',(4.85068927010155,-73.6045179709986,8.40164026751115));
#37317=CARTESIAN_POINT('Ctrl Pts',(7.2760339051377,-73.4295179709986,4.20082013374697));
#37318=CARTESIAN_POINT('Ctrl Pts',(9.70137854017372,-73.2545179709986,-1.72949020946973E-11));
#37319=CARTESIAN_POINT('Ctrl Pts',(7.27603390512296,-73.0795179709986,-4.2008201337725));
#37320=CARTESIAN_POINT('Ctrl Pts',(4.85068927007207,-72.9045179709986,-8.40164026752817));
#37321=CARTESIAN_POINT('Ctrl Pts',(-1.49325371844254E-11,-72.7295179709986,
-8.40164026751963));
#37322=CARTESIAN_POINT('Ctrl Pts',(-4.85068927010146,-72.5545179709986,
-8.4016402675112));
#37323=CARTESIAN_POINT('Ctrl Pts',(-7.27603390513766,-72.3795179709986,
-4.20082013374705));
#37324=CARTESIAN_POINT('Ctrl Pts',(-9.70137854017372,-72.2045179709986,
1.7190315357751E-11));
#37325=CARTESIAN_POINT('Ctrl Pts',(-7.27603390512301,-72.0295179709986,
4.20082013377242));
#37326=CARTESIAN_POINT('Ctrl Pts',(-4.85068927007216,-71.8545179709986,
8.40164026752812));
#37327=CARTESIAN_POINT('Ctrl Pts',(1.48419624133309E-11,-71.6795179709986,
8.40164026751963));
#37328=CARTESIAN_POINT('Ctrl Pts',(4.85068927010137,-71.5045179709986,8.40164026751125));
#37329=CARTESIAN_POINT('Ctrl Pts',(7.27603390513761,-71.3295179709986,4.20082013374713));
#37330=CARTESIAN_POINT('Ctrl Pts',(9.70137854017372,-71.1545179709986,-1.70857286208046E-11));
#37331=CARTESIAN_POINT('Ctrl Pts',(7.27603390512282,-70.9795179709986,-4.20082013377275));
#37332=CARTESIAN_POINT('Ctrl Pts',(4.85068927007225,-70.8045179709986,-8.40164026752806));
#37333=CARTESIAN_POINT('Ctrl Pts',(-1.47513876422365E-11,-70.6295179709986,
-8.40164026751963));
#37334=CARTESIAN_POINT('Ctrl Pts',(-4.85068927010175,-70.4545179709986,
-8.40164026751103));
#37335=CARTESIAN_POINT('Ctrl Pts',(-7.27603390513757,-70.2795179709986,
-4.2008201337472));
#37336=CARTESIAN_POINT('Ctrl Pts',(-9.70137854017372,-70.1045179709986,
1.69811418838583E-11));
#37337=CARTESIAN_POINT('Ctrl Pts',(-7.27603390512286,-69.9295179709986,
4.20082013377267));
#37338=CARTESIAN_POINT('Ctrl Pts',(-4.85068927007234,-69.7545179709986,
8.40164026752801));
#37339=CARTESIAN_POINT('Ctrl Pts',(1.4660812871142E-11,-69.5795179709986,
8.40164026751963));
#37340=CARTESIAN_POINT('Ctrl Pts',(4.85068927010166,-69.4045179709986,8.40164026751108));
#37341=CARTESIAN_POINT('Ctrl Pts',(7.27603390513776,-69.2295179709986,4.20082013374687));
#37342=CARTESIAN_POINT('Ctrl Pts',(9.70137854017372,-69.0545179709986,-1.6876555146912E-11));
#37343=CARTESIAN_POINT('Ctrl Pts',(7.27603390512291,-68.8795179709986,-4.2008201337726));
#37344=CARTESIAN_POINT('Ctrl Pts',(4.85068927007195,-68.7045179709986,-8.40164026752823));
#37345=CARTESIAN_POINT('Ctrl Pts',(-1.45702381000475E-11,-68.5295179709986,
-8.40164026751963));
#37346=CARTESIAN_POINT('Ctrl Pts',(-4.85068927010157,-68.3545179709986,
-8.40164026751113));
#37347=CARTESIAN_POINT('Ctrl Pts',(-7.27603390513772,-68.1795179709986,
-4.20082013374695));
#37348=CARTESIAN_POINT('Ctrl Pts',(-9.70137854017372,-68.0045179709986,
1.67719684099656E-11));
#37349=CARTESIAN_POINT('Ctrl Pts',(-7.27603390512295,-67.8295179709986,
4.20082013377252));
#37350=CARTESIAN_POINT('Ctrl Pts',(-4.85068927007204,-67.6545179709986,
8.40164026752818));
#37351=CARTESIAN_POINT('Ctrl Pts',(1.49572412857975E-11,-67.4795179709986,
8.40164026751963));
#37352=CARTESIAN_POINT('Ctrl Pts',(4.85068927010148,-67.3045179709986,8.40164026751119));
#37353=CARTESIAN_POINT('Ctrl Pts',(7.27603390513767,-67.1295179709986,4.20082013374703));
#37354=CARTESIAN_POINT('Ctrl Pts',(9.70137854017372,-66.9545179709986,-1.72188411969056E-11));
#37355=CARTESIAN_POINT('Ctrl Pts',(7.276033905123,-66.7795179709986,-4.20082013377244));
#37356=CARTESIAN_POINT('Ctrl Pts',(4.85068927007213,-66.6045179709986,-8.40164026752813));
#37357=CARTESIAN_POINT('Ctrl Pts',(-1.48666665147031E-11,-66.4295179709986,
-8.40164026751963));
#37358=CARTESIAN_POINT('Ctrl Pts',(-4.85068927010139,-66.2545179709986,
-8.40164026751124));
#37359=CARTESIAN_POINT('Ctrl Pts',(-7.27603390513763,-66.0795179709986,
-4.2008201337471));
#37360=CARTESIAN_POINT('Ctrl Pts',(-9.70137854017372,-65.9045179709986,
1.71142544599593E-11));
#37361=CARTESIAN_POINT('Ctrl Pts',(-7.27603390512304,-65.7295179709986,
4.20082013377236));
#37362=CARTESIAN_POINT('Ctrl Pts',(-4.85068927007222,-65.5545179709986,
8.40164026752808));
#37363=CARTESIAN_POINT('Ctrl Pts',(1.47760917436086E-11,-65.3795179709986,
8.40164026751963));
#37364=CARTESIAN_POINT('Ctrl Pts',(4.85068927010178,-65.2045179709986,8.40164026751101));
#37365=CARTESIAN_POINT('Ctrl Pts',(7.27603390513758,-65.0295179709986,4.20082013374718));
#37366=CARTESIAN_POINT('Ctrl Pts',(9.70137854017372,-64.8545179709986,-1.70096677230129E-11));
#37367=CARTESIAN_POINT('Ctrl Pts',(7.27603390512285,-64.6795179709986,-4.2008201337727));
#37368=CARTESIAN_POINT('Ctrl Pts',(4.85068927007232,-64.5045179709986,-8.40164026752803));
#37369=CARTESIAN_POINT('Ctrl Pts',(-1.46855169725142E-11,-64.3295179709986,
-8.40164026751963));
#37370=CARTESIAN_POINT('Ctrl Pts',(-4.85068927010169,-64.1545179709986,
-8.40164026751107));
#37371=CARTESIAN_POINT('Ctrl Pts',(-7.27603390513754,-63.9795179709986,
-4.20082013374726));
#37372=CARTESIAN_POINT('Ctrl Pts',(-9.70137854017372,-63.8045179709986,
1.69050809860666E-11));
#37373=CARTESIAN_POINT('Ctrl Pts',(-7.27603390512289,-63.6295179709986,
4.20082013377262));
#37374=CARTESIAN_POINT('Ctrl Pts',(-4.85068927007193,-63.4545179709986,
8.40164026752825));
#37375=CARTESIAN_POINT('Ctrl Pts',(1.45949422014197E-11,-63.2795179709986,
8.40164026751963));
#37376=CARTESIAN_POINT('Ctrl Pts',(4.8506892701016,-63.1045179709986,8.40164026751112));
#37377=CARTESIAN_POINT('Ctrl Pts',(7.27603390513773,-62.9295179709986,4.20082013374692));
#37378=CARTESIAN_POINT('Ctrl Pts',(9.70137854017372,-62.7545179709986,-1.68004942491202E-11));
#37379=CARTESIAN_POINT('Ctrl Pts',(7.27603390512294,-62.5795179709986,-4.20082013377254));
#37380=CARTESIAN_POINT('Ctrl Pts',(4.85068927007202,-62.4045179709986,-8.4016402675282));
#37381=CARTESIAN_POINT('Ctrl Pts',(-1.45043674303253E-11,-62.2295179709986,
-8.40164026751963));
#37382=CARTESIAN_POINT('Ctrl Pts',(-4.85068927010151,-62.0545179709986,
-8.40164026751117));
#37383=CARTESIAN_POINT('Ctrl Pts',(-7.27603390513768,-61.8795179709986,
-4.200820133747));
#37384=CARTESIAN_POINT('Ctrl Pts',(-9.70137854017372,-61.7045179709986,
1.72473670360602E-11));
#37385=CARTESIAN_POINT('Ctrl Pts',(-7.27603390512298,-61.5295179709986,
4.20082013377246));
#37386=CARTESIAN_POINT('Ctrl Pts',(-4.85068927007211,-61.3545179709986,
8.40164026752814));
#37387=CARTESIAN_POINT('Ctrl Pts',(1.48913706160753E-11,-61.1795179709986,
8.40164026751963));
#37388=CARTESIAN_POINT('Ctrl Pts',(4.85068927010141,-61.0045179709986,8.40164026751122));
#37389=CARTESIAN_POINT('Ctrl Pts',(7.27603390513764,-60.8295179709986,4.20082013374708));
#37390=CARTESIAN_POINT('Ctrl Pts',(9.70137854017372,-60.6545179709986,-1.71427802991139E-11));
#37391=CARTESIAN_POINT('Ctrl Pts',(7.27603390512303,-60.4795179709986,-4.20082013377238));
#37392=CARTESIAN_POINT('Ctrl Pts',(4.8506892700722,-60.3045179709986,-8.40164026752809));
#37393=CARTESIAN_POINT('Ctrl Pts',(-1.48007958449808E-11,-60.1295179709986,
-8.40164026751963));
#37394=CARTESIAN_POINT('Ctrl Pts',(-4.8506892701018,-59.9545179709986,-8.401640267511));
#37395=CARTESIAN_POINT('Ctrl Pts',(-7.27603390513759,-59.7795179709986,
-4.20082013374716));
#37396=CARTESIAN_POINT('Ctrl Pts',(-9.70137854017372,-59.6045179709986,
1.70381935621676E-11));
#37397=CARTESIAN_POINT('Ctrl Pts',(-7.27603390512284,-59.4295179709986,
4.20082013377272));
#37398=CARTESIAN_POINT('Ctrl Pts',(-4.85068927007229,-59.2545179709986,
8.40164026752804));
#37399=CARTESIAN_POINT('Ctrl Pts',(1.47102210738864E-11,-59.0795179709986,
8.40164026751963));
#37400=CARTESIAN_POINT('Ctrl Pts',(4.85068927010171,-58.9045179709986,8.40164026751105));
#37401=CARTESIAN_POINT('Ctrl Pts',(7.27603390513755,-58.7295179709986,4.20082013374724));
#37402=CARTESIAN_POINT('Ctrl Pts',(9.70137854017372,-58.5545179709986,-1.69336068252212E-11));
#37403=CARTESIAN_POINT('Ctrl Pts',(7.27603390512288,-58.3795179709986,-4.20082013377264));
#37404=CARTESIAN_POINT('Ctrl Pts',(4.85068927007238,-58.2045179709986,-8.40164026752799));
#37405=CARTESIAN_POINT('Ctrl Pts',(-1.46196463027919E-11,-58.0295179709986,
-8.40164026751963));
#37406=CARTESIAN_POINT('Ctrl Pts',(-4.85068927010162,-57.8545179709986,
-8.40164026751111));
#37407=CARTESIAN_POINT('Ctrl Pts',(-7.27603390513774,-57.6795179709986,
-4.2008201337469));
#37408=CARTESIAN_POINT('Ctrl Pts',(-9.70137854017372,-57.5045179709986,
1.68290200882749E-11));
#37409=CARTESIAN_POINT('Ctrl Pts',(-7.27603390512293,-57.3295179709986,
4.20082013377256));
#37410=CARTESIAN_POINT('Ctrl Pts',(-4.85068927007199,-57.1545179709986,
8.40164026752821));
#37411=CARTESIAN_POINT('Ctrl Pts',(1.45290715316974E-11,-56.9795179709986,
8.40164026751963));
#37412=CARTESIAN_POINT('Ctrl Pts',(4.85068927010153,-56.8045179709986,8.40164026751116));
#37413=CARTESIAN_POINT('Ctrl Pts',(7.2760339051377,-56.6295179709986,4.20082013374698));
#37414=CARTESIAN_POINT('Ctrl Pts',(9.70137854017372,-56.4545179709986,-1.67244333513285E-11));
#37415=CARTESIAN_POINT('Ctrl Pts',(7.27603390512297,-56.2795179709986,-4.20082013377248));
#37416=CARTESIAN_POINT('Ctrl Pts',(4.85068927007208,-56.1045179709986,-8.40164026752816));
#37417=CARTESIAN_POINT('Ctrl Pts',(-1.49160747174474E-11,-55.9295179709986,
-8.40164026751963));
#37418=CARTESIAN_POINT('Ctrl Pts',(-4.85068927010144,-55.7545179709987,
-8.40164026751121));
#37419=CARTESIAN_POINT('Ctrl Pts',(-7.27603390513765,-55.5795179709986,
-4.20082013374706));
#37420=CARTESIAN_POINT('Ctrl Pts',(-9.70137854017372,-55.4045179709986,
1.71713061382685E-11));
#37421=CARTESIAN_POINT('Ctrl Pts',(-7.27603390512302,-55.2295179709986,
4.2008201337724));
#37422=CARTESIAN_POINT('Ctrl Pts',(-4.85068927007218,-55.0545179709986,
8.40164026752811));
#37423=CARTESIAN_POINT('Ctrl Pts',(1.4825499946353E-11,-54.8795179709986,
8.40164026751963));
#37424=CARTESIAN_POINT('Ctrl Pts',(4.85068927010135,-54.7045179709987,8.40164026751126));
#37425=CARTESIAN_POINT('Ctrl Pts',(7.27603390513761,-54.5295179709986,4.20082013374714));
#37426=CARTESIAN_POINT('Ctrl Pts',(9.70137854017372,-54.3545179709986,-1.70667194013222E-11));
#37427=CARTESIAN_POINT('Ctrl Pts',(7.27603390512282,-54.1795179709986,-4.20082013377274));
#37428=CARTESIAN_POINT('Ctrl Pts',(4.85068927007227,-54.0045179709986,-8.40164026752806));
#37429=CARTESIAN_POINT('Ctrl Pts',(-1.47349251752585E-11,-53.8295179709986,
-8.40164026751963));
#37430=CARTESIAN_POINT('Ctrl Pts',(-4.85068927010174,-53.6545179709986,
-8.40164026751104));
#37431=CARTESIAN_POINT('Ctrl Pts',(-7.27603390513756,-53.4795179709987,
-4.20082013374722));
#37432=CARTESIAN_POINT('Ctrl Pts',(-9.70137854017372,-53.3045179709987,
1.69621326643758E-11));
#37433=CARTESIAN_POINT('Ctrl Pts',(-7.27603390512287,-53.1295179709986,
4.20082013377266));
#37434=CARTESIAN_POINT('Ctrl Pts',(-4.85068927007236,-52.9545179709987,
8.401640267528));
#37435=CARTESIAN_POINT('Ctrl Pts',(1.46443504041641E-11,-52.7795179709986,
8.40164026751963));
#37436=CARTESIAN_POINT('Ctrl Pts',(4.85068927010165,-52.6045179709986,8.40164026751109));
#37437=CARTESIAN_POINT('Ctrl Pts',(7.27603390513752,-52.4295179709987,4.2008201337473));
#37438=CARTESIAN_POINT('Ctrl Pts',(9.70137854017372,-52.2545179709986,-1.68575459274295E-11));
#37439=CARTESIAN_POINT('Ctrl Pts',(7.27603390512292,-52.0795179709986,-4.20082013377258));
#37440=CARTESIAN_POINT('Ctrl Pts',(4.85068927007197,-51.9045179709987,-8.40164026752823));
#37441=CARTESIAN_POINT('Ctrl Pts',(-1.45537756330696E-11,-51.7295179709986,
-8.40164026751963));
#37442=CARTESIAN_POINT('Ctrl Pts',(-4.85068927010155,-51.5545179709986,
-8.40164026751114));
#37443=CARTESIAN_POINT('Ctrl Pts',(-7.27603390513771,-51.3795179709987,
-4.20082013374696));
#37444=CARTESIAN_POINT('Ctrl Pts',(-9.70137854017372,-51.2045179709986,
1.67529591904832E-11));
#37445=CARTESIAN_POINT('Ctrl Pts',(-7.27603390512296,-51.0295179709986,
4.2008201337725));
#37446=CARTESIAN_POINT('Ctrl Pts',(-4.85068927007206,-50.8545179709987,
8.40164026752817));
#37447=CARTESIAN_POINT('Ctrl Pts',(1.44632008619752E-11,-50.6795179709987,
8.40164026751963));
#37448=CARTESIAN_POINT('Ctrl Pts',(4.85068927010146,-50.5045179709986,8.4016402675112));
#37449=CARTESIAN_POINT('Ctrl Pts',(7.27603390513766,-50.3295179709987,4.20082013374704));
#37450=CARTESIAN_POINT('Ctrl Pts',(9.70137854017372,-50.1545179709987,-1.71998319774232E-11));
#37451=CARTESIAN_POINT('Ctrl Pts',(7.27603390512301,-49.9795179709986,-4.20082013377243));
#37452=CARTESIAN_POINT('Ctrl Pts',(4.85068927007215,-49.8045179709986,-8.40164026752812));
#37453=CARTESIAN_POINT('Ctrl Pts',(-1.48502040477252E-11,-49.6295179709987,
-8.40164026751963));
#37454=CARTESIAN_POINT('Ctrl Pts',(-4.85068927010137,-49.4545179709986,
-8.40164026751125));
#37455=CARTESIAN_POINT('Ctrl Pts',(-7.27603390513762,-49.2795179709986,
-4.20082013374712));
#37456=CARTESIAN_POINT('Ctrl Pts',(-9.70137854017372,-49.1045179709987,
1.70952452404768E-11));
#37457=CARTESIAN_POINT('Ctrl Pts',(-7.27603390512305,-48.9295179709987,
4.20082013377235));
#37458=CARTESIAN_POINT('Ctrl Pts',(-4.85068927007224,-48.7545179709986,
8.40164026752807));
#37459=CARTESIAN_POINT('Ctrl Pts',(1.47596292766307E-11,-48.5795179709987,
8.40164026751963));
#37460=CARTESIAN_POINT('Ctrl Pts',(4.85068927010176,-48.4045179709987,8.40164026751102));
#37461=CARTESIAN_POINT('Ctrl Pts',(7.27603390513757,-48.2295179709986,4.2008201337472));
#37462=CARTESIAN_POINT('Ctrl Pts',(9.70137854017372,-48.0545179709987,-1.69906585035305E-11));
#37463=CARTESIAN_POINT('Ctrl Pts',(7.27603390512286,-47.8795179709987,-4.20082013377268));
#37464=CARTESIAN_POINT('Ctrl Pts',(5.65116042235429,-47.7622757220518,-7.015183561788));
#37465=CARTESIAN_POINT('Ctrl Pts',(2.55537495509676,-47.63,-8.00360031633711));
#37466=CARTESIAN_POINT('Ctrl Pts',(-5.67113674141202,-212.63,6.1988520909128));
#37467=CARTESIAN_POINT('Ctrl Pts',(-5.09309959239855,-212.63,6.65024148625226));
#37468=CARTESIAN_POINT('Ctrl Pts',(-4.1369669254735,-212.630000000009,7.33153862293111));
#37469=CARTESIAN_POINT('Ctrl Pts',(-1.84049420638942,-212.630000000009,
8.10711214912164));
#37470=CARTESIAN_POINT('Ctrl Pts',(-0.84190354263217,-212.63,8.26396636048523));
#37471=CARTESIAN_POINT('Ctrl Pts',(1.15691725446766,-212.63,8.22412665653735));
#37472=CARTESIAN_POINT('Ctrl Pts',(2.13751792446255,-212.63,8.03230830225828));
#37473=CARTESIAN_POINT('Ctrl Pts',(4.40951680002617,-212.63,7.1736078615634));
#37474=CARTESIAN_POINT('Ctrl Pts',(5.3486773581226,-212.63,6.44726429217888));
#37475=CARTESIAN_POINT('Ctrl Pts',(5.91264939824166,-212.63,5.96893091585754));
#37476=CARTESIAN_POINT('Ctrl Pts',(-1.51301075899711E-11,-213.429517970998,
-8.40164026751963));
#37477=CARTESIAN_POINT('Ctrl Pts',(-4.85068927010199,-213.254517970998,
-8.4016402675109));
#37478=CARTESIAN_POINT('Ctrl Pts',(-7.27603390513785,-213.079517970998,
-4.20082013374671));
#37479=CARTESIAN_POINT('Ctrl Pts',(-9.70137854017372,-212.904517970998,
1.74701493417668E-11));
#37480=CARTESIAN_POINT('Ctrl Pts',(-7.27603390512272,-212.729517970998,
4.20082013377292));
#37481=CARTESIAN_POINT('Ctrl Pts',(-4.85068927007173,-212.554517970998,
8.40164026752836));
#37482=CARTESIAN_POINT('Ctrl Pts',(1.5129078685785E-11,-212.379517970998,
8.40164026751963));
#37483=CARTESIAN_POINT('Ctrl Pts',(4.85068927010198,-212.204517970998,8.4016402675109));
#37484=CARTESIAN_POINT('Ctrl Pts',(7.27603390513785,-212.029517970998,4.20082013374672));
#37485=CARTESIAN_POINT('Ctrl Pts',(9.70137854017372,-211.854517970998,-1.74689612655491E-11));
#37486=CARTESIAN_POINT('Ctrl Pts',(7.27603390512273,-211.679517970998,-4.20082013377291));
#37487=CARTESIAN_POINT('Ctrl Pts',(4.85068927007173,-211.504517970998,-8.40164026752836));
#37488=CARTESIAN_POINT('Ctrl Pts',(-1.51301075899711E-11,-211.329517970998,
-8.40164026751963));
#37489=CARTESIAN_POINT('Ctrl Pts',(-4.85068927010199,-211.154517970998,
-8.4016402675109));
#37490=CARTESIAN_POINT('Ctrl Pts',(-7.27603390513785,-210.979517970998,
-4.20082013374671));
#37491=CARTESIAN_POINT('Ctrl Pts',(-9.70137854017372,-210.804517970998,
1.74701493417668E-11));
#37492=CARTESIAN_POINT('Ctrl Pts',(-7.27603390512272,-210.629517970998,
4.20082013377292));
#37493=CARTESIAN_POINT('Ctrl Pts',(-4.85068927007173,-210.454517970998,
8.40164026752836));
#37494=CARTESIAN_POINT('Ctrl Pts',(1.5129078685785E-11,-210.279517970998,
8.40164026751963));
#37495=CARTESIAN_POINT('Ctrl Pts',(4.85068927010198,-210.104517970998,8.4016402675109));
#37496=CARTESIAN_POINT('Ctrl Pts',(7.27603390513785,-209.929517970998,4.20082013374672));
#37497=CARTESIAN_POINT('Ctrl Pts',(9.70137854017372,-209.754517970998,-1.74689612655491E-11));
#37498=CARTESIAN_POINT('Ctrl Pts',(7.27603390512273,-209.579517970998,-4.20082013377291));
#37499=CARTESIAN_POINT('Ctrl Pts',(4.85068927007173,-209.404517970998,-8.40164026752836));
#37500=CARTESIAN_POINT('Ctrl Pts',(-1.51301075899711E-11,-209.229517970998,
-8.40164026751963));
#37501=CARTESIAN_POINT('Ctrl Pts',(-4.85068927010199,-209.054517970998,
-8.4016402675109));
#37502=CARTESIAN_POINT('Ctrl Pts',(-7.27603390513785,-208.879517970998,
-4.20082013374671));
#37503=CARTESIAN_POINT('Ctrl Pts',(-9.70137854017372,-208.704517970998,
1.74701493417668E-11));
#37504=CARTESIAN_POINT('Ctrl Pts',(-7.27603390512272,-208.529517970998,
4.20082013377292));
#37505=CARTESIAN_POINT('Ctrl Pts',(-4.85068927007173,-208.354517970998,
8.40164026752836));
#37506=CARTESIAN_POINT('Ctrl Pts',(1.5129078685785E-11,-208.179517970998,
8.40164026751963));
#37507=CARTESIAN_POINT('Ctrl Pts',(4.85068927010198,-208.004517970998,8.4016402675109));
#37508=CARTESIAN_POINT('Ctrl Pts',(7.27603390513785,-207.829517970998,4.20082013374672));
#37509=CARTESIAN_POINT('Ctrl Pts',(9.70137854017372,-207.654517970998,-1.74689612655491E-11));
#37510=CARTESIAN_POINT('Ctrl Pts',(7.27603390512273,-207.479517970998,-4.20082013377291));
#37511=CARTESIAN_POINT('Ctrl Pts',(4.85068927007173,-207.304517970998,-8.40164026752836));
#37512=CARTESIAN_POINT('Ctrl Pts',(-1.51301075899711E-11,-207.129517970998,
-8.40164026751963));
#37513=CARTESIAN_POINT('Ctrl Pts',(-4.85068927010199,-206.954517970998,
-8.4016402675109));
#37514=CARTESIAN_POINT('Ctrl Pts',(-7.27603390513785,-206.779517970998,
-4.20082013374671));
#37515=CARTESIAN_POINT('Ctrl Pts',(-9.70137854017372,-206.604517970998,
1.74701493417668E-11));
#37516=CARTESIAN_POINT('Ctrl Pts',(-7.27603390512272,-206.429517970998,
4.20082013377292));
#37517=CARTESIAN_POINT('Ctrl Pts',(-4.85068927007173,-206.254517970998,
8.40164026752836));
#37518=CARTESIAN_POINT('Ctrl Pts',(1.5129078685785E-11,-206.079517970998,
8.40164026751963));
#37519=CARTESIAN_POINT('Ctrl Pts',(4.85068927010198,-205.904517970998,8.4016402675109));
#37520=CARTESIAN_POINT('Ctrl Pts',(7.27603390513785,-205.729517970998,4.20082013374672));
#37521=CARTESIAN_POINT('Ctrl Pts',(9.70137854017372,-205.554517970998,-1.74689612655491E-11));
#37522=CARTESIAN_POINT('Ctrl Pts',(7.27603390512273,-205.379517970998,-4.20082013377291));
#37523=CARTESIAN_POINT('Ctrl Pts',(4.85068927007173,-205.204517970998,-8.40164026752836));
#37524=CARTESIAN_POINT('Ctrl Pts',(-1.51301075899711E-11,-205.029517970998,
-8.40164026751963));
#37525=CARTESIAN_POINT('Ctrl Pts',(-4.85068927010199,-204.854517970998,
-8.4016402675109));
#37526=CARTESIAN_POINT('Ctrl Pts',(-7.27603390513785,-204.679517970998,
-4.20082013374671));
#37527=CARTESIAN_POINT('Ctrl Pts',(-9.70137854017372,-204.504517970998,
1.74701493417668E-11));
#37528=CARTESIAN_POINT('Ctrl Pts',(-7.27603390512272,-204.329517970998,
4.20082013377292));
#37529=CARTESIAN_POINT('Ctrl Pts',(-4.85068927007173,-204.154517970998,
8.40164026752836));
#37530=CARTESIAN_POINT('Ctrl Pts',(1.5129078685785E-11,-203.979517970998,
8.40164026751963));
#37531=CARTESIAN_POINT('Ctrl Pts',(4.85068927010198,-203.804517970998,8.4016402675109));
#37532=CARTESIAN_POINT('Ctrl Pts',(7.27603390513785,-203.629517970998,4.20082013374672));
#37533=CARTESIAN_POINT('Ctrl Pts',(9.70137854017372,-203.454517970998,-1.74689612655491E-11));
#37534=CARTESIAN_POINT('Ctrl Pts',(7.27603390512273,-203.279517970998,-4.20082013377291));
#37535=CARTESIAN_POINT('Ctrl Pts',(4.85068927007173,-203.104517970998,-8.40164026752836));
#37536=CARTESIAN_POINT('Ctrl Pts',(-1.51301075899711E-11,-202.929517970998,
-8.40164026751963));
#37537=CARTESIAN_POINT('Ctrl Pts',(-4.85068927010199,-202.754517970998,
-8.4016402675109));
#37538=CARTESIAN_POINT('Ctrl Pts',(-7.27603390513785,-202.579517970998,
-4.20082013374671));
#37539=CARTESIAN_POINT('Ctrl Pts',(-9.70137854017372,-202.404517970998,
1.74701493417668E-11));
#37540=CARTESIAN_POINT('Ctrl Pts',(-7.27603390512272,-202.229517970998,
4.20082013377292));
#37541=CARTESIAN_POINT('Ctrl Pts',(-4.85068927007173,-202.054517970998,
8.40164026752836));
#37542=CARTESIAN_POINT('Ctrl Pts',(1.5129078685785E-11,-201.879517970998,
8.40164026751963));
#37543=CARTESIAN_POINT('Ctrl Pts',(4.85068927010198,-201.704517970998,8.4016402675109));
#37544=CARTESIAN_POINT('Ctrl Pts',(7.27603390513785,-201.529517970998,4.20082013374672));
#37545=CARTESIAN_POINT('Ctrl Pts',(9.70137854017372,-201.354517970998,-1.74689612655491E-11));
#37546=CARTESIAN_POINT('Ctrl Pts',(7.27603390512273,-201.179517970998,-4.20082013377291));
#37547=CARTESIAN_POINT('Ctrl Pts',(4.85068927007173,-201.004517970998,-8.40164026752836));
#37548=CARTESIAN_POINT('Ctrl Pts',(-1.51301075899711E-11,-200.829517970998,
-8.40164026751963));
#37549=CARTESIAN_POINT('Ctrl Pts',(-4.85068927010199,-200.654517970998,
-8.4016402675109));
#37550=CARTESIAN_POINT('Ctrl Pts',(-7.27603390513785,-200.479517970998,
-4.20082013374671));
#37551=CARTESIAN_POINT('Ctrl Pts',(-9.70137854017372,-200.304517970998,
1.74701493417668E-11));
#37552=CARTESIAN_POINT('Ctrl Pts',(-7.27603390512272,-200.129517970998,
4.20082013377292));
#37553=CARTESIAN_POINT('Ctrl Pts',(-4.85068927007173,-199.954517970998,
8.40164026752836));
#37554=CARTESIAN_POINT('Ctrl Pts',(1.5129078685785E-11,-199.779517970998,
8.40164026751963));
#37555=CARTESIAN_POINT('Ctrl Pts',(4.85068927010198,-199.604517970998,8.4016402675109));
#37556=CARTESIAN_POINT('Ctrl Pts',(7.27603390513785,-199.429517970998,4.20082013374672));
#37557=CARTESIAN_POINT('Ctrl Pts',(9.70137854017372,-199.254517970998,-1.74689612655491E-11));
#37558=CARTESIAN_POINT('Ctrl Pts',(7.27603390512273,-199.079517970998,-4.20082013377291));
#37559=CARTESIAN_POINT('Ctrl Pts',(4.85068927007173,-198.904517970998,-8.40164026752836));
#37560=CARTESIAN_POINT('Ctrl Pts',(-1.51301075899711E-11,-198.729517970998,
-8.40164026751963));
#37561=CARTESIAN_POINT('Ctrl Pts',(-4.85068927010199,-198.554517970998,
-8.4016402675109));
#37562=CARTESIAN_POINT('Ctrl Pts',(-7.27603390513785,-198.379517970998,
-4.20082013374671));
#37563=CARTESIAN_POINT('Ctrl Pts',(-9.70137854017372,-198.204517970998,
1.74701493417668E-11));
#37564=CARTESIAN_POINT('Ctrl Pts',(-7.27603390512272,-198.029517970998,
4.20082013377292));
#37565=CARTESIAN_POINT('Ctrl Pts',(-4.85068927007173,-197.854517970998,
8.40164026752836));
#37566=CARTESIAN_POINT('Ctrl Pts',(1.5129078685785E-11,-197.679517970998,
8.40164026751963));
#37567=CARTESIAN_POINT('Ctrl Pts',(4.85068927010198,-197.504517970998,8.4016402675109));
#37568=CARTESIAN_POINT('Ctrl Pts',(7.27603390513785,-197.329517970998,4.20082013374672));
#37569=CARTESIAN_POINT('Ctrl Pts',(9.70137854017372,-197.154517970998,-1.74689612655491E-11));
#37570=CARTESIAN_POINT('Ctrl Pts',(7.27603390512273,-196.979517970998,-4.20082013377291));
#37571=CARTESIAN_POINT('Ctrl Pts',(4.85068927007173,-196.804517970998,-8.40164026752836));
#37572=CARTESIAN_POINT('Ctrl Pts',(-1.51301075899711E-11,-196.629517970998,
-8.40164026751963));
#37573=CARTESIAN_POINT('Ctrl Pts',(-4.85068927010199,-196.454517970998,
-8.4016402675109));
#37574=CARTESIAN_POINT('Ctrl Pts',(-7.27603390513785,-196.279517970998,
-4.20082013374671));
#37575=CARTESIAN_POINT('Ctrl Pts',(-9.70137854017372,-196.104517970998,
1.74701493417668E-11));
#37576=CARTESIAN_POINT('Ctrl Pts',(-7.27603390512272,-195.929517970998,
4.20082013377292));
#37577=CARTESIAN_POINT('Ctrl Pts',(-4.85068927007173,-195.754517970998,
8.40164026752836));
#37578=CARTESIAN_POINT('Ctrl Pts',(1.5129078685785E-11,-195.579517970998,
8.40164026751963));
#37579=CARTESIAN_POINT('Ctrl Pts',(4.85068927010198,-195.404517970998,8.4016402675109));
#37580=CARTESIAN_POINT('Ctrl Pts',(7.27603390513785,-195.229517970998,4.20082013374672));
#37581=CARTESIAN_POINT('Ctrl Pts',(9.70137854017372,-195.054517970998,-1.74689612655491E-11));
#37582=CARTESIAN_POINT('Ctrl Pts',(7.27603390512273,-194.879517970998,-4.20082013377291));
#37583=CARTESIAN_POINT('Ctrl Pts',(4.85068927007173,-194.704517970998,-8.40164026752836));
#37584=CARTESIAN_POINT('Ctrl Pts',(-1.51301075899711E-11,-194.529517970998,
-8.40164026751963));
#37585=CARTESIAN_POINT('Ctrl Pts',(-4.85068927010199,-194.354517970998,
-8.4016402675109));
#37586=CARTESIAN_POINT('Ctrl Pts',(-7.27603390513785,-194.179517970998,
-4.20082013374671));
#37587=CARTESIAN_POINT('Ctrl Pts',(-9.70137854017372,-194.004517970998,
1.74701493417668E-11));
#37588=CARTESIAN_POINT('Ctrl Pts',(-7.27603390512272,-193.829517970998,
4.20082013377292));
#37589=CARTESIAN_POINT('Ctrl Pts',(-4.85068927007173,-193.654517970998,
8.40164026752836));
#37590=CARTESIAN_POINT('Ctrl Pts',(1.5129078685785E-11,-193.479517970998,
8.40164026751963));
#37591=CARTESIAN_POINT('Ctrl Pts',(4.85068927010198,-193.304517970998,8.4016402675109));
#37592=CARTESIAN_POINT('Ctrl Pts',(7.27603390513785,-193.129517970998,4.20082013374672));
#37593=CARTESIAN_POINT('Ctrl Pts',(9.70137854017372,-192.954517970998,-1.74689612655491E-11));
#37594=CARTESIAN_POINT('Ctrl Pts',(7.27603390512273,-192.779517970998,-4.20082013377291));
#37595=CARTESIAN_POINT('Ctrl Pts',(4.85068927007173,-192.604517970998,-8.40164026752836));
#37596=CARTESIAN_POINT('Ctrl Pts',(-1.51301075899711E-11,-192.429517970998,
-8.40164026751963));
#37597=CARTESIAN_POINT('Ctrl Pts',(-4.85068927010199,-192.254517970998,
-8.4016402675109));
#37598=CARTESIAN_POINT('Ctrl Pts',(-7.27603390513785,-192.079517970998,
-4.20082013374671));
#37599=CARTESIAN_POINT('Ctrl Pts',(-9.70137854017372,-191.904517970998,
1.74701493417668E-11));
#37600=CARTESIAN_POINT('Ctrl Pts',(-7.27603390512272,-191.729517970998,
4.20082013377292));
#37601=CARTESIAN_POINT('Ctrl Pts',(-4.85068927007173,-191.554517970998,
8.40164026752836));
#37602=CARTESIAN_POINT('Ctrl Pts',(1.5129078685785E-11,-191.379517970998,
8.40164026751963));
#37603=CARTESIAN_POINT('Ctrl Pts',(4.85068927010198,-191.204517970998,8.4016402675109));
#37604=CARTESIAN_POINT('Ctrl Pts',(7.27603390513785,-191.029517970998,4.20082013374672));
#37605=CARTESIAN_POINT('Ctrl Pts',(9.70137854017372,-190.854517970998,-1.74689612655491E-11));
#37606=CARTESIAN_POINT('Ctrl Pts',(7.27603390512273,-190.679517970998,-4.20082013377291));
#37607=CARTESIAN_POINT('Ctrl Pts',(4.85068927007173,-190.504517970998,-8.40164026752836));
#37608=CARTESIAN_POINT('Ctrl Pts',(-1.51301075899711E-11,-190.329517970998,
-8.40164026751963));
#37609=CARTESIAN_POINT('Ctrl Pts',(-4.85068927010199,-190.154517970998,
-8.4016402675109));
#37610=CARTESIAN_POINT('Ctrl Pts',(-7.27603390513785,-189.979517970998,
-4.20082013374671));
#37611=CARTESIAN_POINT('Ctrl Pts',(-9.70137854017372,-189.804517970998,
1.74701493417668E-11));
#37612=CARTESIAN_POINT('Ctrl Pts',(-7.27603390512272,-189.629517970998,
4.20082013377292));
#37613=CARTESIAN_POINT('Ctrl Pts',(-4.85068927007173,-189.454517970998,
8.40164026752836));
#37614=CARTESIAN_POINT('Ctrl Pts',(1.5129078685785E-11,-189.279517970998,
8.40164026751963));
#37615=CARTESIAN_POINT('Ctrl Pts',(4.85068927010198,-189.104517970998,8.4016402675109));
#37616=CARTESIAN_POINT('Ctrl Pts',(7.27603390513785,-188.929517970998,4.20082013374672));
#37617=CARTESIAN_POINT('Ctrl Pts',(9.70137854017372,-188.754517970998,-1.74689612655491E-11));
#37618=CARTESIAN_POINT('Ctrl Pts',(7.27603390512273,-188.579517970998,-4.20082013377291));
#37619=CARTESIAN_POINT('Ctrl Pts',(4.85068927007173,-188.404517970998,-8.40164026752836));
#37620=CARTESIAN_POINT('Ctrl Pts',(-1.51301075899711E-11,-188.229517970998,
-8.40164026751963));
#37621=CARTESIAN_POINT('Ctrl Pts',(-4.85068927010199,-188.054517970998,
-8.4016402675109));
#37622=CARTESIAN_POINT('Ctrl Pts',(-7.27603390513785,-187.879517970998,
-4.20082013374671));
#37623=CARTESIAN_POINT('Ctrl Pts',(-9.70137854017372,-187.704517970998,
1.74701493417668E-11));
#37624=CARTESIAN_POINT('Ctrl Pts',(-7.27603390512272,-187.529517970998,
4.20082013377292));
#37625=CARTESIAN_POINT('Ctrl Pts',(-4.85068927007173,-187.354517970998,
8.40164026752836));
#37626=CARTESIAN_POINT('Ctrl Pts',(1.5129078685785E-11,-187.179517970998,
8.40164026751963));
#37627=CARTESIAN_POINT('Ctrl Pts',(4.85068927010198,-187.004517970998,8.4016402675109));
#37628=CARTESIAN_POINT('Ctrl Pts',(7.27603390513785,-186.829517970998,4.20082013374672));
#37629=CARTESIAN_POINT('Ctrl Pts',(9.70137854017372,-186.654517970998,-1.74689612655491E-11));
#37630=CARTESIAN_POINT('Ctrl Pts',(7.27603390512273,-186.479517970998,-4.20082013377291));
#37631=CARTESIAN_POINT('Ctrl Pts',(4.85068927007173,-186.304517970998,-8.40164026752836));
#37632=CARTESIAN_POINT('Ctrl Pts',(-1.51301075899711E-11,-186.129517970998,
-8.40164026751963));
#37633=CARTESIAN_POINT('Ctrl Pts',(-4.85068927010199,-185.954517970998,
-8.4016402675109));
#37634=CARTESIAN_POINT('Ctrl Pts',(-7.27603390513785,-185.779517970998,
-4.20082013374671));
#37635=CARTESIAN_POINT('Ctrl Pts',(-9.70137854017372,-185.604517970998,
1.74701493417668E-11));
#37636=CARTESIAN_POINT('Ctrl Pts',(-7.27603390512272,-185.429517970998,
4.20082013377292));
#37637=CARTESIAN_POINT('Ctrl Pts',(-4.85068927007173,-185.254517970998,
8.40164026752836));
#37638=CARTESIAN_POINT('Ctrl Pts',(1.5129078685785E-11,-185.079517970998,
8.40164026751963));
#37639=CARTESIAN_POINT('Ctrl Pts',(4.85068927010198,-184.904517970998,8.4016402675109));
#37640=CARTESIAN_POINT('Ctrl Pts',(7.27603390513785,-184.729517970998,4.20082013374672));
#37641=CARTESIAN_POINT('Ctrl Pts',(9.70137854017372,-184.554517970998,-1.74689612655491E-11));
#37642=CARTESIAN_POINT('Ctrl Pts',(7.27603390512273,-184.379517970998,-4.20082013377291));
#37643=CARTESIAN_POINT('Ctrl Pts',(4.85068927007173,-184.204517970998,-8.40164026752836));
#37644=CARTESIAN_POINT('Ctrl Pts',(-1.51301075899711E-11,-184.029517970998,
-8.40164026751963));
#37645=CARTESIAN_POINT('Ctrl Pts',(-4.85068927010199,-183.854517970998,
-8.4016402675109));
#37646=CARTESIAN_POINT('Ctrl Pts',(-7.27603390513785,-183.679517970998,
-4.20082013374671));
#37647=CARTESIAN_POINT('Ctrl Pts',(-9.70137854017372,-183.504517970998,
1.74701493417668E-11));
#37648=CARTESIAN_POINT('Ctrl Pts',(-7.27603390512272,-183.329517970998,
4.20082013377292));
#37649=CARTESIAN_POINT('Ctrl Pts',(-4.85068927007173,-183.154517970998,
8.40164026752836));
#37650=CARTESIAN_POINT('Ctrl Pts',(1.5129078685785E-11,-182.979517970998,
8.40164026751963));
#37651=CARTESIAN_POINT('Ctrl Pts',(4.85068927010198,-182.804517970998,8.4016402675109));
#37652=CARTESIAN_POINT('Ctrl Pts',(7.27603390513785,-182.629517970998,4.20082013374672));
#37653=CARTESIAN_POINT('Ctrl Pts',(9.70137854017372,-182.454517970998,-1.74689612655491E-11));
#37654=CARTESIAN_POINT('Ctrl Pts',(7.27603390512273,-182.279517970998,-4.20082013377291));
#37655=CARTESIAN_POINT('Ctrl Pts',(4.85068927007173,-182.104517970998,-8.40164026752836));
#37656=CARTESIAN_POINT('Ctrl Pts',(-1.51301075899711E-11,-181.929517970998,
-8.40164026751963));
#37657=CARTESIAN_POINT('Ctrl Pts',(-4.85068927010199,-181.754517970998,
-8.4016402675109));
#37658=CARTESIAN_POINT('Ctrl Pts',(-7.27603390513785,-181.579517970998,
-4.20082013374671));
#37659=CARTESIAN_POINT('Ctrl Pts',(-9.70137854017372,-181.404517970998,
1.74701493417668E-11));
#37660=CARTESIAN_POINT('Ctrl Pts',(-7.27603390512272,-181.229517970998,
4.20082013377292));
#37661=CARTESIAN_POINT('Ctrl Pts',(-4.85068927007173,-181.054517970998,
8.40164026752836));
#37662=CARTESIAN_POINT('Ctrl Pts',(1.5129078685785E-11,-180.879517970998,
8.40164026751963));
#37663=CARTESIAN_POINT('Ctrl Pts',(4.85068927010198,-180.704517970998,8.4016402675109));
#37664=CARTESIAN_POINT('Ctrl Pts',(7.27603390513785,-180.529517970998,4.20082013374672));
#37665=CARTESIAN_POINT('Ctrl Pts',(9.70137854017372,-180.354517970998,-1.74689612655491E-11));
#37666=CARTESIAN_POINT('Ctrl Pts',(7.27603390512273,-180.179517970998,-4.20082013377291));
#37667=CARTESIAN_POINT('Ctrl Pts',(4.85068927007173,-180.004517970998,-8.40164026752836));
#37668=CARTESIAN_POINT('Ctrl Pts',(-1.51301075899711E-11,-179.829517970998,
-8.40164026751963));
#37669=CARTESIAN_POINT('Ctrl Pts',(-4.85068927010199,-179.654517970998,
-8.4016402675109));
#37670=CARTESIAN_POINT('Ctrl Pts',(-7.27603390513785,-179.479517970998,
-4.20082013374671));
#37671=CARTESIAN_POINT('Ctrl Pts',(-9.70137854017372,-179.304517970998,
1.74701493417668E-11));
#37672=CARTESIAN_POINT('Ctrl Pts',(-7.27603390512272,-179.129517970998,
4.20082013377292));
#37673=CARTESIAN_POINT('Ctrl Pts',(-4.85068927007173,-178.954517970998,
8.40164026752836));
#37674=CARTESIAN_POINT('Ctrl Pts',(1.5129078685785E-11,-178.779517970998,
8.40164026751963));
#37675=CARTESIAN_POINT('Ctrl Pts',(4.85068927010198,-178.604517970998,8.4016402675109));
#37676=CARTESIAN_POINT('Ctrl Pts',(7.27603390513785,-178.429517970998,4.20082013374672));
#37677=CARTESIAN_POINT('Ctrl Pts',(9.70137854017372,-178.254517970998,-1.74689612655491E-11));
#37678=CARTESIAN_POINT('Ctrl Pts',(7.27603390512273,-178.079517970998,-4.20082013377291));
#37679=CARTESIAN_POINT('Ctrl Pts',(4.85068927007173,-177.904517970998,-8.40164026752836));
#37680=CARTESIAN_POINT('Ctrl Pts',(-1.51301075899711E-11,-177.729517970998,
-8.40164026751963));
#37681=CARTESIAN_POINT('Ctrl Pts',(-4.85068927010199,-177.554517970998,
-8.4016402675109));
#37682=CARTESIAN_POINT('Ctrl Pts',(-7.27603390513785,-177.379517970998,
-4.20082013374671));
#37683=CARTESIAN_POINT('Ctrl Pts',(-9.70137854017372,-177.204517970998,
1.74701493417668E-11));
#37684=CARTESIAN_POINT('Ctrl Pts',(-7.27603390512272,-177.029517970998,
4.20082013377292));
#37685=CARTESIAN_POINT('Ctrl Pts',(-4.85068927007173,-176.854517970998,
8.40164026752836));
#37686=CARTESIAN_POINT('Ctrl Pts',(1.5129078685785E-11,-176.679517970998,
8.40164026751963));
#37687=CARTESIAN_POINT('Ctrl Pts',(4.85068927010198,-176.504517970998,8.4016402675109));
#37688=CARTESIAN_POINT('Ctrl Pts',(7.27603390513785,-176.329517970998,4.20082013374672));
#37689=CARTESIAN_POINT('Ctrl Pts',(9.70137854017372,-176.154517970998,-1.74689612655491E-11));
#37690=CARTESIAN_POINT('Ctrl Pts',(7.27603390512273,-175.979517970998,-4.20082013377291));
#37691=CARTESIAN_POINT('Ctrl Pts',(4.85068927007173,-175.804517970998,-8.40164026752836));
#37692=CARTESIAN_POINT('Ctrl Pts',(-1.51301075899711E-11,-175.629517970998,
-8.40164026751963));
#37693=CARTESIAN_POINT('Ctrl Pts',(-4.85068927010199,-175.454517970998,
-8.4016402675109));
#37694=CARTESIAN_POINT('Ctrl Pts',(-7.27603390513785,-175.279517970998,
-4.20082013374671));
#37695=CARTESIAN_POINT('Ctrl Pts',(-9.70137854017372,-175.104517970998,
1.74701493417668E-11));
#37696=CARTESIAN_POINT('Ctrl Pts',(-7.27603390512272,-174.929517970998,
4.20082013377292));
#37697=CARTESIAN_POINT('Ctrl Pts',(-4.85068927007173,-174.754517970998,
8.40164026752836));
#37698=CARTESIAN_POINT('Ctrl Pts',(1.5129078685785E-11,-174.579517970998,
8.40164026751963));
#37699=CARTESIAN_POINT('Ctrl Pts',(4.85068927010198,-174.404517970998,8.4016402675109));
#37700=CARTESIAN_POINT('Ctrl Pts',(7.27603390513785,-174.229517970998,4.20082013374672));
#37701=CARTESIAN_POINT('Ctrl Pts',(9.70137854017372,-174.054517970998,-1.74689612655491E-11));
#37702=CARTESIAN_POINT('Ctrl Pts',(7.27603390512273,-173.879517970998,-4.20082013377291));
#37703=CARTESIAN_POINT('Ctrl Pts',(4.85068927007173,-173.704517970998,-8.40164026752836));
#37704=CARTESIAN_POINT('Ctrl Pts',(-1.51301075899711E-11,-173.529517970998,
-8.40164026751963));
#37705=CARTESIAN_POINT('Ctrl Pts',(-4.85068927010199,-173.354517970998,
-8.4016402675109));
#37706=CARTESIAN_POINT('Ctrl Pts',(-7.27603390513785,-173.179517970998,
-4.20082013374671));
#37707=CARTESIAN_POINT('Ctrl Pts',(-9.70137854017372,-173.004517970998,
1.74701493417668E-11));
#37708=CARTESIAN_POINT('Ctrl Pts',(-7.27603390512272,-172.829517970998,
4.20082013377292));
#37709=CARTESIAN_POINT('Ctrl Pts',(-4.85068927007173,-172.654517970998,
8.40164026752836));
#37710=CARTESIAN_POINT('Ctrl Pts',(1.5129078685785E-11,-172.479517970998,
8.40164026751963));
#37711=CARTESIAN_POINT('Ctrl Pts',(4.85068927010198,-172.304517970998,8.4016402675109));
#37712=CARTESIAN_POINT('Ctrl Pts',(7.27603390513785,-172.129517970998,4.20082013374672));
#37713=CARTESIAN_POINT('Ctrl Pts',(9.70137854017372,-171.954517970998,-1.74689612655491E-11));
#37714=CARTESIAN_POINT('Ctrl Pts',(7.27603390512273,-171.779517970998,-4.20082013377291));
#37715=CARTESIAN_POINT('Ctrl Pts',(4.85068927007173,-171.604517970998,-8.40164026752836));
#37716=CARTESIAN_POINT('Ctrl Pts',(-1.51301075899711E-11,-171.429517970998,
-8.40164026751963));
#37717=CARTESIAN_POINT('Ctrl Pts',(-4.85068927010199,-171.254517970998,
-8.4016402675109));
#37718=CARTESIAN_POINT('Ctrl Pts',(-7.27603390513785,-171.079517970998,
-4.20082013374671));
#37719=CARTESIAN_POINT('Ctrl Pts',(-9.70137854017372,-170.904517970998,
1.74701493417668E-11));
#37720=CARTESIAN_POINT('Ctrl Pts',(-7.27603390512272,-170.729517970998,
4.20082013377292));
#37721=CARTESIAN_POINT('Ctrl Pts',(-4.85068927007173,-170.554517970998,
8.40164026752836));
#37722=CARTESIAN_POINT('Ctrl Pts',(1.5129078685785E-11,-170.379517970998,
8.40164026751963));
#37723=CARTESIAN_POINT('Ctrl Pts',(4.85068927010198,-170.204517970998,8.4016402675109));
#37724=CARTESIAN_POINT('Ctrl Pts',(7.27603390513785,-170.029517970998,4.20082013374672));
#37725=CARTESIAN_POINT('Ctrl Pts',(9.70137854017372,-169.854517970998,-1.74689612655491E-11));
#37726=CARTESIAN_POINT('Ctrl Pts',(7.27603390512273,-169.679517970998,-4.20082013377291));
#37727=CARTESIAN_POINT('Ctrl Pts',(4.85068927007173,-169.504517970998,-8.40164026752836));
#37728=CARTESIAN_POINT('Ctrl Pts',(-1.51301075899711E-11,-169.329517970998,
-8.40164026751963));
#37729=CARTESIAN_POINT('Ctrl Pts',(-4.85068927010199,-169.154517970998,
-8.4016402675109));
#37730=CARTESIAN_POINT('Ctrl Pts',(-7.27603390513785,-168.979517970998,
-4.20082013374671));
#37731=CARTESIAN_POINT('Ctrl Pts',(-9.70137854017372,-168.804517970998,
1.74701493417668E-11));
#37732=CARTESIAN_POINT('Ctrl Pts',(-7.27603390512272,-168.629517970998,
4.20082013377292));
#37733=CARTESIAN_POINT('Ctrl Pts',(-4.85068927007173,-168.454517970998,
8.40164026752836));
#37734=CARTESIAN_POINT('Ctrl Pts',(1.5129078685785E-11,-168.279517970998,
8.40164026751963));
#37735=CARTESIAN_POINT('Ctrl Pts',(4.85068927010198,-168.104517970998,8.4016402675109));
#37736=CARTESIAN_POINT('Ctrl Pts',(7.27603390513785,-167.929517970998,4.20082013374672));
#37737=CARTESIAN_POINT('Ctrl Pts',(9.70137854017372,-167.754517970998,-1.74689612655491E-11));
#37738=CARTESIAN_POINT('Ctrl Pts',(7.27603390512273,-167.579517970998,-4.20082013377291));
#37739=CARTESIAN_POINT('Ctrl Pts',(4.85068927007173,-167.404517970998,-8.40164026752836));
#37740=CARTESIAN_POINT('Ctrl Pts',(-1.51301075899711E-11,-167.229517970998,
-8.40164026751963));
#37741=CARTESIAN_POINT('Ctrl Pts',(-4.85068927010199,-167.054517970998,
-8.4016402675109));
#37742=CARTESIAN_POINT('Ctrl Pts',(-7.27603390513785,-166.879517970998,
-4.20082013374671));
#37743=CARTESIAN_POINT('Ctrl Pts',(-9.70137854017372,-166.704517970998,
1.74701493417668E-11));
#37744=CARTESIAN_POINT('Ctrl Pts',(-7.27603390512272,-166.529517970998,
4.20082013377292));
#37745=CARTESIAN_POINT('Ctrl Pts',(-4.85068927007173,-166.354517970998,
8.40164026752836));
#37746=CARTESIAN_POINT('Ctrl Pts',(1.5129078685785E-11,-166.179517970998,
8.40164026751963));
#37747=CARTESIAN_POINT('Ctrl Pts',(4.85068927010198,-166.004517970998,8.4016402675109));
#37748=CARTESIAN_POINT('Ctrl Pts',(7.27603390513785,-165.829517970998,4.20082013374672));
#37749=CARTESIAN_POINT('Ctrl Pts',(9.70137854017372,-165.654517970998,-1.74689612655491E-11));
#37750=CARTESIAN_POINT('Ctrl Pts',(7.27603390512273,-165.479517970998,-4.20082013377291));
#37751=CARTESIAN_POINT('Ctrl Pts',(4.85068927007173,-165.304517970998,-8.40164026752836));
#37752=CARTESIAN_POINT('Ctrl Pts',(-1.51301075899711E-11,-165.129517970998,
-8.40164026751963));
#37753=CARTESIAN_POINT('Ctrl Pts',(-4.85068927010199,-164.954517970998,
-8.4016402675109));
#37754=CARTESIAN_POINT('Ctrl Pts',(-7.27603390513785,-164.779517970998,
-4.20082013374671));
#37755=CARTESIAN_POINT('Ctrl Pts',(-9.70137854017372,-164.604517970998,
1.74701493417668E-11));
#37756=CARTESIAN_POINT('Ctrl Pts',(-7.27603390512272,-164.429517970998,
4.20082013377292));
#37757=CARTESIAN_POINT('Ctrl Pts',(-4.85068927007173,-164.254517970998,
8.40164026752836));
#37758=CARTESIAN_POINT('Ctrl Pts',(1.5129078685785E-11,-164.079517970998,
8.40164026751963));
#37759=CARTESIAN_POINT('Ctrl Pts',(4.85068927010198,-163.904517970998,8.4016402675109));
#37760=CARTESIAN_POINT('Ctrl Pts',(7.27603390513785,-163.729517970998,4.20082013374672));
#37761=CARTESIAN_POINT('Ctrl Pts',(9.70137854017372,-163.554517970998,-1.74689612655491E-11));
#37762=CARTESIAN_POINT('Ctrl Pts',(7.27603390512273,-163.379517970998,-4.20082013377291));
#37763=CARTESIAN_POINT('Ctrl Pts',(4.85068927007173,-163.204517970998,-8.40164026752836));
#37764=CARTESIAN_POINT('Ctrl Pts',(-1.51301075899711E-11,-163.029517970998,
-8.40164026751963));
#37765=CARTESIAN_POINT('Ctrl Pts',(-4.85068927010199,-162.854517970998,
-8.4016402675109));
#37766=CARTESIAN_POINT('Ctrl Pts',(-7.27603390513785,-162.679517970998,
-4.20082013374671));
#37767=CARTESIAN_POINT('Ctrl Pts',(-9.70137854017372,-162.504517970998,
1.74701493417668E-11));
#37768=CARTESIAN_POINT('Ctrl Pts',(-7.27603390512272,-162.329517970998,
4.20082013377292));
#37769=CARTESIAN_POINT('Ctrl Pts',(-4.85068927007173,-162.154517970998,
8.40164026752836));
#37770=CARTESIAN_POINT('Ctrl Pts',(1.5129078685785E-11,-161.979517970998,
8.40164026751963));
#37771=CARTESIAN_POINT('Ctrl Pts',(4.85068927010198,-161.804517970998,8.4016402675109));
#37772=CARTESIAN_POINT('Ctrl Pts',(7.27603390513785,-161.629517970998,4.20082013374672));
#37773=CARTESIAN_POINT('Ctrl Pts',(9.70137854017372,-161.454517970998,-1.74689612655491E-11));
#37774=CARTESIAN_POINT('Ctrl Pts',(7.27603390512273,-161.279517970998,-4.20082013377291));
#37775=CARTESIAN_POINT('Ctrl Pts',(4.85068927007173,-161.104517970998,-8.40164026752836));
#37776=CARTESIAN_POINT('Ctrl Pts',(-1.51301075899711E-11,-160.929517970998,
-8.40164026751963));
#37777=CARTESIAN_POINT('Ctrl Pts',(-4.85068927010199,-160.754517970998,
-8.4016402675109));
#37778=CARTESIAN_POINT('Ctrl Pts',(-7.27603390513785,-160.579517970998,
-4.20082013374671));
#37779=CARTESIAN_POINT('Ctrl Pts',(-9.70137854017372,-160.404517970998,
1.74701493417668E-11));
#37780=CARTESIAN_POINT('Ctrl Pts',(-7.27603390512272,-160.229517970998,
4.20082013377292));
#37781=CARTESIAN_POINT('Ctrl Pts',(-4.85068927007173,-160.054517970998,
8.40164026752836));
#37782=CARTESIAN_POINT('Ctrl Pts',(1.5129078685785E-11,-159.879517970998,
8.40164026751963));
#37783=CARTESIAN_POINT('Ctrl Pts',(4.85068927010198,-159.704517970998,8.4016402675109));
#37784=CARTESIAN_POINT('Ctrl Pts',(7.27603390513785,-159.529517970998,4.20082013374672));
#37785=CARTESIAN_POINT('Ctrl Pts',(9.70137854017372,-159.354517970998,-1.74689612655491E-11));
#37786=CARTESIAN_POINT('Ctrl Pts',(7.27603390512273,-159.179517970998,-4.20082013377291));
#37787=CARTESIAN_POINT('Ctrl Pts',(4.85068927007173,-159.004517970998,-8.40164026752836));
#37788=CARTESIAN_POINT('Ctrl Pts',(-1.51301075899711E-11,-158.829517970998,
-8.40164026751963));
#37789=CARTESIAN_POINT('Ctrl Pts',(-4.85068927010199,-158.654517970998,
-8.4016402675109));
#37790=CARTESIAN_POINT('Ctrl Pts',(-7.27603390513785,-158.479517970998,
-4.20082013374671));
#37791=CARTESIAN_POINT('Ctrl Pts',(-9.70137854017372,-158.304517970998,
1.74701493417668E-11));
#37792=CARTESIAN_POINT('Ctrl Pts',(-7.27603390512272,-158.129517970998,
4.20082013377292));
#37793=CARTESIAN_POINT('Ctrl Pts',(-4.85068927007173,-157.954517970998,
8.40164026752836));
#37794=CARTESIAN_POINT('Ctrl Pts',(1.5129078685785E-11,-157.779517970998,
8.40164026751963));
#37795=CARTESIAN_POINT('Ctrl Pts',(4.85068927010198,-157.604517970998,8.4016402675109));
#37796=CARTESIAN_POINT('Ctrl Pts',(7.27603390513785,-157.429517970998,4.20082013374672));
#37797=CARTESIAN_POINT('Ctrl Pts',(9.70137854017372,-157.254517970998,-1.74689612655491E-11));
#37798=CARTESIAN_POINT('Ctrl Pts',(7.27603390512273,-157.079517970998,-4.20082013377291));
#37799=CARTESIAN_POINT('Ctrl Pts',(4.85068927007173,-156.904517970998,-8.40164026752836));
#37800=CARTESIAN_POINT('Ctrl Pts',(-1.51301075899711E-11,-156.729517970998,
-8.40164026751963));
#37801=CARTESIAN_POINT('Ctrl Pts',(-4.85068927010199,-156.554517970998,
-8.4016402675109));
#37802=CARTESIAN_POINT('Ctrl Pts',(-7.27603390513785,-156.379517970998,
-4.20082013374671));
#37803=CARTESIAN_POINT('Ctrl Pts',(-9.70137854017372,-156.204517970998,
1.74701493417668E-11));
#37804=CARTESIAN_POINT('Ctrl Pts',(-7.27603390512272,-156.029517970998,
4.20082013377292));
#37805=CARTESIAN_POINT('Ctrl Pts',(-4.85068927007173,-155.854517970998,
8.40164026752836));
#37806=CARTESIAN_POINT('Ctrl Pts',(1.5129078685785E-11,-155.679517970998,
8.40164026751963));
#37807=CARTESIAN_POINT('Ctrl Pts',(4.85068927010198,-155.504517970998,8.4016402675109));
#37808=CARTESIAN_POINT('Ctrl Pts',(7.27603390513785,-155.329517970998,4.20082013374672));
#37809=CARTESIAN_POINT('Ctrl Pts',(9.70137854017372,-155.154517970998,-1.74689612655491E-11));
#37810=CARTESIAN_POINT('Ctrl Pts',(7.27603390512273,-154.979517970998,-4.20082013377291));
#37811=CARTESIAN_POINT('Ctrl Pts',(4.85068927007173,-154.804517970998,-8.40164026752836));
#37812=CARTESIAN_POINT('Ctrl Pts',(-1.51301075899711E-11,-154.629517970998,
-8.40164026751963));
#37813=CARTESIAN_POINT('Ctrl Pts',(-4.85068927010199,-154.454517970998,
-8.4016402675109));
#37814=CARTESIAN_POINT('Ctrl Pts',(-7.27603390513785,-154.279517970998,
-4.20082013374671));
#37815=CARTESIAN_POINT('Ctrl Pts',(-9.70137854017372,-154.104517970998,
1.74701493417668E-11));
#37816=CARTESIAN_POINT('Ctrl Pts',(-7.27603390512272,-153.929517970998,
4.20082013377292));
#37817=CARTESIAN_POINT('Ctrl Pts',(-4.85068927007173,-153.754517970998,
8.40164026752836));
#37818=CARTESIAN_POINT('Ctrl Pts',(1.5129078685785E-11,-153.579517970998,
8.40164026751963));
#37819=CARTESIAN_POINT('Ctrl Pts',(4.85068927010198,-153.404517970998,8.4016402675109));
#37820=CARTESIAN_POINT('Ctrl Pts',(7.27603390513785,-153.229517970998,4.20082013374672));
#37821=CARTESIAN_POINT('Ctrl Pts',(9.70137854017372,-153.054517970998,-1.74689612655491E-11));
#37822=CARTESIAN_POINT('Ctrl Pts',(7.27603390512273,-152.879517970998,-4.20082013377291));
#37823=CARTESIAN_POINT('Ctrl Pts',(4.85068927007173,-152.704517970998,-8.40164026752836));
#37824=CARTESIAN_POINT('Ctrl Pts',(-1.51301075899711E-11,-152.529517970998,
-8.40164026751963));
#37825=CARTESIAN_POINT('Ctrl Pts',(-4.85068927010199,-152.354517970998,
-8.4016402675109));
#37826=CARTESIAN_POINT('Ctrl Pts',(-7.27603390513785,-152.179517970998,
-4.20082013374671));
#37827=CARTESIAN_POINT('Ctrl Pts',(-9.70137854017372,-152.004517970998,
1.74701493417668E-11));
#37828=CARTESIAN_POINT('Ctrl Pts',(-7.27603390512272,-151.829517970998,
4.20082013377292));
#37829=CARTESIAN_POINT('Ctrl Pts',(-4.85068927007173,-151.654517970998,
8.40164026752836));
#37830=CARTESIAN_POINT('Ctrl Pts',(1.5129078685785E-11,-151.479517970998,
8.40164026751963));
#37831=CARTESIAN_POINT('Ctrl Pts',(4.85068927010198,-151.304517970998,8.4016402675109));
#37832=CARTESIAN_POINT('Ctrl Pts',(7.27603390513785,-151.129517970998,4.20082013374672));
#37833=CARTESIAN_POINT('Ctrl Pts',(9.70137854017372,-150.954517970998,-1.74689612655491E-11));
#37834=CARTESIAN_POINT('Ctrl Pts',(7.27603390512273,-150.779517970998,-4.20082013377291));
#37835=CARTESIAN_POINT('Ctrl Pts',(4.85068927007173,-150.604517970998,-8.40164026752836));
#37836=CARTESIAN_POINT('Ctrl Pts',(-1.51301075899711E-11,-150.429517970998,
-8.40164026751963));
#37837=CARTESIAN_POINT('Ctrl Pts',(-4.85068927010199,-150.254517970998,
-8.4016402675109));
#37838=CARTESIAN_POINT('Ctrl Pts',(-7.27603390513785,-150.079517970998,
-4.20082013374671));
#37839=CARTESIAN_POINT('Ctrl Pts',(-9.70137854017372,-149.904517970998,
1.74701493417668E-11));
#37840=CARTESIAN_POINT('Ctrl Pts',(-7.27603390512272,-149.729517970998,
4.20082013377292));
#37841=CARTESIAN_POINT('Ctrl Pts',(-4.85068927007173,-149.554517970998,
8.40164026752836));
#37842=CARTESIAN_POINT('Ctrl Pts',(1.5129078685785E-11,-149.379517970998,
8.40164026751963));
#37843=CARTESIAN_POINT('Ctrl Pts',(4.85068927010198,-149.204517970998,8.4016402675109));
#37844=CARTESIAN_POINT('Ctrl Pts',(7.27603390513785,-149.029517970998,4.20082013374672));
#37845=CARTESIAN_POINT('Ctrl Pts',(9.70137854017372,-148.854517970998,-1.74689612655491E-11));
#37846=CARTESIAN_POINT('Ctrl Pts',(7.27603390512273,-148.679517970998,-4.20082013377291));
#37847=CARTESIAN_POINT('Ctrl Pts',(4.85068927007173,-148.504517970998,-8.40164026752836));
#37848=CARTESIAN_POINT('Ctrl Pts',(-1.51301075899711E-11,-148.329517970998,
-8.40164026751963));
#37849=CARTESIAN_POINT('Ctrl Pts',(-4.85068927010199,-148.154517970998,
-8.4016402675109));
#37850=CARTESIAN_POINT('Ctrl Pts',(-7.27603390513785,-147.979517970998,
-4.20082013374671));
#37851=CARTESIAN_POINT('Ctrl Pts',(-9.70137854017372,-147.804517970998,
1.74701493417668E-11));
#37852=CARTESIAN_POINT('Ctrl Pts',(-7.27603390512272,-147.629517970998,
4.20082013377292));
#37853=CARTESIAN_POINT('Ctrl Pts',(-4.85068927007173,-147.454517970998,
8.40164026752836));
#37854=CARTESIAN_POINT('Ctrl Pts',(1.5129078685785E-11,-147.279517970998,
8.40164026751963));
#37855=CARTESIAN_POINT('Ctrl Pts',(4.85068927010198,-147.104517970998,8.4016402675109));
#37856=CARTESIAN_POINT('Ctrl Pts',(7.27603390513785,-146.929517970998,4.20082013374672));
#37857=CARTESIAN_POINT('Ctrl Pts',(9.70137854017372,-146.754517970998,-1.74689612655491E-11));
#37858=CARTESIAN_POINT('Ctrl Pts',(7.27603390512273,-146.579517970998,-4.20082013377291));
#37859=CARTESIAN_POINT('Ctrl Pts',(4.85068927007173,-146.404517970998,-8.40164026752836));
#37860=CARTESIAN_POINT('Ctrl Pts',(-1.51301075899711E-11,-146.229517970998,
-8.40164026751963));
#37861=CARTESIAN_POINT('Ctrl Pts',(-4.85068927010199,-146.054517970998,
-8.4016402675109));
#37862=CARTESIAN_POINT('Ctrl Pts',(-7.27603390513785,-145.879517970998,
-4.20082013374671));
#37863=CARTESIAN_POINT('Ctrl Pts',(-9.70137854017372,-145.704517970998,
1.74701493417668E-11));
#37864=CARTESIAN_POINT('Ctrl Pts',(-7.27603390512272,-145.529517970998,
4.20082013377292));
#37865=CARTESIAN_POINT('Ctrl Pts',(-4.85068927007173,-145.354517970998,
8.40164026752836));
#37866=CARTESIAN_POINT('Ctrl Pts',(1.5129078685785E-11,-145.179517970998,
8.40164026751963));
#37867=CARTESIAN_POINT('Ctrl Pts',(4.85068927010198,-145.004517970998,8.4016402675109));
#37868=CARTESIAN_POINT('Ctrl Pts',(7.27603390513785,-144.829517970998,4.20082013374672));
#37869=CARTESIAN_POINT('Ctrl Pts',(9.70137854017372,-144.654517970998,-1.74689612655491E-11));
#37870=CARTESIAN_POINT('Ctrl Pts',(7.27603390512273,-144.479517970998,-4.20082013377291));
#37871=CARTESIAN_POINT('Ctrl Pts',(4.85068927007173,-144.304517970998,-8.40164026752836));
#37872=CARTESIAN_POINT('Ctrl Pts',(-1.51301075899711E-11,-144.129517970998,
-8.40164026751963));
#37873=CARTESIAN_POINT('Ctrl Pts',(-4.85068927010199,-143.954517970998,
-8.4016402675109));
#37874=CARTESIAN_POINT('Ctrl Pts',(-7.27603390513785,-143.779517970998,
-4.20082013374671));
#37875=CARTESIAN_POINT('Ctrl Pts',(-9.70137854017372,-143.604517970998,
1.74701493417668E-11));
#37876=CARTESIAN_POINT('Ctrl Pts',(-7.27603390512272,-143.429517970998,
4.20082013377292));
#37877=CARTESIAN_POINT('Ctrl Pts',(-4.85068927007173,-143.254517970998,
8.40164026752836));
#37878=CARTESIAN_POINT('Ctrl Pts',(1.5129078685785E-11,-143.079517970998,
8.40164026751963));
#37879=CARTESIAN_POINT('Ctrl Pts',(4.85068927010198,-142.904517970998,8.4016402675109));
#37880=CARTESIAN_POINT('Ctrl Pts',(7.27603390513785,-142.729517970998,4.20082013374672));
#37881=CARTESIAN_POINT('Ctrl Pts',(9.70137854017372,-142.554517970998,-1.74689612655491E-11));
#37882=CARTESIAN_POINT('Ctrl Pts',(7.27603390512273,-142.379517970998,-4.20082013377291));
#37883=CARTESIAN_POINT('Ctrl Pts',(4.85068927007173,-142.204517970998,-8.40164026752836));
#37884=CARTESIAN_POINT('Ctrl Pts',(-1.51301075899711E-11,-142.029517970998,
-8.40164026751963));
#37885=CARTESIAN_POINT('Ctrl Pts',(-4.85068927010199,-141.854517970998,
-8.4016402675109));
#37886=CARTESIAN_POINT('Ctrl Pts',(-7.27603390513785,-141.679517970998,
-4.20082013374671));
#37887=CARTESIAN_POINT('Ctrl Pts',(-9.70137854017372,-141.504517970998,
1.74701493417668E-11));
#37888=CARTESIAN_POINT('Ctrl Pts',(-7.27603390512272,-141.329517970998,
4.20082013377292));
#37889=CARTESIAN_POINT('Ctrl Pts',(-4.85068927007173,-141.154517970998,
8.40164026752836));
#37890=CARTESIAN_POINT('Ctrl Pts',(1.5129078685785E-11,-140.979517970998,
8.40164026751963));
#37891=CARTESIAN_POINT('Ctrl Pts',(4.85068927010198,-140.804517970998,8.4016402675109));
#37892=CARTESIAN_POINT('Ctrl Pts',(7.27603390513785,-140.629517970998,4.20082013374672));
#37893=CARTESIAN_POINT('Ctrl Pts',(9.70137854017372,-140.454517970998,-1.74689612655491E-11));
#37894=CARTESIAN_POINT('Ctrl Pts',(7.27603390512273,-140.279517970998,-4.20082013377291));
#37895=CARTESIAN_POINT('Ctrl Pts',(4.85068927007173,-140.104517970998,-8.40164026752836));
#37896=CARTESIAN_POINT('Ctrl Pts',(-1.51301075899711E-11,-139.929517970998,
-8.40164026751963));
#37897=CARTESIAN_POINT('Ctrl Pts',(-4.85068927010199,-139.754517970998,
-8.4016402675109));
#37898=CARTESIAN_POINT('Ctrl Pts',(-7.27603390513785,-139.579517970998,
-4.20082013374671));
#37899=CARTESIAN_POINT('Ctrl Pts',(-9.70137854017372,-139.404517970998,
1.74701493417668E-11));
#37900=CARTESIAN_POINT('Ctrl Pts',(-7.27603390512272,-139.229517970998,
4.20082013377292));
#37901=CARTESIAN_POINT('Ctrl Pts',(-4.85068927007173,-139.054517970998,
8.40164026752836));
#37902=CARTESIAN_POINT('Ctrl Pts',(1.5129078685785E-11,-138.879517970998,
8.40164026751963));
#37903=CARTESIAN_POINT('Ctrl Pts',(4.85068927010198,-138.704517970998,8.4016402675109));
#37904=CARTESIAN_POINT('Ctrl Pts',(7.27603390513785,-138.529517970998,4.20082013374672));
#37905=CARTESIAN_POINT('Ctrl Pts',(9.70137854017372,-138.354517970998,-1.74689612655491E-11));
#37906=CARTESIAN_POINT('Ctrl Pts',(7.27603390512273,-138.179517970998,-4.20082013377291));
#37907=CARTESIAN_POINT('Ctrl Pts',(4.85068927007173,-138.004517970998,-8.40164026752836));
#37908=CARTESIAN_POINT('Ctrl Pts',(-1.51301075899711E-11,-137.829517970998,
-8.40164026751963));
#37909=CARTESIAN_POINT('Ctrl Pts',(-4.85068927010199,-137.654517970998,
-8.4016402675109));
#37910=CARTESIAN_POINT('Ctrl Pts',(-7.27603390513785,-137.479517970998,
-4.20082013374671));
#37911=CARTESIAN_POINT('Ctrl Pts',(-9.70137854017372,-137.304517970998,
1.74701493417668E-11));
#37912=CARTESIAN_POINT('Ctrl Pts',(-7.27603390512272,-137.129517970998,
4.20082013377292));
#37913=CARTESIAN_POINT('Ctrl Pts',(-4.85068927007173,-136.954517970998,
8.40164026752836));
#37914=CARTESIAN_POINT('Ctrl Pts',(1.5129078685785E-11,-136.779517970998,
8.40164026751963));
#37915=CARTESIAN_POINT('Ctrl Pts',(4.85068927010198,-136.604517970998,8.4016402675109));
#37916=CARTESIAN_POINT('Ctrl Pts',(7.27603390513785,-136.429517970998,4.20082013374672));
#37917=CARTESIAN_POINT('Ctrl Pts',(9.70137854017372,-136.254517970999,-1.74689612655491E-11));
#37918=CARTESIAN_POINT('Ctrl Pts',(7.27603390512273,-136.079517970998,-4.20082013377291));
#37919=CARTESIAN_POINT('Ctrl Pts',(4.85068927007173,-135.904517970998,-8.40164026752836));
#37920=CARTESIAN_POINT('Ctrl Pts',(-1.51301075899711E-11,-135.729517970998,
-8.40164026751963));
#37921=CARTESIAN_POINT('Ctrl Pts',(-4.85068927010199,-135.554517970998,
-8.4016402675109));
#37922=CARTESIAN_POINT('Ctrl Pts',(-7.27603390513785,-135.379517970998,
-4.20082013374671));
#37923=CARTESIAN_POINT('Ctrl Pts',(-9.70137854017372,-135.204517970998,
1.74701493417668E-11));
#37924=CARTESIAN_POINT('Ctrl Pts',(-7.27603390512272,-135.029517970998,
4.20082013377292));
#37925=CARTESIAN_POINT('Ctrl Pts',(-4.85068927007173,-134.854517970998,
8.40164026752836));
#37926=CARTESIAN_POINT('Ctrl Pts',(1.5129078685785E-11,-134.679517970998,
8.40164026751963));
#37927=CARTESIAN_POINT('Ctrl Pts',(4.85068927010198,-134.504517970998,8.4016402675109));
#37928=CARTESIAN_POINT('Ctrl Pts',(7.27603390513785,-134.329517970998,4.20082013374672));
#37929=CARTESIAN_POINT('Ctrl Pts',(9.70137854017372,-134.154517970998,-1.74689612655491E-11));
#37930=CARTESIAN_POINT('Ctrl Pts',(7.27603390512273,-133.979517970998,-4.20082013377291));
#37931=CARTESIAN_POINT('Ctrl Pts',(4.85068927007173,-133.804517970998,-8.40164026752836));
#37932=CARTESIAN_POINT('Ctrl Pts',(-1.51301075899711E-11,-133.629517970998,
-8.40164026751963));
#37933=CARTESIAN_POINT('Ctrl Pts',(-4.85068927010199,-133.454517970998,
-8.4016402675109));
#37934=CARTESIAN_POINT('Ctrl Pts',(-7.27603390513785,-133.279517970998,
-4.20082013374671));
#37935=CARTESIAN_POINT('Ctrl Pts',(-9.70137854017372,-133.104517970998,
1.74701493417668E-11));
#37936=CARTESIAN_POINT('Ctrl Pts',(-7.27603390512272,-132.929517970998,
4.20082013377292));
#37937=CARTESIAN_POINT('Ctrl Pts',(-4.85068927007173,-132.754517970998,
8.40164026752836));
#37938=CARTESIAN_POINT('Ctrl Pts',(1.5129078685785E-11,-132.579517970998,
8.40164026751963));
#37939=CARTESIAN_POINT('Ctrl Pts',(4.85068927010198,-132.404517970998,8.4016402675109));
#37940=CARTESIAN_POINT('Ctrl Pts',(7.27603390513785,-132.229517970998,4.20082013374672));
#37941=CARTESIAN_POINT('Ctrl Pts',(9.70137854017372,-132.054517970998,-1.74689612655491E-11));
#37942=CARTESIAN_POINT('Ctrl Pts',(7.27603390512273,-131.879517970998,-4.20082013377291));
#37943=CARTESIAN_POINT('Ctrl Pts',(4.85068927007173,-131.704517970998,-8.40164026752836));
#37944=CARTESIAN_POINT('Ctrl Pts',(-1.51301075899711E-11,-131.529517970998,
-8.40164026751963));
#37945=CARTESIAN_POINT('Ctrl Pts',(-4.85068927010199,-131.354517970998,
-8.4016402675109));
#37946=CARTESIAN_POINT('Ctrl Pts',(-7.27603390513785,-131.179517970998,
-4.20082013374671));
#37947=CARTESIAN_POINT('Ctrl Pts',(-9.70137854017372,-131.004517970998,
1.74701493417668E-11));
#37948=CARTESIAN_POINT('Ctrl Pts',(-7.27603390512272,-130.829517970998,
4.20082013377292));
#37949=CARTESIAN_POINT('Ctrl Pts',(-4.85068927007173,-130.654517970998,
8.40164026752836));
#37950=CARTESIAN_POINT('Ctrl Pts',(1.5129078685785E-11,-130.479517970998,
8.40164026751963));
#37951=CARTESIAN_POINT('Ctrl Pts',(4.85068927010198,-130.304517970998,8.4016402675109));
#37952=CARTESIAN_POINT('Ctrl Pts',(7.27603390513785,-130.129517970998,4.20082013374672));
#37953=CARTESIAN_POINT('Ctrl Pts',(9.70137854017372,-129.954517970998,-1.74689612655491E-11));
#37954=CARTESIAN_POINT('Ctrl Pts',(7.27603390512273,-129.779517970998,-4.20082013377291));
#37955=CARTESIAN_POINT('Ctrl Pts',(4.85068927007173,-129.604517970998,-8.40164026752836));
#37956=CARTESIAN_POINT('Ctrl Pts',(-1.51301075899711E-11,-129.429517970998,
-8.40164026751963));
#37957=CARTESIAN_POINT('Ctrl Pts',(-4.85068927010199,-129.254517970998,
-8.4016402675109));
#37958=CARTESIAN_POINT('Ctrl Pts',(-7.27603390513785,-129.079517970998,
-4.20082013374671));
#37959=CARTESIAN_POINT('Ctrl Pts',(-9.70137854017372,-128.904517970998,
1.74701493417668E-11));
#37960=CARTESIAN_POINT('Ctrl Pts',(-7.27603390512272,-128.729517970998,
4.20082013377292));
#37961=CARTESIAN_POINT('Ctrl Pts',(-4.85068927007173,-128.554517970998,
8.40164026752836));
#37962=CARTESIAN_POINT('Ctrl Pts',(1.5129078685785E-11,-128.379517970998,
8.40164026751963));
#37963=CARTESIAN_POINT('Ctrl Pts',(4.85068927010198,-128.204517970998,8.4016402675109));
#37964=CARTESIAN_POINT('Ctrl Pts',(7.27603390513785,-128.029517970998,4.20082013374672));
#37965=CARTESIAN_POINT('Ctrl Pts',(9.70137854017372,-127.854517970998,-1.74689612655491E-11));
#37966=CARTESIAN_POINT('Ctrl Pts',(7.27603390512273,-127.679517970998,-4.20082013377291));
#37967=CARTESIAN_POINT('Ctrl Pts',(4.85068927007173,-127.504517970998,-8.40164026752836));
#37968=CARTESIAN_POINT('Ctrl Pts',(-1.51301075899711E-11,-127.329517970998,
-8.40164026751963));
#37969=CARTESIAN_POINT('Ctrl Pts',(-4.85068927010199,-127.154517970998,
-8.4016402675109));
#37970=CARTESIAN_POINT('Ctrl Pts',(-7.27603390513785,-126.979517970998,
-4.20082013374671));
#37971=CARTESIAN_POINT('Ctrl Pts',(-9.70137854017372,-126.804517970998,
1.74701493417668E-11));
#37972=CARTESIAN_POINT('Ctrl Pts',(-7.27603390512272,-126.629517970998,
4.20082013377292));
#37973=CARTESIAN_POINT('Ctrl Pts',(-4.85068927007173,-126.454517970998,
8.40164026752836));
#37974=CARTESIAN_POINT('Ctrl Pts',(1.5129078685785E-11,-126.279517970998,
8.40164026751963));
#37975=CARTESIAN_POINT('Ctrl Pts',(4.85068927010198,-126.104517970998,8.4016402675109));
#37976=CARTESIAN_POINT('Ctrl Pts',(7.27603390513785,-125.929517970998,4.20082013374672));
#37977=CARTESIAN_POINT('Ctrl Pts',(9.70137854017372,-125.754517970998,-1.74689612655491E-11));
#37978=CARTESIAN_POINT('Ctrl Pts',(7.27603390512273,-125.579517970998,-4.20082013377291));
#37979=CARTESIAN_POINT('Ctrl Pts',(4.85068927007173,-125.404517970998,-8.40164026752836));
#37980=CARTESIAN_POINT('Ctrl Pts',(-1.51301075899711E-11,-125.229517970998,
-8.40164026751963));
#37981=CARTESIAN_POINT('Ctrl Pts',(-4.85068927010199,-125.054517970998,
-8.4016402675109));
#37982=CARTESIAN_POINT('Ctrl Pts',(-7.27603390513785,-124.879517970998,
-4.20082013374671));
#37983=CARTESIAN_POINT('Ctrl Pts',(-9.70137854017372,-124.704517970998,
1.74701493417668E-11));
#37984=CARTESIAN_POINT('Ctrl Pts',(-7.27603390512272,-124.529517970998,
4.20082013377292));
#37985=CARTESIAN_POINT('Ctrl Pts',(-4.85068927007173,-124.354517970998,
8.40164026752836));
#37986=CARTESIAN_POINT('Ctrl Pts',(1.5129078685785E-11,-124.179517970998,
8.40164026751963));
#37987=CARTESIAN_POINT('Ctrl Pts',(4.85068927010198,-124.004517970998,8.4016402675109));
#37988=CARTESIAN_POINT('Ctrl Pts',(7.27603390513785,-123.829517970998,4.20082013374672));
#37989=CARTESIAN_POINT('Ctrl Pts',(9.70137854017372,-123.654517970998,-1.74689612655491E-11));
#37990=CARTESIAN_POINT('Ctrl Pts',(7.27603390512273,-123.479517970998,-4.20082013377291));
#37991=CARTESIAN_POINT('Ctrl Pts',(4.85068927007173,-123.304517970998,-8.40164026752836));
#37992=CARTESIAN_POINT('Ctrl Pts',(-1.51301075899711E-11,-123.129517970998,
-8.40164026751963));
#37993=CARTESIAN_POINT('Ctrl Pts',(-4.85068927010199,-122.954517970998,
-8.4016402675109));
#37994=CARTESIAN_POINT('Ctrl Pts',(-7.27603390513785,-122.779517970998,
-4.20082013374671));
#37995=CARTESIAN_POINT('Ctrl Pts',(-9.70137854017372,-122.604517970998,
1.74701493417668E-11));
#37996=CARTESIAN_POINT('Ctrl Pts',(-7.27603390512272,-122.429517970998,
4.20082013377292));
#37997=CARTESIAN_POINT('Ctrl Pts',(-4.85068927007173,-122.254517970998,
8.40164026752836));
#37998=CARTESIAN_POINT('Ctrl Pts',(1.5129078685785E-11,-122.079517970998,
8.40164026751963));
#37999=CARTESIAN_POINT('Ctrl Pts',(4.85068927010198,-121.904517970998,8.4016402675109));
#38000=CARTESIAN_POINT('Ctrl Pts',(7.27603390513785,-121.729517970998,4.20082013374672));
#38001=CARTESIAN_POINT('Ctrl Pts',(9.70137854017372,-121.554517970999,-1.74689612655491E-11));
#38002=CARTESIAN_POINT('Ctrl Pts',(7.27603390512273,-121.379517970998,-4.20082013377291));
#38003=CARTESIAN_POINT('Ctrl Pts',(4.85068927007173,-121.204517970998,-8.40164026752836));
#38004=CARTESIAN_POINT('Ctrl Pts',(-1.51301075899711E-11,-121.029517970998,
-8.40164026751963));
#38005=CARTESIAN_POINT('Ctrl Pts',(-4.85068927010199,-120.854517970999,
-8.4016402675109));
#38006=CARTESIAN_POINT('Ctrl Pts',(-7.27603390513785,-120.679517970999,
-4.20082013374671));
#38007=CARTESIAN_POINT('Ctrl Pts',(-9.70137854017372,-120.504517970999,
1.74701493417668E-11));
#38008=CARTESIAN_POINT('Ctrl Pts',(-7.27603390512272,-120.329517970998,
4.20082013377292));
#38009=CARTESIAN_POINT('Ctrl Pts',(-4.85068927007173,-120.154517970998,
8.40164026752836));
#38010=CARTESIAN_POINT('Ctrl Pts',(1.5129078685785E-11,-119.979517970999,
8.40164026751963));
#38011=CARTESIAN_POINT('Ctrl Pts',(4.85068927010198,-119.804517970999,8.4016402675109));
#38012=CARTESIAN_POINT('Ctrl Pts',(7.27603390513785,-119.629517970998,4.20082013374672));
#38013=CARTESIAN_POINT('Ctrl Pts',(9.70137854017372,-119.454517970998,-1.74689612655491E-11));
#38014=CARTESIAN_POINT('Ctrl Pts',(7.27603390512273,-119.279517970999,-4.20082013377291));
#38015=CARTESIAN_POINT('Ctrl Pts',(4.85068927007173,-119.104517970998,-8.40164026752836));
#38016=CARTESIAN_POINT('Ctrl Pts',(-1.51301075899711E-11,-118.929517970998,
-8.40164026751963));
#38017=CARTESIAN_POINT('Ctrl Pts',(-4.85068927010199,-118.754517970998,
-8.4016402675109));
#38018=CARTESIAN_POINT('Ctrl Pts',(-7.27603390513785,-118.579517970998,
-4.20082013374671));
#38019=CARTESIAN_POINT('Ctrl Pts',(-9.70137854017372,-118.404517970999,
1.74701493417668E-11));
#38020=CARTESIAN_POINT('Ctrl Pts',(-7.27603390512272,-118.229517970998,
4.20082013377292));
#38021=CARTESIAN_POINT('Ctrl Pts',(-4.85068927007173,-118.054517970998,
8.40164026752836));
#38022=CARTESIAN_POINT('Ctrl Pts',(1.5129078685785E-11,-117.879517970999,
8.40164026751963));
#38023=CARTESIAN_POINT('Ctrl Pts',(4.85068927010198,-117.704517970998,8.4016402675109));
#38024=CARTESIAN_POINT('Ctrl Pts',(7.27603390513785,-117.529517970998,4.20082013374672));
#38025=CARTESIAN_POINT('Ctrl Pts',(9.70137854017372,-117.354517970999,-1.74689612655491E-11));
#38026=CARTESIAN_POINT('Ctrl Pts',(7.27603390512273,-117.179517970999,-4.20082013377291));
#38027=CARTESIAN_POINT('Ctrl Pts',(4.85068927007173,-117.004517970999,-8.40164026752836));
#38028=CARTESIAN_POINT('Ctrl Pts',(-1.51301075899711E-11,-116.829517970998,
-8.40164026751963));
#38029=CARTESIAN_POINT('Ctrl Pts',(-4.85068927010199,-116.654517970998,
-8.4016402675109));
#38030=CARTESIAN_POINT('Ctrl Pts',(-7.27603390513785,-116.479517970999,
-4.20082013374671));
#38031=CARTESIAN_POINT('Ctrl Pts',(-9.70137854017372,-116.304517970999,
1.74701493417668E-11));
#38032=CARTESIAN_POINT('Ctrl Pts',(-7.27603390512272,-116.129517970999,
4.20082013377292));
#38033=CARTESIAN_POINT('Ctrl Pts',(-4.85068927007173,-115.954517970998,
8.40164026752836));
#38034=CARTESIAN_POINT('Ctrl Pts',(1.5129078685785E-11,-115.779517970998,
8.40164026751963));
#38035=CARTESIAN_POINT('Ctrl Pts',(4.85068927010198,-115.604517970999,8.4016402675109));
#38036=CARTESIAN_POINT('Ctrl Pts',(7.27603390513785,-115.429517970999,4.20082013374672));
#38037=CARTESIAN_POINT('Ctrl Pts',(9.70137854017372,-115.254517970999,-1.74689612655491E-11));
#38038=CARTESIAN_POINT('Ctrl Pts',(7.27603390512273,-115.079517970998,-4.20082013377291));
#38039=CARTESIAN_POINT('Ctrl Pts',(4.85068927007173,-114.904517970999,-8.40164026752836));
#38040=CARTESIAN_POINT('Ctrl Pts',(-1.51301075899711E-11,-114.729517970999,
-8.40164026751963));
#38041=CARTESIAN_POINT('Ctrl Pts',(-4.85068927010199,-114.554517970999,
-8.4016402675109));
#38042=CARTESIAN_POINT('Ctrl Pts',(-7.27603390513785,-114.379517970999,
-4.20082013374671));
#38043=CARTESIAN_POINT('Ctrl Pts',(-9.70137854017372,-114.204517970999,
1.74701493417668E-11));
#38044=CARTESIAN_POINT('Ctrl Pts',(-7.27603390512272,-114.029517970999,
4.20082013377292));
#38045=CARTESIAN_POINT('Ctrl Pts',(-4.85068927007173,-113.854517970999,
8.40164026752836));
#38046=CARTESIAN_POINT('Ctrl Pts',(1.5129078685785E-11,-113.679517970999,
8.40164026751963));
#38047=CARTESIAN_POINT('Ctrl Pts',(4.85068927010198,-113.504517970999,8.4016402675109));
#38048=CARTESIAN_POINT('Ctrl Pts',(7.27603390513785,-113.329517970999,4.20082013374672));
#38049=CARTESIAN_POINT('Ctrl Pts',(9.70137854017372,-113.154517970999,-1.74689612655491E-11));
#38050=CARTESIAN_POINT('Ctrl Pts',(7.27603390512273,-112.979517970999,-4.20082013377291));
#38051=CARTESIAN_POINT('Ctrl Pts',(4.85068927007173,-112.804517970999,-8.40164026752836));
#38052=CARTESIAN_POINT('Ctrl Pts',(-1.51301075899711E-11,-112.629517970999,
-8.40164026751963));
#38053=CARTESIAN_POINT('Ctrl Pts',(-4.85068927010199,-112.454517970998,
-8.4016402675109));
#38054=CARTESIAN_POINT('Ctrl Pts',(-7.27603390513785,-112.279517970998,
-4.20082013374671));
#38055=CARTESIAN_POINT('Ctrl Pts',(-9.70137854017372,-112.104517970999,
1.74701493417668E-11));
#38056=CARTESIAN_POINT('Ctrl Pts',(-7.27603390512272,-111.929517970999,
4.20082013377292));
#38057=CARTESIAN_POINT('Ctrl Pts',(-4.85068927007173,-111.754517970999,
8.40164026752836));
#38058=CARTESIAN_POINT('Ctrl Pts',(1.5129078685785E-11,-111.579517970999,
8.40164026751963));
#38059=CARTESIAN_POINT('Ctrl Pts',(4.85068927010198,-111.404517970998,8.4016402675109));
#38060=CARTESIAN_POINT('Ctrl Pts',(7.27603390513785,-111.229517970999,4.20082013374672));
#38061=CARTESIAN_POINT('Ctrl Pts',(9.70137854017372,-111.054517970999,-1.74689612655491E-11));
#38062=CARTESIAN_POINT('Ctrl Pts',(7.27603390512273,-110.879517970999,-4.20082013377291));
#38063=CARTESIAN_POINT('Ctrl Pts',(4.85068927007173,-110.704517970999,-8.40164026752836));
#38064=CARTESIAN_POINT('Ctrl Pts',(-1.51301075899711E-11,-110.529517970999,
-8.40164026751963));
#38065=CARTESIAN_POINT('Ctrl Pts',(-4.85068927010199,-110.354517970999,
-8.4016402675109));
#38066=CARTESIAN_POINT('Ctrl Pts',(-7.27603390513785,-110.179517970999,
-4.20082013374671));
#38067=CARTESIAN_POINT('Ctrl Pts',(-9.70137854017372,-110.004517970999,
1.74701493417668E-11));
#38068=CARTESIAN_POINT('Ctrl Pts',(-7.27603390512272,-109.829517970999,
4.20082013377292));
#38069=CARTESIAN_POINT('Ctrl Pts',(-4.85068927007173,-109.654517970999,
8.40164026752836));
#38070=CARTESIAN_POINT('Ctrl Pts',(1.5129078685785E-11,-109.479517970999,
8.40164026751963));
#38071=CARTESIAN_POINT('Ctrl Pts',(4.85068927010198,-109.304517970999,8.4016402675109));
#38072=CARTESIAN_POINT('Ctrl Pts',(7.27603390513785,-109.129517970999,4.20082013374672));
#38073=CARTESIAN_POINT('Ctrl Pts',(9.70137854017372,-108.954517970999,-1.74689612655491E-11));
#38074=CARTESIAN_POINT('Ctrl Pts',(7.27603390512273,-108.779517970999,-4.20082013377291));
#38075=CARTESIAN_POINT('Ctrl Pts',(4.85068927007173,-108.604517970999,-8.40164026752836));
#38076=CARTESIAN_POINT('Ctrl Pts',(-1.51301075899711E-11,-108.429517970999,
-8.40164026751963));
#38077=CARTESIAN_POINT('Ctrl Pts',(-4.85068927010199,-108.254517970999,
-8.4016402675109));
#38078=CARTESIAN_POINT('Ctrl Pts',(-7.27603390513785,-108.079517970999,
-4.20082013374671));
#38079=CARTESIAN_POINT('Ctrl Pts',(-9.70137854017372,-107.904517970999,
1.74701493417668E-11));
#38080=CARTESIAN_POINT('Ctrl Pts',(-7.27603390512272,-107.729517970999,
4.20082013377292));
#38081=CARTESIAN_POINT('Ctrl Pts',(-4.85068927007173,-107.554517970999,
8.40164026752836));
#38082=CARTESIAN_POINT('Ctrl Pts',(1.5129078685785E-11,-107.379517970999,
8.40164026751963));
#38083=CARTESIAN_POINT('Ctrl Pts',(4.85068927010198,-107.204517970999,8.4016402675109));
#38084=CARTESIAN_POINT('Ctrl Pts',(7.27603390513785,-107.029517970999,4.20082013374672));
#38085=CARTESIAN_POINT('Ctrl Pts',(9.70137854017372,-106.854517970999,-1.74689612655491E-11));
#38086=CARTESIAN_POINT('Ctrl Pts',(7.27603390512273,-106.679517970999,-4.20082013377291));
#38087=CARTESIAN_POINT('Ctrl Pts',(4.85068927007173,-106.504517970998,-8.40164026752836));
#38088=CARTESIAN_POINT('Ctrl Pts',(-1.51301075899711E-11,-106.329517970999,
-8.40164026751963));
#38089=CARTESIAN_POINT('Ctrl Pts',(-4.85068927010199,-106.154517970999,
-8.4016402675109));
#38090=CARTESIAN_POINT('Ctrl Pts',(-7.27603390513785,-105.979517970999,
-4.20082013374671));
#38091=CARTESIAN_POINT('Ctrl Pts',(-9.70137854017372,-105.804517970999,
1.74701493417668E-11));
#38092=CARTESIAN_POINT('Ctrl Pts',(-7.27603390512272,-105.629517970999,
4.20082013377292));
#38093=CARTESIAN_POINT('Ctrl Pts',(-4.85068927007173,-105.454517970999,
8.40164026752836));
#38094=CARTESIAN_POINT('Ctrl Pts',(1.5129078685785E-11,-105.279517970999,
8.40164026751963));
#38095=CARTESIAN_POINT('Ctrl Pts',(4.85068927010198,-105.104517970999,8.4016402675109));
#38096=CARTESIAN_POINT('Ctrl Pts',(7.27603390513785,-104.929517970999,4.20082013374672));
#38097=CARTESIAN_POINT('Ctrl Pts',(9.70137854017372,-104.754517970999,-1.74689612655491E-11));
#38098=CARTESIAN_POINT('Ctrl Pts',(7.27603390512273,-104.579517970999,-4.20082013377291));
#38099=CARTESIAN_POINT('Ctrl Pts',(4.85068927007173,-104.404517970999,-8.40164026752836));
#38100=CARTESIAN_POINT('Ctrl Pts',(-1.51301075899711E-11,-104.229517970999,
-8.40164026751963));
#38101=CARTESIAN_POINT('Ctrl Pts',(-4.85068927010199,-104.054517970999,
-8.4016402675109));
#38102=CARTESIAN_POINT('Ctrl Pts',(-7.27603390513785,-103.879517970999,
-4.20082013374671));
#38103=CARTESIAN_POINT('Ctrl Pts',(-9.70137854017372,-103.704517970999,
1.74701493417668E-11));
#38104=CARTESIAN_POINT('Ctrl Pts',(-7.27603390512272,-103.529517970999,
4.20082013377292));
#38105=CARTESIAN_POINT('Ctrl Pts',(-4.85068927007173,-103.354517970999,
8.40164026752836));
#38106=CARTESIAN_POINT('Ctrl Pts',(1.5129078685785E-11,-103.179517970999,
8.40164026751963));
#38107=CARTESIAN_POINT('Ctrl Pts',(4.85068927010198,-103.004517970999,8.4016402675109));
#38108=CARTESIAN_POINT('Ctrl Pts',(7.27603390513785,-102.829517970999,4.20082013374672));
#38109=CARTESIAN_POINT('Ctrl Pts',(9.70137854017372,-102.654517970999,-1.74689612655491E-11));
#38110=CARTESIAN_POINT('Ctrl Pts',(7.27603390512273,-102.479517970999,-4.20082013377291));
#38111=CARTESIAN_POINT('Ctrl Pts',(4.85068927007173,-102.304517970999,-8.40164026752836));
#38112=CARTESIAN_POINT('Ctrl Pts',(-1.51301075899711E-11,-102.129517970999,
-8.40164026751963));
#38113=CARTESIAN_POINT('Ctrl Pts',(-4.85068927010199,-101.954517970999,
-8.4016402675109));
#38114=CARTESIAN_POINT('Ctrl Pts',(-7.27603390513785,-101.779517970999,
-4.20082013374671));
#38115=CARTESIAN_POINT('Ctrl Pts',(-9.70137854017372,-101.604517970999,
1.74701493417668E-11));
#38116=CARTESIAN_POINT('Ctrl Pts',(-7.27603390512272,-101.429517970999,
4.20082013377292));
#38117=CARTESIAN_POINT('Ctrl Pts',(-4.85068927007173,-101.254517970999,
8.40164026752836));
#38118=CARTESIAN_POINT('Ctrl Pts',(1.5129078685785E-11,-101.079517970999,
8.40164026751963));
#38119=CARTESIAN_POINT('Ctrl Pts',(4.85068927010198,-100.904517970999,8.4016402675109));
#38120=CARTESIAN_POINT('Ctrl Pts',(7.27603390513785,-100.729517970999,4.20082013374672));
#38121=CARTESIAN_POINT('Ctrl Pts',(9.70137854017372,-100.554517970999,-1.74689612655491E-11));
#38122=CARTESIAN_POINT('Ctrl Pts',(7.27603390512273,-100.379517970999,-4.20082013377291));
#38123=CARTESIAN_POINT('Ctrl Pts',(4.85068927007173,-100.204517970999,-8.40164026752836));
#38124=CARTESIAN_POINT('Ctrl Pts',(-1.51301075899711E-11,-100.029517970999,
-8.40164026751963));
#38125=CARTESIAN_POINT('Ctrl Pts',(-4.85068927010199,-99.8545179709986,
-8.4016402675109));
#38126=CARTESIAN_POINT('Ctrl Pts',(-7.27603390513785,-99.6795179709985,
-4.20082013374671));
#38127=CARTESIAN_POINT('Ctrl Pts',(-9.70137854017372,-99.5045179709985,
1.74701493417668E-11));
#38128=CARTESIAN_POINT('Ctrl Pts',(-7.27603390512272,-99.3295179709985,
4.20082013377292));
#38129=CARTESIAN_POINT('Ctrl Pts',(-4.85068927007173,-99.1545179709985,
8.40164026752836));
#38130=CARTESIAN_POINT('Ctrl Pts',(1.5129078685785E-11,-98.9795179709985,
8.40164026751963));
#38131=CARTESIAN_POINT('Ctrl Pts',(4.85068927010198,-98.8045179709985,8.4016402675109));
#38132=CARTESIAN_POINT('Ctrl Pts',(7.27603390513785,-98.6295179709985,4.20082013374672));
#38133=CARTESIAN_POINT('Ctrl Pts',(9.70137854017372,-98.4545179709986,-1.74689612655491E-11));
#38134=CARTESIAN_POINT('Ctrl Pts',(7.27603390512273,-98.2795179709986,-4.20082013377291));
#38135=CARTESIAN_POINT('Ctrl Pts',(4.85068927007173,-98.1045179709986,-8.40164026752836));
#38136=CARTESIAN_POINT('Ctrl Pts',(-1.51301075899711E-11,-97.9295179709985,
-8.40164026751963));
#38137=CARTESIAN_POINT('Ctrl Pts',(-4.85068927010199,-97.7545179709985,
-8.4016402675109));
#38138=CARTESIAN_POINT('Ctrl Pts',(-7.27603390513785,-97.5795179709986,
-4.20082013374671));
#38139=CARTESIAN_POINT('Ctrl Pts',(-9.70137854017372,-97.4045179709985,
1.74701493417668E-11));
#38140=CARTESIAN_POINT('Ctrl Pts',(-7.27603390512272,-97.2295179709985,
4.20082013377292));
#38141=CARTESIAN_POINT('Ctrl Pts',(-4.85068927007173,-97.0545179709985,
8.40164026752836));
#38142=CARTESIAN_POINT('Ctrl Pts',(1.5129078685785E-11,-96.8795179709986,
8.40164026751963));
#38143=CARTESIAN_POINT('Ctrl Pts',(4.85068927010198,-96.7045179709986,8.4016402675109));
#38144=CARTESIAN_POINT('Ctrl Pts',(7.27603390513785,-96.5295179709985,4.20082013374672));
#38145=CARTESIAN_POINT('Ctrl Pts',(9.70137854017372,-96.3545179709985,-1.74689612655491E-11));
#38146=CARTESIAN_POINT('Ctrl Pts',(7.27603390512273,-96.1795179709985,-4.20082013377291));
#38147=CARTESIAN_POINT('Ctrl Pts',(4.85068927007173,-96.0045179709986,-8.40164026752836));
#38148=CARTESIAN_POINT('Ctrl Pts',(-1.51301075899711E-11,-95.8295179709985,
-8.40164026751963));
#38149=CARTESIAN_POINT('Ctrl Pts',(-4.85068927010199,-95.6545179709985,
-8.4016402675109));
#38150=CARTESIAN_POINT('Ctrl Pts',(-7.27603390513785,-95.4795179709985,
-4.20082013374671));
#38151=CARTESIAN_POINT('Ctrl Pts',(-9.70137854017372,-95.3045179709986,
1.74701493417668E-11));
#38152=CARTESIAN_POINT('Ctrl Pts',(-7.27603390512272,-95.1295179709986,
4.20082013377292));
#38153=CARTESIAN_POINT('Ctrl Pts',(-4.85068927007173,-94.9545179709986,
8.40164026752836));
#38154=CARTESIAN_POINT('Ctrl Pts',(1.5129078685785E-11,-94.7795179709985,
8.40164026751963));
#38155=CARTESIAN_POINT('Ctrl Pts',(4.85068927010198,-94.6045179709986,8.4016402675109));
#38156=CARTESIAN_POINT('Ctrl Pts',(7.27603390513785,-94.4295179709985,4.20082013374672));
#38157=CARTESIAN_POINT('Ctrl Pts',(9.70137854017372,-94.2545179709985,-1.74689612655491E-11));
#38158=CARTESIAN_POINT('Ctrl Pts',(7.27603390512273,-94.0795179709986,-4.20082013377291));
#38159=CARTESIAN_POINT('Ctrl Pts',(4.85068927007173,-93.9045179709986,-8.40164026752836));
#38160=CARTESIAN_POINT('Ctrl Pts',(-1.51301075899711E-11,-93.7295179709986,
-8.40164026751963));
#38161=CARTESIAN_POINT('Ctrl Pts',(-4.85068927010199,-93.5545179709985,
-8.4016402675109));
#38162=CARTESIAN_POINT('Ctrl Pts',(-7.27603390513785,-93.3795179709985,
-4.20082013374671));
#38163=CARTESIAN_POINT('Ctrl Pts',(-9.70137854017372,-93.2045179709986,
1.74701493417668E-11));
#38164=CARTESIAN_POINT('Ctrl Pts',(-7.27603390512272,-93.0295179709986,
4.20082013377292));
#38165=CARTESIAN_POINT('Ctrl Pts',(-4.85068927007173,-92.8545179709985,
8.40164026752836));
#38166=CARTESIAN_POINT('Ctrl Pts',(1.5129078685785E-11,-92.6795179709985,
8.40164026751963));
#38167=CARTESIAN_POINT('Ctrl Pts',(4.85068927010198,-92.5045179709985,8.4016402675109));
#38168=CARTESIAN_POINT('Ctrl Pts',(7.27603390513785,-92.3295179709986,4.20082013374672));
#38169=CARTESIAN_POINT('Ctrl Pts',(9.70137854017372,-92.1545179709986,-1.74689612655491E-11));
#38170=CARTESIAN_POINT('Ctrl Pts',(7.27603390512273,-91.9795179709986,-4.20082013377291));
#38171=CARTESIAN_POINT('Ctrl Pts',(4.85068927007173,-91.8045179709985,-8.40164026752836));
#38172=CARTESIAN_POINT('Ctrl Pts',(-1.51301075899711E-11,-91.6295179709986,
-8.40164026751963));
#38173=CARTESIAN_POINT('Ctrl Pts',(-4.85068927010199,-91.4545179709986,
-8.4016402675109));
#38174=CARTESIAN_POINT('Ctrl Pts',(-7.27603390513785,-91.2795179709986,
-4.20082013374671));
#38175=CARTESIAN_POINT('Ctrl Pts',(-9.70137854017372,-91.1045179709985,
1.74701493417668E-11));
#38176=CARTESIAN_POINT('Ctrl Pts',(-7.27603390512272,-90.9295179709986,
4.20082013377292));
#38177=CARTESIAN_POINT('Ctrl Pts',(-4.85068927007173,-90.7545179709986,
8.40164026752836));
#38178=CARTESIAN_POINT('Ctrl Pts',(1.5129078685785E-11,-90.5795179709986,
8.40164026751963));
#38179=CARTESIAN_POINT('Ctrl Pts',(4.85068927010198,-90.4045179709985,8.4016402675109));
#38180=CARTESIAN_POINT('Ctrl Pts',(7.27603390513785,-90.2295179709986,4.20082013374672));
#38181=CARTESIAN_POINT('Ctrl Pts',(9.70137854017372,-90.0545179709986,-1.74689612655491E-11));
#38182=CARTESIAN_POINT('Ctrl Pts',(7.27603390512273,-89.8795179709985,-4.20082013377291));
#38183=CARTESIAN_POINT('Ctrl Pts',(4.85068927007173,-89.7045179709986,-8.40164026752836));
#38184=CARTESIAN_POINT('Ctrl Pts',(-1.51301075899711E-11,-89.5295179709986,
-8.40164026751963));
#38185=CARTESIAN_POINT('Ctrl Pts',(-4.85068927010199,-89.3545179709986,
-8.4016402675109));
#38186=CARTESIAN_POINT('Ctrl Pts',(-7.27603390513785,-89.1795179709986,
-4.20082013374671));
#38187=CARTESIAN_POINT('Ctrl Pts',(-9.70137854017372,-89.0045179709985,
1.74701493417668E-11));
#38188=CARTESIAN_POINT('Ctrl Pts',(-7.27603390512272,-88.8295179709986,
4.20082013377292));
#38189=CARTESIAN_POINT('Ctrl Pts',(-4.85068927007173,-88.6545179709986,
8.40164026752836));
#38190=CARTESIAN_POINT('Ctrl Pts',(1.5129078685785E-11,-88.4795179709986,
8.40164026751963));
#38191=CARTESIAN_POINT('Ctrl Pts',(4.85068927010198,-88.3045179709985,8.4016402675109));
#38192=CARTESIAN_POINT('Ctrl Pts',(7.27603390513785,-88.1295179709985,4.20082013374672));
#38193=CARTESIAN_POINT('Ctrl Pts',(9.70137854017372,-87.9545179709986,-1.74689612655491E-11));
#38194=CARTESIAN_POINT('Ctrl Pts',(7.27603390512273,-87.7795179709986,-4.20082013377291));
#38195=CARTESIAN_POINT('Ctrl Pts',(4.85068927007173,-87.6045179709986,-8.40164026752836));
#38196=CARTESIAN_POINT('Ctrl Pts',(-1.51301075899711E-11,-87.4295179709986,
-8.40164026751963));
#38197=CARTESIAN_POINT('Ctrl Pts',(-4.85068927010199,-87.2545179709986,
-8.4016402675109));
#38198=CARTESIAN_POINT('Ctrl Pts',(-7.27603390513785,-87.0795179709986,
-4.20082013374671));
#38199=CARTESIAN_POINT('Ctrl Pts',(-9.70137854017372,-86.9045179709986,
1.74701493417668E-11));
#38200=CARTESIAN_POINT('Ctrl Pts',(-7.27603390512272,-86.7295179709986,
4.20082013377292));
#38201=CARTESIAN_POINT('Ctrl Pts',(-4.85068927007173,-86.5545179709986,
8.40164026752836));
#38202=CARTESIAN_POINT('Ctrl Pts',(1.5129078685785E-11,-86.3795179709986,
8.40164026751963));
#38203=CARTESIAN_POINT('Ctrl Pts',(4.85068927010198,-86.2045179709986,8.4016402675109));
#38204=CARTESIAN_POINT('Ctrl Pts',(7.27603390513785,-86.0295179709986,4.20082013374672));
#38205=CARTESIAN_POINT('Ctrl Pts',(9.70137854017372,-85.8545179709986,-1.74689612655491E-11));
#38206=CARTESIAN_POINT('Ctrl Pts',(7.27603390512273,-85.6795179709986,-4.20082013377291));
#38207=CARTESIAN_POINT('Ctrl Pts',(4.85068927007173,-85.5045179709986,-8.40164026752836));
#38208=CARTESIAN_POINT('Ctrl Pts',(-1.51301075899711E-11,-85.3295179709986,
-8.40164026751963));
#38209=CARTESIAN_POINT('Ctrl Pts',(-4.85068927010199,-85.1545179709986,
-8.4016402675109));
#38210=CARTESIAN_POINT('Ctrl Pts',(-7.27603390513785,-84.9795179709986,
-4.20082013374671));
#38211=CARTESIAN_POINT('Ctrl Pts',(-9.70137854017372,-84.8045179709986,
1.74701493417668E-11));
#38212=CARTESIAN_POINT('Ctrl Pts',(-7.27603390512272,-84.6295179709986,
4.20082013377292));
#38213=CARTESIAN_POINT('Ctrl Pts',(-4.85068927007173,-84.4545179709986,
8.40164026752836));
#38214=CARTESIAN_POINT('Ctrl Pts',(1.5129078685785E-11,-84.2795179709986,
8.40164026751963));
#38215=CARTESIAN_POINT('Ctrl Pts',(4.85068927010198,-84.1045179709986,8.4016402675109));
#38216=CARTESIAN_POINT('Ctrl Pts',(7.27603390513785,-83.9295179709986,4.20082013374672));
#38217=CARTESIAN_POINT('Ctrl Pts',(9.70137854017372,-83.7545179709985,-1.74689612655491E-11));
#38218=CARTESIAN_POINT('Ctrl Pts',(7.27603390512273,-83.5795179709986,-4.20082013377291));
#38219=CARTESIAN_POINT('Ctrl Pts',(4.85068927007173,-83.4045179709986,-8.40164026752836));
#38220=CARTESIAN_POINT('Ctrl Pts',(-1.51301075899711E-11,-83.2295179709986,
-8.40164026751963));
#38221=CARTESIAN_POINT('Ctrl Pts',(-4.85068927010199,-83.0545179709986,
-8.4016402675109));
#38222=CARTESIAN_POINT('Ctrl Pts',(-7.27603390513785,-82.8795179709986,
-4.20082013374671));
#38223=CARTESIAN_POINT('Ctrl Pts',(-9.70137854017372,-82.7045179709986,
1.74701493417668E-11));
#38224=CARTESIAN_POINT('Ctrl Pts',(-7.27603390512272,-82.5295179709986,
4.20082013377292));
#38225=CARTESIAN_POINT('Ctrl Pts',(-4.85068927007173,-82.3545179709986,
8.40164026752836));
#38226=CARTESIAN_POINT('Ctrl Pts',(1.5129078685785E-11,-82.1795179709986,
8.40164026751963));
#38227=CARTESIAN_POINT('Ctrl Pts',(4.85068927010198,-82.0045179709986,8.4016402675109));
#38228=CARTESIAN_POINT('Ctrl Pts',(7.27603390513785,-81.8295179709986,4.20082013374672));
#38229=CARTESIAN_POINT('Ctrl Pts',(9.70137854017372,-81.6545179709986,-1.74689612655491E-11));
#38230=CARTESIAN_POINT('Ctrl Pts',(7.27603390512273,-81.4795179709986,-4.20082013377291));
#38231=CARTESIAN_POINT('Ctrl Pts',(4.85068927007173,-81.3045179709986,-8.40164026752836));
#38232=CARTESIAN_POINT('Ctrl Pts',(-1.51301075899711E-11,-81.1295179709986,
-8.40164026751963));
#38233=CARTESIAN_POINT('Ctrl Pts',(-4.85068927010199,-80.9545179709986,
-8.4016402675109));
#38234=CARTESIAN_POINT('Ctrl Pts',(-7.27603390513785,-80.7795179709986,
-4.20082013374671));
#38235=CARTESIAN_POINT('Ctrl Pts',(-9.70137854017372,-80.6045179709986,
1.74701493417668E-11));
#38236=CARTESIAN_POINT('Ctrl Pts',(-7.27603390512272,-80.4295179709986,
4.20082013377292));
#38237=CARTESIAN_POINT('Ctrl Pts',(-4.85068927007173,-80.2545179709986,
8.40164026752836));
#38238=CARTESIAN_POINT('Ctrl Pts',(1.5129078685785E-11,-80.0795179709986,
8.40164026751963));
#38239=CARTESIAN_POINT('Ctrl Pts',(4.85068927010198,-79.9045179709986,8.4016402675109));
#38240=CARTESIAN_POINT('Ctrl Pts',(7.27603390513785,-79.7295179709986,4.20082013374672));
#38241=CARTESIAN_POINT('Ctrl Pts',(9.70137854017372,-79.5545179709986,-1.74689612655491E-11));
#38242=CARTESIAN_POINT('Ctrl Pts',(7.27603390512273,-79.3795179709986,-4.20082013377291));
#38243=CARTESIAN_POINT('Ctrl Pts',(4.85068927007173,-79.2045179709986,-8.40164026752836));
#38244=CARTESIAN_POINT('Ctrl Pts',(-1.51301075899711E-11,-79.0295179709986,
-8.40164026751963));
#38245=CARTESIAN_POINT('Ctrl Pts',(-4.85068927010199,-78.8545179709986,
-8.4016402675109));
#38246=CARTESIAN_POINT('Ctrl Pts',(-7.27603390513785,-78.6795179709986,
-4.20082013374671));
#38247=CARTESIAN_POINT('Ctrl Pts',(-9.70137854017372,-78.5045179709986,
1.74701493417668E-11));
#38248=CARTESIAN_POINT('Ctrl Pts',(-7.27603390512272,-78.3295179709986,
4.20082013377292));
#38249=CARTESIAN_POINT('Ctrl Pts',(-4.85068927007173,-78.1545179709986,
8.40164026752836));
#38250=CARTESIAN_POINT('Ctrl Pts',(1.5129078685785E-11,-77.9795179709986,
8.40164026751963));
#38251=CARTESIAN_POINT('Ctrl Pts',(4.85068927010198,-77.8045179709986,8.4016402675109));
#38252=CARTESIAN_POINT('Ctrl Pts',(7.27603390513785,-77.6295179709986,4.20082013374672));
#38253=CARTESIAN_POINT('Ctrl Pts',(9.70137854017372,-77.4545179709986,-1.74689612655491E-11));
#38254=CARTESIAN_POINT('Ctrl Pts',(7.27603390512273,-77.2795179709986,-4.20082013377291));
#38255=CARTESIAN_POINT('Ctrl Pts',(4.85068927007173,-77.1045179709986,-8.40164026752836));
#38256=CARTESIAN_POINT('Ctrl Pts',(-1.51301075899711E-11,-76.9295179709986,
-8.40164026751963));
#38257=CARTESIAN_POINT('Ctrl Pts',(-4.85068927010199,-76.7545179709986,
-8.4016402675109));
#38258=CARTESIAN_POINT('Ctrl Pts',(-7.27603390513785,-76.5795179709986,
-4.20082013374671));
#38259=CARTESIAN_POINT('Ctrl Pts',(-9.70137854017372,-76.4045179709986,
1.74701493417668E-11));
#38260=CARTESIAN_POINT('Ctrl Pts',(-7.27603390512272,-76.2295179709986,
4.20082013377292));
#38261=CARTESIAN_POINT('Ctrl Pts',(-4.85068927007173,-76.0545179709986,
8.40164026752836));
#38262=CARTESIAN_POINT('Ctrl Pts',(1.5129078685785E-11,-75.8795179709986,
8.40164026751963));
#38263=CARTESIAN_POINT('Ctrl Pts',(4.85068927010198,-75.7045179709986,8.4016402675109));
#38264=CARTESIAN_POINT('Ctrl Pts',(7.27603390513785,-75.5295179709986,4.20082013374672));
#38265=CARTESIAN_POINT('Ctrl Pts',(9.70137854017372,-75.3545179709986,-1.74689612655491E-11));
#38266=CARTESIAN_POINT('Ctrl Pts',(7.27603390512273,-75.1795179709986,-4.20082013377291));
#38267=CARTESIAN_POINT('Ctrl Pts',(4.85068927007173,-75.0045179709986,-8.40164026752836));
#38268=CARTESIAN_POINT('Ctrl Pts',(-1.51301075899711E-11,-74.8295179709986,
-8.40164026751963));
#38269=CARTESIAN_POINT('Ctrl Pts',(-4.85068927010199,-74.6545179709986,
-8.4016402675109));
#38270=CARTESIAN_POINT('Ctrl Pts',(-7.27603390513785,-74.4795179709986,
-4.20082013374671));
#38271=CARTESIAN_POINT('Ctrl Pts',(-9.70137854017372,-74.3045179709986,
1.74701493417668E-11));
#38272=CARTESIAN_POINT('Ctrl Pts',(-7.27603390512272,-74.1295179709986,
4.20082013377292));
#38273=CARTESIAN_POINT('Ctrl Pts',(-4.85068927007173,-73.9545179709986,
8.40164026752836));
#38274=CARTESIAN_POINT('Ctrl Pts',(1.5129078685785E-11,-73.7795179709986,
8.40164026751963));
#38275=CARTESIAN_POINT('Ctrl Pts',(4.85068927010198,-73.6045179709986,8.4016402675109));
#38276=CARTESIAN_POINT('Ctrl Pts',(7.27603390513785,-73.4295179709986,4.20082013374672));
#38277=CARTESIAN_POINT('Ctrl Pts',(9.70137854017372,-73.2545179709986,-1.74689612655491E-11));
#38278=CARTESIAN_POINT('Ctrl Pts',(7.27603390512273,-73.0795179709986,-4.20082013377291));
#38279=CARTESIAN_POINT('Ctrl Pts',(4.85068927007173,-72.9045179709986,-8.40164026752836));
#38280=CARTESIAN_POINT('Ctrl Pts',(-1.51301075899711E-11,-72.7295179709986,
-8.40164026751963));
#38281=CARTESIAN_POINT('Ctrl Pts',(-4.85068927010199,-72.5545179709986,
-8.4016402675109));
#38282=CARTESIAN_POINT('Ctrl Pts',(-7.27603390513785,-72.3795179709986,
-4.20082013374671));
#38283=CARTESIAN_POINT('Ctrl Pts',(-9.70137854017372,-72.2045179709986,
1.74701493417668E-11));
#38284=CARTESIAN_POINT('Ctrl Pts',(-7.27603390512272,-72.0295179709986,
4.20082013377292));
#38285=CARTESIAN_POINT('Ctrl Pts',(-4.85068927007173,-71.8545179709986,
8.40164026752836));
#38286=CARTESIAN_POINT('Ctrl Pts',(1.5129078685785E-11,-71.6795179709986,
8.40164026751963));
#38287=CARTESIAN_POINT('Ctrl Pts',(4.85068927010198,-71.5045179709986,8.4016402675109));
#38288=CARTESIAN_POINT('Ctrl Pts',(7.27603390513785,-71.3295179709986,4.20082013374672));
#38289=CARTESIAN_POINT('Ctrl Pts',(9.70137854017372,-71.1545179709986,-1.74689612655491E-11));
#38290=CARTESIAN_POINT('Ctrl Pts',(7.27603390512273,-70.9795179709986,-4.20082013377291));
#38291=CARTESIAN_POINT('Ctrl Pts',(4.85068927007173,-70.8045179709986,-8.40164026752836));
#38292=CARTESIAN_POINT('Ctrl Pts',(-1.51301075899711E-11,-70.6295179709986,
-8.40164026751963));
#38293=CARTESIAN_POINT('Ctrl Pts',(-4.85068927010199,-70.4545179709986,
-8.4016402675109));
#38294=CARTESIAN_POINT('Ctrl Pts',(-7.27603390513785,-70.2795179709986,
-4.20082013374671));
#38295=CARTESIAN_POINT('Ctrl Pts',(-9.70137854017372,-70.1045179709986,
1.74701493417668E-11));
#38296=CARTESIAN_POINT('Ctrl Pts',(-7.27603390512272,-69.9295179709986,
4.20082013377292));
#38297=CARTESIAN_POINT('Ctrl Pts',(-4.85068927007173,-69.7545179709986,
8.40164026752836));
#38298=CARTESIAN_POINT('Ctrl Pts',(1.5129078685785E-11,-69.5795179709986,
8.40164026751963));
#38299=CARTESIAN_POINT('Ctrl Pts',(4.85068927010198,-69.4045179709986,8.4016402675109));
#38300=CARTESIAN_POINT('Ctrl Pts',(7.27603390513785,-69.2295179709986,4.20082013374672));
#38301=CARTESIAN_POINT('Ctrl Pts',(9.70137854017372,-69.0545179709986,-1.74689612655491E-11));
#38302=CARTESIAN_POINT('Ctrl Pts',(7.27603390512273,-68.8795179709986,-4.20082013377291));
#38303=CARTESIAN_POINT('Ctrl Pts',(4.85068927007173,-68.7045179709986,-8.40164026752836));
#38304=CARTESIAN_POINT('Ctrl Pts',(-1.51301075899711E-11,-68.5295179709986,
-8.40164026751963));
#38305=CARTESIAN_POINT('Ctrl Pts',(-4.85068927010199,-68.3545179709986,
-8.4016402675109));
#38306=CARTESIAN_POINT('Ctrl Pts',(-7.27603390513785,-68.1795179709986,
-4.20082013374671));
#38307=CARTESIAN_POINT('Ctrl Pts',(-9.70137854017372,-68.0045179709986,
1.74701493417668E-11));
#38308=CARTESIAN_POINT('Ctrl Pts',(-7.27603390512272,-67.8295179709986,
4.20082013377292));
#38309=CARTESIAN_POINT('Ctrl Pts',(-4.85068927007173,-67.6545179709986,
8.40164026752836));
#38310=CARTESIAN_POINT('Ctrl Pts',(1.5129078685785E-11,-67.4795179709986,
8.40164026751963));
#38311=CARTESIAN_POINT('Ctrl Pts',(4.85068927010198,-67.3045179709986,8.4016402675109));
#38312=CARTESIAN_POINT('Ctrl Pts',(7.27603390513785,-67.1295179709986,4.20082013374672));
#38313=CARTESIAN_POINT('Ctrl Pts',(9.70137854017372,-66.9545179709986,-1.74689612655491E-11));
#38314=CARTESIAN_POINT('Ctrl Pts',(7.27603390512273,-66.7795179709986,-4.20082013377291));
#38315=CARTESIAN_POINT('Ctrl Pts',(4.85068927007173,-66.6045179709986,-8.40164026752836));
#38316=CARTESIAN_POINT('Ctrl Pts',(-1.51301075899711E-11,-66.4295179709986,
-8.40164026751963));
#38317=CARTESIAN_POINT('Ctrl Pts',(-4.85068927010199,-66.2545179709986,
-8.4016402675109));
#38318=CARTESIAN_POINT('Ctrl Pts',(-7.27603390513785,-66.0795179709986,
-4.20082013374671));
#38319=CARTESIAN_POINT('Ctrl Pts',(-9.70137854017372,-65.9045179709986,
1.74701493417668E-11));
#38320=CARTESIAN_POINT('Ctrl Pts',(-7.27603390512272,-65.7295179709986,
4.20082013377292));
#38321=CARTESIAN_POINT('Ctrl Pts',(-4.85068927007173,-65.5545179709986,
8.40164026752836));
#38322=CARTESIAN_POINT('Ctrl Pts',(1.5129078685785E-11,-65.3795179709986,
8.40164026751963));
#38323=CARTESIAN_POINT('Ctrl Pts',(4.85068927010198,-65.2045179709986,8.4016402675109));
#38324=CARTESIAN_POINT('Ctrl Pts',(7.27603390513785,-65.0295179709986,4.20082013374672));
#38325=CARTESIAN_POINT('Ctrl Pts',(9.70137854017372,-64.8545179709986,-1.74689612655491E-11));
#38326=CARTESIAN_POINT('Ctrl Pts',(7.27603390512273,-64.6795179709986,-4.20082013377291));
#38327=CARTESIAN_POINT('Ctrl Pts',(4.85068927007173,-64.5045179709986,-8.40164026752836));
#38328=CARTESIAN_POINT('Ctrl Pts',(-1.51301075899711E-11,-64.3295179709986,
-8.40164026751963));
#38329=CARTESIAN_POINT('Ctrl Pts',(-4.85068927010199,-64.1545179709986,
-8.4016402675109));
#38330=CARTESIAN_POINT('Ctrl Pts',(-7.27603390513785,-63.9795179709986,
-4.20082013374671));
#38331=CARTESIAN_POINT('Ctrl Pts',(-9.70137854017372,-63.8045179709986,
1.74701493417668E-11));
#38332=CARTESIAN_POINT('Ctrl Pts',(-7.27603390512272,-63.6295179709986,
4.20082013377292));
#38333=CARTESIAN_POINT('Ctrl Pts',(-4.85068927007173,-63.4545179709986,
8.40164026752836));
#38334=CARTESIAN_POINT('Ctrl Pts',(1.5129078685785E-11,-63.2795179709986,
8.40164026751963));
#38335=CARTESIAN_POINT('Ctrl Pts',(4.85068927010198,-63.1045179709986,8.4016402675109));
#38336=CARTESIAN_POINT('Ctrl Pts',(7.27603390513785,-62.9295179709986,4.20082013374672));
#38337=CARTESIAN_POINT('Ctrl Pts',(9.70137854017372,-62.7545179709986,-1.74689612655491E-11));
#38338=CARTESIAN_POINT('Ctrl Pts',(7.27603390512273,-62.5795179709986,-4.20082013377291));
#38339=CARTESIAN_POINT('Ctrl Pts',(4.85068927007173,-62.4045179709986,-8.40164026752836));
#38340=CARTESIAN_POINT('Ctrl Pts',(-1.51301075899711E-11,-62.2295179709986,
-8.40164026751963));
#38341=CARTESIAN_POINT('Ctrl Pts',(-4.85068927010199,-62.0545179709986,
-8.4016402675109));
#38342=CARTESIAN_POINT('Ctrl Pts',(-7.27603390513785,-61.8795179709986,
-4.20082013374671));
#38343=CARTESIAN_POINT('Ctrl Pts',(-9.70137854017372,-61.7045179709986,
1.74701493417668E-11));
#38344=CARTESIAN_POINT('Ctrl Pts',(-7.27603390512272,-61.5295179709986,
4.20082013377292));
#38345=CARTESIAN_POINT('Ctrl Pts',(-4.85068927007173,-61.3545179709986,
8.40164026752836));
#38346=CARTESIAN_POINT('Ctrl Pts',(1.5129078685785E-11,-61.1795179709986,
8.40164026751963));
#38347=CARTESIAN_POINT('Ctrl Pts',(4.85068927010198,-61.0045179709986,8.4016402675109));
#38348=CARTESIAN_POINT('Ctrl Pts',(7.27603390513785,-60.8295179709986,4.20082013374672));
#38349=CARTESIAN_POINT('Ctrl Pts',(9.70137854017372,-60.6545179709986,-1.74689612655491E-11));
#38350=CARTESIAN_POINT('Ctrl Pts',(7.27603390512273,-60.4795179709986,-4.20082013377291));
#38351=CARTESIAN_POINT('Ctrl Pts',(4.85068927007173,-60.3045179709986,-8.40164026752836));
#38352=CARTESIAN_POINT('Ctrl Pts',(-1.51301075899711E-11,-60.1295179709986,
-8.40164026751963));
#38353=CARTESIAN_POINT('Ctrl Pts',(-4.85068927010199,-59.9545179709986,
-8.4016402675109));
#38354=CARTESIAN_POINT('Ctrl Pts',(-7.27603390513785,-59.7795179709986,
-4.20082013374671));
#38355=CARTESIAN_POINT('Ctrl Pts',(-9.70137854017372,-59.6045179709986,
1.74701493417668E-11));
#38356=CARTESIAN_POINT('Ctrl Pts',(-7.27603390512272,-59.4295179709986,
4.20082013377292));
#38357=CARTESIAN_POINT('Ctrl Pts',(-4.85068927007173,-59.2545179709986,
8.40164026752836));
#38358=CARTESIAN_POINT('Ctrl Pts',(1.5129078685785E-11,-59.0795179709986,
8.40164026751963));
#38359=CARTESIAN_POINT('Ctrl Pts',(4.85068927010198,-58.9045179709986,8.4016402675109));
#38360=CARTESIAN_POINT('Ctrl Pts',(7.27603390513785,-58.7295179709986,4.20082013374672));
#38361=CARTESIAN_POINT('Ctrl Pts',(9.70137854017372,-58.5545179709986,-1.74689612655491E-11));
#38362=CARTESIAN_POINT('Ctrl Pts',(7.27603390512273,-58.3795179709986,-4.20082013377291));
#38363=CARTESIAN_POINT('Ctrl Pts',(4.85068927007173,-58.2045179709986,-8.40164026752836));
#38364=CARTESIAN_POINT('Ctrl Pts',(-1.51301075899711E-11,-58.0295179709986,
-8.40164026751963));
#38365=CARTESIAN_POINT('Ctrl Pts',(-4.85068927010199,-57.8545179709986,
-8.4016402675109));
#38366=CARTESIAN_POINT('Ctrl Pts',(-7.27603390513785,-57.6795179709986,
-4.20082013374671));
#38367=CARTESIAN_POINT('Ctrl Pts',(-9.70137854017372,-57.5045179709986,
1.74701493417668E-11));
#38368=CARTESIAN_POINT('Ctrl Pts',(-7.27603390512272,-57.3295179709986,
4.20082013377292));
#38369=CARTESIAN_POINT('Ctrl Pts',(-4.85068927007173,-57.1545179709986,
8.40164026752836));
#38370=CARTESIAN_POINT('Ctrl Pts',(1.5129078685785E-11,-56.9795179709986,
8.40164026751963));
#38371=CARTESIAN_POINT('Ctrl Pts',(4.85068927010198,-56.8045179709986,8.4016402675109));
#38372=CARTESIAN_POINT('Ctrl Pts',(7.27603390513785,-56.6295179709986,4.20082013374672));
#38373=CARTESIAN_POINT('Ctrl Pts',(9.70137854017372,-56.4545179709986,-1.74689612655491E-11));
#38374=CARTESIAN_POINT('Ctrl Pts',(7.27603390512273,-56.2795179709986,-4.20082013377291));
#38375=CARTESIAN_POINT('Ctrl Pts',(4.85068927007173,-56.1045179709986,-8.40164026752836));
#38376=CARTESIAN_POINT('Ctrl Pts',(-1.51301075899711E-11,-55.9295179709986,
-8.40164026751963));
#38377=CARTESIAN_POINT('Ctrl Pts',(-4.85068927010199,-55.7545179709987,
-8.4016402675109));
#38378=CARTESIAN_POINT('Ctrl Pts',(-7.27603390513785,-55.5795179709986,
-4.20082013374671));
#38379=CARTESIAN_POINT('Ctrl Pts',(-9.70137854017372,-55.4045179709986,
1.74701493417668E-11));
#38380=CARTESIAN_POINT('Ctrl Pts',(-7.27603390512272,-55.2295179709986,
4.20082013377292));
#38381=CARTESIAN_POINT('Ctrl Pts',(-4.85068927007173,-55.0545179709987,
8.40164026752836));
#38382=CARTESIAN_POINT('Ctrl Pts',(1.5129078685785E-11,-54.8795179709986,
8.40164026751963));
#38383=CARTESIAN_POINT('Ctrl Pts',(4.85068927010198,-54.7045179709987,8.4016402675109));
#38384=CARTESIAN_POINT('Ctrl Pts',(7.27603390513785,-54.5295179709986,4.20082013374672));
#38385=CARTESIAN_POINT('Ctrl Pts',(9.70137854017372,-54.3545179709986,-1.74689612655491E-11));
#38386=CARTESIAN_POINT('Ctrl Pts',(7.27603390512273,-54.1795179709986,-4.20082013377291));
#38387=CARTESIAN_POINT('Ctrl Pts',(4.85068927007173,-54.0045179709987,-8.40164026752836));
#38388=CARTESIAN_POINT('Ctrl Pts',(-1.51301075899711E-11,-53.8295179709986,
-8.40164026751963));
#38389=CARTESIAN_POINT('Ctrl Pts',(-4.85068927010199,-53.6545179709986,
-8.4016402675109));
#38390=CARTESIAN_POINT('Ctrl Pts',(-7.27603390513785,-53.4795179709987,
-4.20082013374671));
#38391=CARTESIAN_POINT('Ctrl Pts',(-9.70137854017372,-53.3045179709987,
1.74701493417668E-11));
#38392=CARTESIAN_POINT('Ctrl Pts',(-7.27603390512272,-53.1295179709986,
4.20082013377292));
#38393=CARTESIAN_POINT('Ctrl Pts',(-4.85068927007173,-52.9545179709987,
8.40164026752836));
#38394=CARTESIAN_POINT('Ctrl Pts',(1.5129078685785E-11,-52.7795179709986,
8.40164026751963));
#38395=CARTESIAN_POINT('Ctrl Pts',(4.85068927010198,-52.6045179709986,8.4016402675109));
#38396=CARTESIAN_POINT('Ctrl Pts',(7.27603390513785,-52.4295179709987,4.20082013374672));
#38397=CARTESIAN_POINT('Ctrl Pts',(9.70137854017372,-52.2545179709986,-1.74689612655491E-11));
#38398=CARTESIAN_POINT('Ctrl Pts',(7.27603390512273,-52.0795179709986,-4.20082013377291));
#38399=CARTESIAN_POINT('Ctrl Pts',(4.85068927007173,-51.9045179709987,-8.40164026752836));
#38400=CARTESIAN_POINT('Ctrl Pts',(-1.51301075899711E-11,-51.7295179709986,
-8.40164026751963));
#38401=CARTESIAN_POINT('Ctrl Pts',(-4.85068927010199,-51.5545179709986,
-8.4016402675109));
#38402=CARTESIAN_POINT('Ctrl Pts',(-7.27603390513785,-51.3795179709987,
-4.20082013374671));
#38403=CARTESIAN_POINT('Ctrl Pts',(-9.70137854017372,-51.2045179709987,
1.74701493417668E-11));
#38404=CARTESIAN_POINT('Ctrl Pts',(-7.27603390512272,-51.0295179709986,
4.20082013377292));
#38405=CARTESIAN_POINT('Ctrl Pts',(-4.85068927007173,-50.8545179709987,
8.40164026752836));
#38406=CARTESIAN_POINT('Ctrl Pts',(1.5129078685785E-11,-50.6795179709987,
8.40164026751963));
#38407=CARTESIAN_POINT('Ctrl Pts',(4.85068927010198,-50.5045179709986,8.4016402675109));
#38408=CARTESIAN_POINT('Ctrl Pts',(7.27603390513785,-50.3295179709987,4.20082013374672));
#38409=CARTESIAN_POINT('Ctrl Pts',(9.70137854017372,-50.1545179709987,-1.74689612655491E-11));
#38410=CARTESIAN_POINT('Ctrl Pts',(7.27603390512273,-49.9795179709986,-4.20082013377291));
#38411=CARTESIAN_POINT('Ctrl Pts',(4.85068927007173,-49.8045179709986,-8.40164026752836));
#38412=CARTESIAN_POINT('Ctrl Pts',(-1.51301075899711E-11,-49.6295179709987,
-8.40164026751963));
#38413=CARTESIAN_POINT('Ctrl Pts',(-4.85068927010199,-49.4545179709986,
-8.4016402675109));
#38414=CARTESIAN_POINT('Ctrl Pts',(-7.27603390513785,-49.2795179709986,
-4.20082013374671));
#38415=CARTESIAN_POINT('Ctrl Pts',(-9.70137854017372,-49.1045179709987,
1.74701493417668E-11));
#38416=CARTESIAN_POINT('Ctrl Pts',(-7.27603390512272,-48.9295179709987,
4.20082013377292));
#38417=CARTESIAN_POINT('Ctrl Pts',(-4.85068927007173,-48.7545179709986,
8.40164026752836));
#38418=CARTESIAN_POINT('Ctrl Pts',(1.5129078685785E-11,-48.5795179709987,
8.40164026751963));
#38419=CARTESIAN_POINT('Ctrl Pts',(4.85068927010198,-48.4045179709987,8.4016402675109));
#38420=CARTESIAN_POINT('Ctrl Pts',(7.27603390513785,-48.2295179709986,4.20082013374672));
#38421=CARTESIAN_POINT('Ctrl Pts',(9.70137854017372,-48.0545179709987,-1.74689612655491E-11));
#38422=CARTESIAN_POINT('Ctrl Pts',(7.27603390512273,-47.8795179709987,-4.20082013377291));
#38423=CARTESIAN_POINT('Ctrl Pts',(4.85068927007173,-47.7045179709986,-8.40164026752836));
#38424=CARTESIAN_POINT('Ctrl Pts',(-1.51301075899711E-11,-47.5295179709987,
-8.40164026751963));
#38425=CARTESIAN_POINT('Ctrl Pts',(-4.85068927010199,-47.3545179709987,
-8.4016402675109));
#38426=CARTESIAN_POINT('Ctrl Pts',(-7.27603390513785,-47.1795179709986,
-4.20082013374671));
#38427=CARTESIAN_POINT('Ctrl Pts',(-9.70137854017372,-47.0045179709987,
1.74701493417668E-11));
#38428=CARTESIAN_POINT('Ctrl Pts',(-7.27603390512272,-46.8295179709987,
4.20082013377292));
#38429=CARTESIAN_POINT('Ctrl Pts',(-4.85068927007173,-46.6545179709987,
8.40164026752836));
#38430=CARTESIAN_POINT('Ctrl Pts',(1.5129078685785E-11,-46.4795179709987,
8.40164026751963));
#38431=CARTESIAN_POINT('Ctrl Pts',(4.85068927010198,-46.3045179709987,8.4016402675109));
#38432=CARTESIAN_POINT('Ctrl Pts',(7.27603390513785,-46.1295179709986,4.20082013374672));
#38433=CARTESIAN_POINT('Ctrl Pts',(9.70137854017372,-45.9545179709987,-1.74689612655491E-11));
#38434=CARTESIAN_POINT('Ctrl Pts',(7.27603390512273,-45.7795179709987,-4.20082013377291));
#38435=CARTESIAN_POINT('Ctrl Pts',(4.85068927007173,-45.6045179709986,-8.40164026752836));
#38436=CARTESIAN_POINT('Ctrl Pts',(-1.51301075899711E-11,-45.4295179709987,
-8.40164026751963));
#38437=CARTESIAN_POINT('Ctrl Pts',(-4.85068927010199,-45.2545179709987,
-8.4016402675109));
#38438=CARTESIAN_POINT('Ctrl Pts',(-7.27603390513785,-45.0795179709987,
-4.20082013374671));
#38439=CARTESIAN_POINT('Ctrl Pts',(-9.70137854017372,-44.9045179709986,
1.74701493417668E-11));
#38440=CARTESIAN_POINT('Ctrl Pts',(-7.27603390512272,-44.7295179709987,
4.20082013377292));
#38441=CARTESIAN_POINT('Ctrl Pts',(-4.85068927007173,-44.5545179709987,
8.40164026752836));
#38442=CARTESIAN_POINT('Ctrl Pts',(1.5129078685785E-11,-44.3795179709986,
8.40164026751963));
#38443=CARTESIAN_POINT('Ctrl Pts',(4.85068927010198,-44.2045179709987,8.4016402675109));
#38444=CARTESIAN_POINT('Ctrl Pts',(7.27603390513785,-44.0295179709987,4.20082013374672));
#38445=CARTESIAN_POINT('Ctrl Pts',(9.70137854017372,-43.8545179709986,-1.74689612655491E-11));
#38446=CARTESIAN_POINT('Ctrl Pts',(7.27603390512273,-43.6795179709987,-4.20082013377291));
#38447=CARTESIAN_POINT('Ctrl Pts',(4.85068927007173,-43.5045179709987,-8.40164026752836));
#38448=CARTESIAN_POINT('Ctrl Pts',(-1.51301075899711E-11,-43.3295179709987,
-8.40164026751963));
#38449=CARTESIAN_POINT('Ctrl Pts',(-1.78726082715848E-11,-212.63675111262,
-9.92453123331945));
#38450=CARTESIAN_POINT('Ctrl Pts',(-5.7299307791557,-212.46175111262,-9.92453123330913));
#38451=CARTESIAN_POINT('Ctrl Pts',(-8.59489616871569,-212.28675111262,-4.96226561664425));
#38452=CARTESIAN_POINT('Ctrl Pts',(-11.4598615582757,-212.11175111262,2.06368086793017E-11));
#38453=CARTESIAN_POINT('Ctrl Pts',(-8.59489616869782,-211.93675111262,4.9622656166752));
#38454=CARTESIAN_POINT('Ctrl Pts',(-5.72993077911996,-211.76175111262,9.92453123332977));
#38455=CARTESIAN_POINT('Ctrl Pts',(1.7871392867044E-11,-211.58675111262,
9.92453123331945));
#38456=CARTESIAN_POINT('Ctrl Pts',(5.7299307791557,-211.41175111262,9.92453123330913));
#38457=CARTESIAN_POINT('Ctrl Pts',(8.59489616871569,-211.23675111262,4.96226561664425));
#38458=CARTESIAN_POINT('Ctrl Pts',(11.4598615582757,-211.06175111262,-2.06354052510241E-11));
#38459=CARTESIAN_POINT('Ctrl Pts',(8.59489616869782,-210.88675111262,-4.9622656166752));
#38460=CARTESIAN_POINT('Ctrl Pts',(5.72993077911996,-210.71175111262,-9.92453123332976));
#38461=CARTESIAN_POINT('Ctrl Pts',(-1.78726082715848E-11,-210.53675111262,
-9.92453123331945));
#38462=CARTESIAN_POINT('Ctrl Pts',(-5.7299307791557,-210.36175111262,-9.92453123330913));
#38463=CARTESIAN_POINT('Ctrl Pts',(-8.59489616871569,-210.18675111262,-4.96226561664425));
#38464=CARTESIAN_POINT('Ctrl Pts',(-11.4598615582757,-210.01175111262,2.06368086793017E-11));
#38465=CARTESIAN_POINT('Ctrl Pts',(-8.59489616869782,-209.83675111262,4.9622656166752));
#38466=CARTESIAN_POINT('Ctrl Pts',(-5.72993077911996,-209.66175111262,9.92453123332977));
#38467=CARTESIAN_POINT('Ctrl Pts',(1.7871392867044E-11,-209.48675111262,
9.92453123331945));
#38468=CARTESIAN_POINT('Ctrl Pts',(5.7299307791557,-209.31175111262,9.92453123330913));
#38469=CARTESIAN_POINT('Ctrl Pts',(8.59489616871569,-209.13675111262,4.96226561664425));
#38470=CARTESIAN_POINT('Ctrl Pts',(11.4598615582757,-208.96175111262,-2.06354052510241E-11));
#38471=CARTESIAN_POINT('Ctrl Pts',(8.59489616869782,-208.78675111262,-4.9622656166752));
#38472=CARTESIAN_POINT('Ctrl Pts',(5.72993077911996,-208.61175111262,-9.92453123332976));
#38473=CARTESIAN_POINT('Ctrl Pts',(-1.78726082715848E-11,-208.43675111262,
-9.92453123331945));
#38474=CARTESIAN_POINT('Ctrl Pts',(-5.7299307791557,-208.26175111262,-9.92453123330913));
#38475=CARTESIAN_POINT('Ctrl Pts',(-8.59489616871569,-208.08675111262,-4.96226561664425));
#38476=CARTESIAN_POINT('Ctrl Pts',(-11.4598615582757,-207.91175111262,2.06368086793017E-11));
#38477=CARTESIAN_POINT('Ctrl Pts',(-8.59489616869782,-207.73675111262,4.9622656166752));
#38478=CARTESIAN_POINT('Ctrl Pts',(-5.72993077911996,-207.56175111262,9.92453123332977));
#38479=CARTESIAN_POINT('Ctrl Pts',(1.7871392867044E-11,-207.38675111262,
9.92453123331945));
#38480=CARTESIAN_POINT('Ctrl Pts',(5.7299307791557,-207.21175111262,9.92453123330913));
#38481=CARTESIAN_POINT('Ctrl Pts',(8.59489616871569,-207.03675111262,4.96226561664425));
#38482=CARTESIAN_POINT('Ctrl Pts',(11.4598615582757,-206.86175111262,-2.06354052510241E-11));
#38483=CARTESIAN_POINT('Ctrl Pts',(8.59489616869782,-206.68675111262,-4.9622656166752));
#38484=CARTESIAN_POINT('Ctrl Pts',(5.72993077911996,-206.51175111262,-9.92453123332976));
#38485=CARTESIAN_POINT('Ctrl Pts',(-1.78726082715848E-11,-206.33675111262,
-9.92453123331945));
#38486=CARTESIAN_POINT('Ctrl Pts',(-5.7299307791557,-206.16175111262,-9.92453123330913));
#38487=CARTESIAN_POINT('Ctrl Pts',(-8.59489616871569,-205.98675111262,-4.96226561664425));
#38488=CARTESIAN_POINT('Ctrl Pts',(-11.4598615582757,-205.81175111262,2.06368086793017E-11));
#38489=CARTESIAN_POINT('Ctrl Pts',(-8.59489616869782,-205.63675111262,4.9622656166752));
#38490=CARTESIAN_POINT('Ctrl Pts',(-5.72993077911996,-205.46175111262,9.92453123332977));
#38491=CARTESIAN_POINT('Ctrl Pts',(1.7871392867044E-11,-205.28675111262,
9.92453123331945));
#38492=CARTESIAN_POINT('Ctrl Pts',(5.7299307791557,-205.11175111262,9.92453123330913));
#38493=CARTESIAN_POINT('Ctrl Pts',(8.59489616871569,-204.93675111262,4.96226561664425));
#38494=CARTESIAN_POINT('Ctrl Pts',(11.4598615582757,-204.76175111262,-2.06354052510241E-11));
#38495=CARTESIAN_POINT('Ctrl Pts',(8.59489616869782,-204.58675111262,-4.9622656166752));
#38496=CARTESIAN_POINT('Ctrl Pts',(5.72993077911996,-204.41175111262,-9.92453123332976));
#38497=CARTESIAN_POINT('Ctrl Pts',(-1.78726082715848E-11,-204.23675111262,
-9.92453123331945));
#38498=CARTESIAN_POINT('Ctrl Pts',(-5.7299307791557,-204.06175111262,-9.92453123330913));
#38499=CARTESIAN_POINT('Ctrl Pts',(-8.59489616871569,-203.88675111262,-4.96226561664425));
#38500=CARTESIAN_POINT('Ctrl Pts',(-11.4598615582757,-203.71175111262,2.06368086793017E-11));
#38501=CARTESIAN_POINT('Ctrl Pts',(-8.59489616869782,-203.53675111262,4.9622656166752));
#38502=CARTESIAN_POINT('Ctrl Pts',(-5.72993077911996,-203.36175111262,9.92453123332977));
#38503=CARTESIAN_POINT('Ctrl Pts',(1.7871392867044E-11,-203.18675111262,
9.92453123331945));
#38504=CARTESIAN_POINT('Ctrl Pts',(5.7299307791557,-203.01175111262,9.92453123330913));
#38505=CARTESIAN_POINT('Ctrl Pts',(8.59489616871569,-202.83675111262,4.96226561664425));
#38506=CARTESIAN_POINT('Ctrl Pts',(11.4598615582757,-202.66175111262,-2.06354052510241E-11));
#38507=CARTESIAN_POINT('Ctrl Pts',(8.59489616869782,-202.48675111262,-4.9622656166752));
#38508=CARTESIAN_POINT('Ctrl Pts',(5.72993077911996,-202.31175111262,-9.92453123332976));
#38509=CARTESIAN_POINT('Ctrl Pts',(-1.78726082715848E-11,-202.13675111262,
-9.92453123331945));
#38510=CARTESIAN_POINT('Ctrl Pts',(-5.7299307791557,-201.96175111262,-9.92453123330913));
#38511=CARTESIAN_POINT('Ctrl Pts',(-8.59489616871569,-201.78675111262,-4.96226561664425));
#38512=CARTESIAN_POINT('Ctrl Pts',(-11.4598615582757,-201.61175111262,2.06368086793017E-11));
#38513=CARTESIAN_POINT('Ctrl Pts',(-8.59489616869782,-201.43675111262,4.9622656166752));
#38514=CARTESIAN_POINT('Ctrl Pts',(-5.72993077911996,-201.26175111262,9.92453123332977));
#38515=CARTESIAN_POINT('Ctrl Pts',(1.7871392867044E-11,-201.08675111262,
9.92453123331945));
#38516=CARTESIAN_POINT('Ctrl Pts',(5.7299307791557,-200.91175111262,9.92453123330913));
#38517=CARTESIAN_POINT('Ctrl Pts',(8.59489616871569,-200.73675111262,4.96226561664425));
#38518=CARTESIAN_POINT('Ctrl Pts',(11.4598615582757,-200.56175111262,-2.06354052510241E-11));
#38519=CARTESIAN_POINT('Ctrl Pts',(8.59489616869782,-200.38675111262,-4.9622656166752));
#38520=CARTESIAN_POINT('Ctrl Pts',(5.72993077911996,-200.21175111262,-9.92453123332976));
#38521=CARTESIAN_POINT('Ctrl Pts',(-1.78726082715848E-11,-200.03675111262,
-9.92453123331945));
#38522=CARTESIAN_POINT('Ctrl Pts',(-5.7299307791557,-199.86175111262,-9.92453123330913));
#38523=CARTESIAN_POINT('Ctrl Pts',(-8.59489616871569,-199.68675111262,-4.96226561664425));
#38524=CARTESIAN_POINT('Ctrl Pts',(-11.4598615582757,-199.51175111262,2.06368086793017E-11));
#38525=CARTESIAN_POINT('Ctrl Pts',(-8.59489616869782,-199.33675111262,4.9622656166752));
#38526=CARTESIAN_POINT('Ctrl Pts',(-5.72993077911996,-199.16175111262,9.92453123332977));
#38527=CARTESIAN_POINT('Ctrl Pts',(1.7871392867044E-11,-198.98675111262,
9.92453123331945));
#38528=CARTESIAN_POINT('Ctrl Pts',(5.7299307791557,-198.81175111262,9.92453123330913));
#38529=CARTESIAN_POINT('Ctrl Pts',(8.59489616871569,-198.63675111262,4.96226561664425));
#38530=CARTESIAN_POINT('Ctrl Pts',(11.4598615582757,-198.46175111262,-2.06354052510241E-11));
#38531=CARTESIAN_POINT('Ctrl Pts',(8.59489616869782,-198.28675111262,-4.9622656166752));
#38532=CARTESIAN_POINT('Ctrl Pts',(5.72993077911996,-198.11175111262,-9.92453123332976));
#38533=CARTESIAN_POINT('Ctrl Pts',(-1.78726082715848E-11,-197.93675111262,
-9.92453123331945));
#38534=CARTESIAN_POINT('Ctrl Pts',(-5.7299307791557,-197.76175111262,-9.92453123330913));
#38535=CARTESIAN_POINT('Ctrl Pts',(-8.59489616871569,-197.58675111262,-4.96226561664425));
#38536=CARTESIAN_POINT('Ctrl Pts',(-11.4598615582757,-197.41175111262,2.06368086793017E-11));
#38537=CARTESIAN_POINT('Ctrl Pts',(-8.59489616869782,-197.23675111262,4.9622656166752));
#38538=CARTESIAN_POINT('Ctrl Pts',(-5.72993077911996,-197.06175111262,9.92453123332977));
#38539=CARTESIAN_POINT('Ctrl Pts',(1.7871392867044E-11,-196.88675111262,
9.92453123331945));
#38540=CARTESIAN_POINT('Ctrl Pts',(5.7299307791557,-196.71175111262,9.92453123330913));
#38541=CARTESIAN_POINT('Ctrl Pts',(8.59489616871569,-196.53675111262,4.96226561664425));
#38542=CARTESIAN_POINT('Ctrl Pts',(11.4598615582757,-196.36175111262,-2.06354052510241E-11));
#38543=CARTESIAN_POINT('Ctrl Pts',(8.59489616869782,-196.18675111262,-4.9622656166752));
#38544=CARTESIAN_POINT('Ctrl Pts',(5.72993077911996,-196.01175111262,-9.92453123332976));
#38545=CARTESIAN_POINT('Ctrl Pts',(-1.78726082715848E-11,-195.83675111262,
-9.92453123331945));
#38546=CARTESIAN_POINT('Ctrl Pts',(-5.7299307791557,-195.66175111262,-9.92453123330913));
#38547=CARTESIAN_POINT('Ctrl Pts',(-8.59489616871569,-195.48675111262,-4.96226561664425));
#38548=CARTESIAN_POINT('Ctrl Pts',(-11.4598615582757,-195.31175111262,2.06368086793017E-11));
#38549=CARTESIAN_POINT('Ctrl Pts',(-8.59489616869782,-195.13675111262,4.9622656166752));
#38550=CARTESIAN_POINT('Ctrl Pts',(-5.72993077911996,-194.96175111262,9.92453123332977));
#38551=CARTESIAN_POINT('Ctrl Pts',(1.7871392867044E-11,-194.78675111262,
9.92453123331945));
#38552=CARTESIAN_POINT('Ctrl Pts',(5.7299307791557,-194.61175111262,9.92453123330913));
#38553=CARTESIAN_POINT('Ctrl Pts',(8.59489616871569,-194.43675111262,4.96226561664425));
#38554=CARTESIAN_POINT('Ctrl Pts',(11.4598615582757,-194.26175111262,-2.06354052510241E-11));
#38555=CARTESIAN_POINT('Ctrl Pts',(8.59489616869782,-194.08675111262,-4.9622656166752));
#38556=CARTESIAN_POINT('Ctrl Pts',(5.72993077911996,-193.91175111262,-9.92453123332976));
#38557=CARTESIAN_POINT('Ctrl Pts',(-1.78726082715848E-11,-193.73675111262,
-9.92453123331945));
#38558=CARTESIAN_POINT('Ctrl Pts',(-5.7299307791557,-193.56175111262,-9.92453123330913));
#38559=CARTESIAN_POINT('Ctrl Pts',(-8.59489616871569,-193.38675111262,-4.96226561664425));
#38560=CARTESIAN_POINT('Ctrl Pts',(-11.4598615582757,-193.21175111262,2.06368086793017E-11));
#38561=CARTESIAN_POINT('Ctrl Pts',(-8.59489616869782,-193.03675111262,4.9622656166752));
#38562=CARTESIAN_POINT('Ctrl Pts',(-5.72993077911996,-192.86175111262,9.92453123332977));
#38563=CARTESIAN_POINT('Ctrl Pts',(1.7871392867044E-11,-192.68675111262,
9.92453123331945));
#38564=CARTESIAN_POINT('Ctrl Pts',(5.7299307791557,-192.51175111262,9.92453123330913));
#38565=CARTESIAN_POINT('Ctrl Pts',(8.59489616871569,-192.33675111262,4.96226561664425));
#38566=CARTESIAN_POINT('Ctrl Pts',(11.4598615582757,-192.16175111262,-2.06354052510241E-11));
#38567=CARTESIAN_POINT('Ctrl Pts',(8.59489616869782,-191.98675111262,-4.9622656166752));
#38568=CARTESIAN_POINT('Ctrl Pts',(5.72993077911996,-191.81175111262,-9.92453123332976));
#38569=CARTESIAN_POINT('Ctrl Pts',(-1.78726082715848E-11,-191.63675111262,
-9.92453123331945));
#38570=CARTESIAN_POINT('Ctrl Pts',(-5.7299307791557,-191.46175111262,-9.92453123330913));
#38571=CARTESIAN_POINT('Ctrl Pts',(-8.59489616871569,-191.28675111262,-4.96226561664425));
#38572=CARTESIAN_POINT('Ctrl Pts',(-11.4598615582757,-191.11175111262,2.06368086793017E-11));
#38573=CARTESIAN_POINT('Ctrl Pts',(-8.59489616869782,-190.93675111262,4.9622656166752));
#38574=CARTESIAN_POINT('Ctrl Pts',(-5.72993077911996,-190.76175111262,9.92453123332977));
#38575=CARTESIAN_POINT('Ctrl Pts',(1.7871392867044E-11,-190.58675111262,
9.92453123331945));
#38576=CARTESIAN_POINT('Ctrl Pts',(5.7299307791557,-190.41175111262,9.92453123330913));
#38577=CARTESIAN_POINT('Ctrl Pts',(8.59489616871569,-190.23675111262,4.96226561664425));
#38578=CARTESIAN_POINT('Ctrl Pts',(11.4598615582757,-190.06175111262,-2.06354052510241E-11));
#38579=CARTESIAN_POINT('Ctrl Pts',(8.59489616869782,-189.88675111262,-4.9622656166752));
#38580=CARTESIAN_POINT('Ctrl Pts',(5.72993077911996,-189.71175111262,-9.92453123332976));
#38581=CARTESIAN_POINT('Ctrl Pts',(-1.78726082715848E-11,-189.53675111262,
-9.92453123331945));
#38582=CARTESIAN_POINT('Ctrl Pts',(-5.7299307791557,-189.36175111262,-9.92453123330913));
#38583=CARTESIAN_POINT('Ctrl Pts',(-8.59489616871569,-189.18675111262,-4.96226561664425));
#38584=CARTESIAN_POINT('Ctrl Pts',(-11.4598615582757,-189.01175111262,2.06368086793017E-11));
#38585=CARTESIAN_POINT('Ctrl Pts',(-8.59489616869782,-188.83675111262,4.9622656166752));
#38586=CARTESIAN_POINT('Ctrl Pts',(-5.72993077911996,-188.66175111262,9.92453123332977));
#38587=CARTESIAN_POINT('Ctrl Pts',(1.7871392867044E-11,-188.48675111262,
9.92453123331945));
#38588=CARTESIAN_POINT('Ctrl Pts',(5.7299307791557,-188.31175111262,9.92453123330913));
#38589=CARTESIAN_POINT('Ctrl Pts',(8.59489616871569,-188.13675111262,4.96226561664425));
#38590=CARTESIAN_POINT('Ctrl Pts',(11.4598615582757,-187.96175111262,-2.06354052510241E-11));
#38591=CARTESIAN_POINT('Ctrl Pts',(8.59489616869782,-187.78675111262,-4.9622656166752));
#38592=CARTESIAN_POINT('Ctrl Pts',(5.72993077911996,-187.61175111262,-9.92453123332976));
#38593=CARTESIAN_POINT('Ctrl Pts',(-1.78726082715848E-11,-187.43675111262,
-9.92453123331945));
#38594=CARTESIAN_POINT('Ctrl Pts',(-5.7299307791557,-187.26175111262,-9.92453123330913));
#38595=CARTESIAN_POINT('Ctrl Pts',(-8.59489616871569,-187.08675111262,-4.96226561664425));
#38596=CARTESIAN_POINT('Ctrl Pts',(-11.4598615582757,-186.91175111262,2.06368086793017E-11));
#38597=CARTESIAN_POINT('Ctrl Pts',(-8.59489616869782,-186.73675111262,4.9622656166752));
#38598=CARTESIAN_POINT('Ctrl Pts',(-5.72993077911996,-186.56175111262,9.92453123332977));
#38599=CARTESIAN_POINT('Ctrl Pts',(1.7871392867044E-11,-186.38675111262,
9.92453123331945));
#38600=CARTESIAN_POINT('Ctrl Pts',(5.7299307791557,-186.21175111262,9.92453123330913));
#38601=CARTESIAN_POINT('Ctrl Pts',(8.59489616871569,-186.03675111262,4.96226561664425));
#38602=CARTESIAN_POINT('Ctrl Pts',(11.4598615582757,-185.86175111262,-2.06354052510241E-11));
#38603=CARTESIAN_POINT('Ctrl Pts',(8.59489616869782,-185.68675111262,-4.9622656166752));
#38604=CARTESIAN_POINT('Ctrl Pts',(5.72993077911996,-185.51175111262,-9.92453123332976));
#38605=CARTESIAN_POINT('Ctrl Pts',(-1.78726082715848E-11,-185.33675111262,
-9.92453123331945));
#38606=CARTESIAN_POINT('Ctrl Pts',(-5.7299307791557,-185.16175111262,-9.92453123330913));
#38607=CARTESIAN_POINT('Ctrl Pts',(-8.59489616871569,-184.98675111262,-4.96226561664425));
#38608=CARTESIAN_POINT('Ctrl Pts',(-11.4598615582757,-184.81175111262,2.06368086793017E-11));
#38609=CARTESIAN_POINT('Ctrl Pts',(-8.59489616869782,-184.63675111262,4.9622656166752));
#38610=CARTESIAN_POINT('Ctrl Pts',(-5.72993077911996,-184.46175111262,9.92453123332977));
#38611=CARTESIAN_POINT('Ctrl Pts',(1.7871392867044E-11,-184.28675111262,
9.92453123331945));
#38612=CARTESIAN_POINT('Ctrl Pts',(5.7299307791557,-184.11175111262,9.92453123330913));
#38613=CARTESIAN_POINT('Ctrl Pts',(8.59489616871569,-183.93675111262,4.96226561664425));
#38614=CARTESIAN_POINT('Ctrl Pts',(11.4598615582757,-183.76175111262,-2.06354052510241E-11));
#38615=CARTESIAN_POINT('Ctrl Pts',(8.59489616869782,-183.58675111262,-4.9622656166752));
#38616=CARTESIAN_POINT('Ctrl Pts',(5.72993077911996,-183.41175111262,-9.92453123332976));
#38617=CARTESIAN_POINT('Ctrl Pts',(-1.78726082715848E-11,-183.23675111262,
-9.92453123331945));
#38618=CARTESIAN_POINT('Ctrl Pts',(-5.7299307791557,-183.06175111262,-9.92453123330913));
#38619=CARTESIAN_POINT('Ctrl Pts',(-8.59489616871569,-182.88675111262,-4.96226561664425));
#38620=CARTESIAN_POINT('Ctrl Pts',(-11.4598615582757,-182.71175111262,2.06368086793017E-11));
#38621=CARTESIAN_POINT('Ctrl Pts',(-8.59489616869782,-182.53675111262,4.9622656166752));
#38622=CARTESIAN_POINT('Ctrl Pts',(-5.72993077911996,-182.36175111262,9.92453123332977));
#38623=CARTESIAN_POINT('Ctrl Pts',(1.7871392867044E-11,-182.18675111262,
9.92453123331945));
#38624=CARTESIAN_POINT('Ctrl Pts',(5.7299307791557,-182.01175111262,9.92453123330913));
#38625=CARTESIAN_POINT('Ctrl Pts',(8.59489616871569,-181.83675111262,4.96226561664425));
#38626=CARTESIAN_POINT('Ctrl Pts',(11.4598615582757,-181.66175111262,-2.06354052510241E-11));
#38627=CARTESIAN_POINT('Ctrl Pts',(8.59489616869782,-181.48675111262,-4.9622656166752));
#38628=CARTESIAN_POINT('Ctrl Pts',(5.72993077911996,-181.31175111262,-9.92453123332976));
#38629=CARTESIAN_POINT('Ctrl Pts',(-1.78726082715848E-11,-181.13675111262,
-9.92453123331945));
#38630=CARTESIAN_POINT('Ctrl Pts',(-5.7299307791557,-180.96175111262,-9.92453123330913));
#38631=CARTESIAN_POINT('Ctrl Pts',(-8.59489616871569,-180.78675111262,-4.96226561664425));
#38632=CARTESIAN_POINT('Ctrl Pts',(-11.4598615582757,-180.61175111262,2.06368086793017E-11));
#38633=CARTESIAN_POINT('Ctrl Pts',(-8.59489616869782,-180.43675111262,4.9622656166752));
#38634=CARTESIAN_POINT('Ctrl Pts',(-5.72993077911996,-180.26175111262,9.92453123332977));
#38635=CARTESIAN_POINT('Ctrl Pts',(1.7871392867044E-11,-180.08675111262,
9.92453123331945));
#38636=CARTESIAN_POINT('Ctrl Pts',(5.7299307791557,-179.91175111262,9.92453123330913));
#38637=CARTESIAN_POINT('Ctrl Pts',(8.59489616871569,-179.73675111262,4.96226561664425));
#38638=CARTESIAN_POINT('Ctrl Pts',(11.4598615582757,-179.56175111262,-2.06354052510241E-11));
#38639=CARTESIAN_POINT('Ctrl Pts',(8.59489616869782,-179.38675111262,-4.9622656166752));
#38640=CARTESIAN_POINT('Ctrl Pts',(5.72993077911996,-179.21175111262,-9.92453123332976));
#38641=CARTESIAN_POINT('Ctrl Pts',(-1.78726082715848E-11,-179.03675111262,
-9.92453123331945));
#38642=CARTESIAN_POINT('Ctrl Pts',(-5.7299307791557,-178.86175111262,-9.92453123330913));
#38643=CARTESIAN_POINT('Ctrl Pts',(-8.59489616871569,-178.68675111262,-4.96226561664425));
#38644=CARTESIAN_POINT('Ctrl Pts',(-11.4598615582757,-178.51175111262,2.06368086793017E-11));
#38645=CARTESIAN_POINT('Ctrl Pts',(-8.59489616869782,-178.33675111262,4.9622656166752));
#38646=CARTESIAN_POINT('Ctrl Pts',(-5.72993077911996,-178.16175111262,9.92453123332977));
#38647=CARTESIAN_POINT('Ctrl Pts',(1.7871392867044E-11,-177.98675111262,
9.92453123331945));
#38648=CARTESIAN_POINT('Ctrl Pts',(5.7299307791557,-177.81175111262,9.92453123330913));
#38649=CARTESIAN_POINT('Ctrl Pts',(8.59489616871569,-177.63675111262,4.96226561664425));
#38650=CARTESIAN_POINT('Ctrl Pts',(11.4598615582757,-177.46175111262,-2.06354052510241E-11));
#38651=CARTESIAN_POINT('Ctrl Pts',(8.59489616869782,-177.28675111262,-4.9622656166752));
#38652=CARTESIAN_POINT('Ctrl Pts',(5.72993077911996,-177.11175111262,-9.92453123332976));
#38653=CARTESIAN_POINT('Ctrl Pts',(-1.78726082715848E-11,-176.93675111262,
-9.92453123331945));
#38654=CARTESIAN_POINT('Ctrl Pts',(-5.7299307791557,-176.76175111262,-9.92453123330913));
#38655=CARTESIAN_POINT('Ctrl Pts',(-8.59489616871569,-176.58675111262,-4.96226561664425));
#38656=CARTESIAN_POINT('Ctrl Pts',(-11.4598615582757,-176.41175111262,2.06368086793017E-11));
#38657=CARTESIAN_POINT('Ctrl Pts',(-8.59489616869782,-176.23675111262,4.9622656166752));
#38658=CARTESIAN_POINT('Ctrl Pts',(-5.72993077911996,-176.06175111262,9.92453123332977));
#38659=CARTESIAN_POINT('Ctrl Pts',(1.7871392867044E-11,-175.88675111262,
9.92453123331945));
#38660=CARTESIAN_POINT('Ctrl Pts',(5.7299307791557,-175.71175111262,9.92453123330913));
#38661=CARTESIAN_POINT('Ctrl Pts',(8.59489616871569,-175.53675111262,4.96226561664425));
#38662=CARTESIAN_POINT('Ctrl Pts',(11.4598615582757,-175.36175111262,-2.06354052510241E-11));
#38663=CARTESIAN_POINT('Ctrl Pts',(8.59489616869782,-175.18675111262,-4.9622656166752));
#38664=CARTESIAN_POINT('Ctrl Pts',(5.72993077911996,-175.01175111262,-9.92453123332976));
#38665=CARTESIAN_POINT('Ctrl Pts',(-1.78726082715848E-11,-174.83675111262,
-9.92453123331945));
#38666=CARTESIAN_POINT('Ctrl Pts',(-5.7299307791557,-174.66175111262,-9.92453123330913));
#38667=CARTESIAN_POINT('Ctrl Pts',(-8.59489616871569,-174.48675111262,-4.96226561664425));
#38668=CARTESIAN_POINT('Ctrl Pts',(-11.4598615582757,-174.31175111262,2.06368086793017E-11));
#38669=CARTESIAN_POINT('Ctrl Pts',(-8.59489616869782,-174.13675111262,4.9622656166752));
#38670=CARTESIAN_POINT('Ctrl Pts',(-5.72993077911996,-173.96175111262,9.92453123332977));
#38671=CARTESIAN_POINT('Ctrl Pts',(1.7871392867044E-11,-173.78675111262,
9.92453123331945));
#38672=CARTESIAN_POINT('Ctrl Pts',(5.7299307791557,-173.61175111262,9.92453123330913));
#38673=CARTESIAN_POINT('Ctrl Pts',(8.59489616871569,-173.43675111262,4.96226561664425));
#38674=CARTESIAN_POINT('Ctrl Pts',(11.4598615582757,-173.26175111262,-2.06354052510241E-11));
#38675=CARTESIAN_POINT('Ctrl Pts',(8.59489616869782,-173.08675111262,-4.9622656166752));
#38676=CARTESIAN_POINT('Ctrl Pts',(5.72993077911996,-172.91175111262,-9.92453123332976));
#38677=CARTESIAN_POINT('Ctrl Pts',(-1.78726082715848E-11,-172.73675111262,
-9.92453123331945));
#38678=CARTESIAN_POINT('Ctrl Pts',(-5.7299307791557,-172.56175111262,-9.92453123330913));
#38679=CARTESIAN_POINT('Ctrl Pts',(-8.59489616871569,-172.38675111262,-4.96226561664425));
#38680=CARTESIAN_POINT('Ctrl Pts',(-11.4598615582757,-172.21175111262,2.06368086793017E-11));
#38681=CARTESIAN_POINT('Ctrl Pts',(-8.59489616869782,-172.03675111262,4.9622656166752));
#38682=CARTESIAN_POINT('Ctrl Pts',(-5.72993077911996,-171.86175111262,9.92453123332977));
#38683=CARTESIAN_POINT('Ctrl Pts',(1.7871392867044E-11,-171.68675111262,
9.92453123331945));
#38684=CARTESIAN_POINT('Ctrl Pts',(5.7299307791557,-171.51175111262,9.92453123330913));
#38685=CARTESIAN_POINT('Ctrl Pts',(8.59489616871569,-171.33675111262,4.96226561664425));
#38686=CARTESIAN_POINT('Ctrl Pts',(11.4598615582757,-171.16175111262,-2.06354052510241E-11));
#38687=CARTESIAN_POINT('Ctrl Pts',(8.59489616869782,-170.98675111262,-4.9622656166752));
#38688=CARTESIAN_POINT('Ctrl Pts',(5.72993077911996,-170.81175111262,-9.92453123332976));
#38689=CARTESIAN_POINT('Ctrl Pts',(-1.78726082715848E-11,-170.63675111262,
-9.92453123331945));
#38690=CARTESIAN_POINT('Ctrl Pts',(-5.7299307791557,-170.46175111262,-9.92453123330913));
#38691=CARTESIAN_POINT('Ctrl Pts',(-8.59489616871569,-170.28675111262,-4.96226561664425));
#38692=CARTESIAN_POINT('Ctrl Pts',(-11.4598615582757,-170.11175111262,2.06368086793017E-11));
#38693=CARTESIAN_POINT('Ctrl Pts',(-8.59489616869782,-169.93675111262,4.9622656166752));
#38694=CARTESIAN_POINT('Ctrl Pts',(-5.72993077911996,-169.76175111262,9.92453123332977));
#38695=CARTESIAN_POINT('Ctrl Pts',(1.7871392867044E-11,-169.58675111262,
9.92453123331945));
#38696=CARTESIAN_POINT('Ctrl Pts',(5.7299307791557,-169.41175111262,9.92453123330913));
#38697=CARTESIAN_POINT('Ctrl Pts',(8.59489616871569,-169.23675111262,4.96226561664425));
#38698=CARTESIAN_POINT('Ctrl Pts',(11.4598615582757,-169.06175111262,-2.06354052510241E-11));
#38699=CARTESIAN_POINT('Ctrl Pts',(8.59489616869782,-168.88675111262,-4.9622656166752));
#38700=CARTESIAN_POINT('Ctrl Pts',(5.72993077911996,-168.71175111262,-9.92453123332976));
#38701=CARTESIAN_POINT('Ctrl Pts',(-1.78726082715848E-11,-168.53675111262,
-9.92453123331945));
#38702=CARTESIAN_POINT('Ctrl Pts',(-5.7299307791557,-168.36175111262,-9.92453123330913));
#38703=CARTESIAN_POINT('Ctrl Pts',(-8.59489616871569,-168.18675111262,-4.96226561664425));
#38704=CARTESIAN_POINT('Ctrl Pts',(-11.4598615582757,-168.01175111262,2.06368086793017E-11));
#38705=CARTESIAN_POINT('Ctrl Pts',(-8.59489616869782,-167.83675111262,4.9622656166752));
#38706=CARTESIAN_POINT('Ctrl Pts',(-5.72993077911996,-167.66175111262,9.92453123332977));
#38707=CARTESIAN_POINT('Ctrl Pts',(1.7871392867044E-11,-167.48675111262,
9.92453123331945));
#38708=CARTESIAN_POINT('Ctrl Pts',(5.7299307791557,-167.31175111262,9.92453123330913));
#38709=CARTESIAN_POINT('Ctrl Pts',(8.59489616871569,-167.13675111262,4.96226561664425));
#38710=CARTESIAN_POINT('Ctrl Pts',(11.4598615582757,-166.96175111262,-2.06354052510241E-11));
#38711=CARTESIAN_POINT('Ctrl Pts',(8.59489616869782,-166.78675111262,-4.9622656166752));
#38712=CARTESIAN_POINT('Ctrl Pts',(5.72993077911996,-166.61175111262,-9.92453123332976));
#38713=CARTESIAN_POINT('Ctrl Pts',(-1.78726082715848E-11,-166.43675111262,
-9.92453123331945));
#38714=CARTESIAN_POINT('Ctrl Pts',(-5.7299307791557,-166.26175111262,-9.92453123330913));
#38715=CARTESIAN_POINT('Ctrl Pts',(-8.59489616871569,-166.08675111262,-4.96226561664425));
#38716=CARTESIAN_POINT('Ctrl Pts',(-11.4598615582757,-165.91175111262,2.06368086793017E-11));
#38717=CARTESIAN_POINT('Ctrl Pts',(-8.59489616869782,-165.73675111262,4.9622656166752));
#38718=CARTESIAN_POINT('Ctrl Pts',(-5.72993077911996,-165.56175111262,9.92453123332977));
#38719=CARTESIAN_POINT('Ctrl Pts',(1.7871392867044E-11,-165.38675111262,
9.92453123331945));
#38720=CARTESIAN_POINT('Ctrl Pts',(5.7299307791557,-165.21175111262,9.92453123330913));
#38721=CARTESIAN_POINT('Ctrl Pts',(8.59489616871569,-165.03675111262,4.96226561664425));
#38722=CARTESIAN_POINT('Ctrl Pts',(11.4598615582757,-164.86175111262,-2.06354052510241E-11));
#38723=CARTESIAN_POINT('Ctrl Pts',(8.59489616869782,-164.68675111262,-4.9622656166752));
#38724=CARTESIAN_POINT('Ctrl Pts',(5.72993077911996,-164.51175111262,-9.92453123332976));
#38725=CARTESIAN_POINT('Ctrl Pts',(-1.78726082715848E-11,-164.33675111262,
-9.92453123331945));
#38726=CARTESIAN_POINT('Ctrl Pts',(-5.7299307791557,-164.16175111262,-9.92453123330913));
#38727=CARTESIAN_POINT('Ctrl Pts',(-8.59489616871569,-163.98675111262,-4.96226561664425));
#38728=CARTESIAN_POINT('Ctrl Pts',(-11.4598615582757,-163.81175111262,2.06368086793017E-11));
#38729=CARTESIAN_POINT('Ctrl Pts',(-8.59489616869782,-163.63675111262,4.9622656166752));
#38730=CARTESIAN_POINT('Ctrl Pts',(-5.72993077911996,-163.46175111262,9.92453123332977));
#38731=CARTESIAN_POINT('Ctrl Pts',(1.7871392867044E-11,-163.28675111262,
9.92453123331945));
#38732=CARTESIAN_POINT('Ctrl Pts',(5.7299307791557,-163.11175111262,9.92453123330913));
#38733=CARTESIAN_POINT('Ctrl Pts',(8.59489616871569,-162.93675111262,4.96226561664425));
#38734=CARTESIAN_POINT('Ctrl Pts',(11.4598615582757,-162.76175111262,-2.06354052510241E-11));
#38735=CARTESIAN_POINT('Ctrl Pts',(8.59489616869782,-162.58675111262,-4.9622656166752));
#38736=CARTESIAN_POINT('Ctrl Pts',(5.72993077911996,-162.41175111262,-9.92453123332976));
#38737=CARTESIAN_POINT('Ctrl Pts',(-1.78726082715848E-11,-162.23675111262,
-9.92453123331945));
#38738=CARTESIAN_POINT('Ctrl Pts',(-5.7299307791557,-162.06175111262,-9.92453123330913));
#38739=CARTESIAN_POINT('Ctrl Pts',(-8.59489616871569,-161.88675111262,-4.96226561664425));
#38740=CARTESIAN_POINT('Ctrl Pts',(-11.4598615582757,-161.71175111262,2.06368086793017E-11));
#38741=CARTESIAN_POINT('Ctrl Pts',(-8.59489616869782,-161.53675111262,4.9622656166752));
#38742=CARTESIAN_POINT('Ctrl Pts',(-5.72993077911996,-161.36175111262,9.92453123332977));
#38743=CARTESIAN_POINT('Ctrl Pts',(1.7871392867044E-11,-161.18675111262,
9.92453123331945));
#38744=CARTESIAN_POINT('Ctrl Pts',(5.7299307791557,-161.01175111262,9.92453123330913));
#38745=CARTESIAN_POINT('Ctrl Pts',(8.59489616871569,-160.83675111262,4.96226561664425));
#38746=CARTESIAN_POINT('Ctrl Pts',(11.4598615582757,-160.66175111262,-2.06354052510241E-11));
#38747=CARTESIAN_POINT('Ctrl Pts',(8.59489616869782,-160.48675111262,-4.9622656166752));
#38748=CARTESIAN_POINT('Ctrl Pts',(5.72993077911996,-160.31175111262,-9.92453123332976));
#38749=CARTESIAN_POINT('Ctrl Pts',(-1.78726082715848E-11,-160.13675111262,
-9.92453123331945));
#38750=CARTESIAN_POINT('Ctrl Pts',(-5.7299307791557,-159.96175111262,-9.92453123330913));
#38751=CARTESIAN_POINT('Ctrl Pts',(-8.59489616871569,-159.78675111262,-4.96226561664425));
#38752=CARTESIAN_POINT('Ctrl Pts',(-11.4598615582757,-159.61175111262,2.06368086793017E-11));
#38753=CARTESIAN_POINT('Ctrl Pts',(-8.59489616869782,-159.43675111262,4.9622656166752));
#38754=CARTESIAN_POINT('Ctrl Pts',(-5.72993077911996,-159.26175111262,9.92453123332977));
#38755=CARTESIAN_POINT('Ctrl Pts',(1.7871392867044E-11,-159.08675111262,
9.92453123331945));
#38756=CARTESIAN_POINT('Ctrl Pts',(5.7299307791557,-158.91175111262,9.92453123330913));
#38757=CARTESIAN_POINT('Ctrl Pts',(8.59489616871569,-158.73675111262,4.96226561664425));
#38758=CARTESIAN_POINT('Ctrl Pts',(11.4598615582757,-158.56175111262,-2.06354052510241E-11));
#38759=CARTESIAN_POINT('Ctrl Pts',(8.59489616869782,-158.38675111262,-4.9622656166752));
#38760=CARTESIAN_POINT('Ctrl Pts',(5.72993077911996,-158.21175111262,-9.92453123332976));
#38761=CARTESIAN_POINT('Ctrl Pts',(-1.78726082715848E-11,-158.03675111262,
-9.92453123331945));
#38762=CARTESIAN_POINT('Ctrl Pts',(-5.7299307791557,-157.86175111262,-9.92453123330913));
#38763=CARTESIAN_POINT('Ctrl Pts',(-8.59489616871569,-157.68675111262,-4.96226561664425));
#38764=CARTESIAN_POINT('Ctrl Pts',(-11.4598615582757,-157.51175111262,2.06368086793017E-11));
#38765=CARTESIAN_POINT('Ctrl Pts',(-8.59489616869782,-157.33675111262,4.9622656166752));
#38766=CARTESIAN_POINT('Ctrl Pts',(-5.72993077911996,-157.16175111262,9.92453123332977));
#38767=CARTESIAN_POINT('Ctrl Pts',(1.7871392867044E-11,-156.98675111262,
9.92453123331945));
#38768=CARTESIAN_POINT('Ctrl Pts',(5.7299307791557,-156.81175111262,9.92453123330913));
#38769=CARTESIAN_POINT('Ctrl Pts',(8.59489616871569,-156.63675111262,4.96226561664425));
#38770=CARTESIAN_POINT('Ctrl Pts',(11.4598615582757,-156.46175111262,-2.06354052510241E-11));
#38771=CARTESIAN_POINT('Ctrl Pts',(8.59489616869782,-156.28675111262,-4.9622656166752));
#38772=CARTESIAN_POINT('Ctrl Pts',(5.72993077911996,-156.11175111262,-9.92453123332976));
#38773=CARTESIAN_POINT('Ctrl Pts',(-1.78726082715848E-11,-155.93675111262,
-9.92453123331945));
#38774=CARTESIAN_POINT('Ctrl Pts',(-5.7299307791557,-155.76175111262,-9.92453123330913));
#38775=CARTESIAN_POINT('Ctrl Pts',(-8.59489616871569,-155.58675111262,-4.96226561664425));
#38776=CARTESIAN_POINT('Ctrl Pts',(-11.4598615582757,-155.41175111262,2.06368086793017E-11));
#38777=CARTESIAN_POINT('Ctrl Pts',(-8.59489616869782,-155.23675111262,4.9622656166752));
#38778=CARTESIAN_POINT('Ctrl Pts',(-5.72993077911996,-155.06175111262,9.92453123332977));
#38779=CARTESIAN_POINT('Ctrl Pts',(1.7871392867044E-11,-154.88675111262,
9.92453123331945));
#38780=CARTESIAN_POINT('Ctrl Pts',(5.7299307791557,-154.71175111262,9.92453123330913));
#38781=CARTESIAN_POINT('Ctrl Pts',(8.59489616871569,-154.53675111262,4.96226561664425));
#38782=CARTESIAN_POINT('Ctrl Pts',(11.4598615582757,-154.36175111262,-2.06354052510241E-11));
#38783=CARTESIAN_POINT('Ctrl Pts',(8.59489616869782,-154.18675111262,-4.9622656166752));
#38784=CARTESIAN_POINT('Ctrl Pts',(5.72993077911996,-154.01175111262,-9.92453123332976));
#38785=CARTESIAN_POINT('Ctrl Pts',(-1.78726082715848E-11,-153.83675111262,
-9.92453123331945));
#38786=CARTESIAN_POINT('Ctrl Pts',(-5.7299307791557,-153.66175111262,-9.92453123330913));
#38787=CARTESIAN_POINT('Ctrl Pts',(-8.59489616871569,-153.48675111262,-4.96226561664425));
#38788=CARTESIAN_POINT('Ctrl Pts',(-11.4598615582757,-153.31175111262,2.06368086793017E-11));
#38789=CARTESIAN_POINT('Ctrl Pts',(-8.59489616869782,-153.13675111262,4.9622656166752));
#38790=CARTESIAN_POINT('Ctrl Pts',(-5.72993077911996,-152.96175111262,9.92453123332977));
#38791=CARTESIAN_POINT('Ctrl Pts',(1.7871392867044E-11,-152.78675111262,
9.92453123331945));
#38792=CARTESIAN_POINT('Ctrl Pts',(5.7299307791557,-152.61175111262,9.92453123330913));
#38793=CARTESIAN_POINT('Ctrl Pts',(8.59489616871569,-152.43675111262,4.96226561664425));
#38794=CARTESIAN_POINT('Ctrl Pts',(11.4598615582757,-152.26175111262,-2.06354052510241E-11));
#38795=CARTESIAN_POINT('Ctrl Pts',(8.59489616869782,-152.08675111262,-4.9622656166752));
#38796=CARTESIAN_POINT('Ctrl Pts',(5.72993077911996,-151.91175111262,-9.92453123332976));
#38797=CARTESIAN_POINT('Ctrl Pts',(-1.78726082715848E-11,-151.73675111262,
-9.92453123331945));
#38798=CARTESIAN_POINT('Ctrl Pts',(-5.7299307791557,-151.56175111262,-9.92453123330913));
#38799=CARTESIAN_POINT('Ctrl Pts',(-8.59489616871569,-151.38675111262,-4.96226561664425));
#38800=CARTESIAN_POINT('Ctrl Pts',(-11.4598615582757,-151.21175111262,2.06368086793017E-11));
#38801=CARTESIAN_POINT('Ctrl Pts',(-8.59489616869782,-151.03675111262,4.9622656166752));
#38802=CARTESIAN_POINT('Ctrl Pts',(-5.72993077911996,-150.86175111262,9.92453123332977));
#38803=CARTESIAN_POINT('Ctrl Pts',(1.7871392867044E-11,-150.68675111262,
9.92453123331945));
#38804=CARTESIAN_POINT('Ctrl Pts',(5.7299307791557,-150.51175111262,9.92453123330913));
#38805=CARTESIAN_POINT('Ctrl Pts',(8.59489616871569,-150.33675111262,4.96226561664425));
#38806=CARTESIAN_POINT('Ctrl Pts',(11.4598615582757,-150.16175111262,-2.06354052510241E-11));
#38807=CARTESIAN_POINT('Ctrl Pts',(8.59489616869782,-149.98675111262,-4.9622656166752));
#38808=CARTESIAN_POINT('Ctrl Pts',(5.72993077911996,-149.81175111262,-9.92453123332976));
#38809=CARTESIAN_POINT('Ctrl Pts',(-1.78726082715848E-11,-149.63675111262,
-9.92453123331945));
#38810=CARTESIAN_POINT('Ctrl Pts',(-5.7299307791557,-149.46175111262,-9.92453123330913));
#38811=CARTESIAN_POINT('Ctrl Pts',(-8.59489616871569,-149.28675111262,-4.96226561664425));
#38812=CARTESIAN_POINT('Ctrl Pts',(-11.4598615582757,-149.11175111262,2.06368086793017E-11));
#38813=CARTESIAN_POINT('Ctrl Pts',(-8.59489616869782,-148.93675111262,4.9622656166752));
#38814=CARTESIAN_POINT('Ctrl Pts',(-5.72993077911996,-148.76175111262,9.92453123332977));
#38815=CARTESIAN_POINT('Ctrl Pts',(1.7871392867044E-11,-148.58675111262,
9.92453123331945));
#38816=CARTESIAN_POINT('Ctrl Pts',(5.7299307791557,-148.41175111262,9.92453123330913));
#38817=CARTESIAN_POINT('Ctrl Pts',(8.59489616871569,-148.23675111262,4.96226561664425));
#38818=CARTESIAN_POINT('Ctrl Pts',(11.4598615582757,-148.06175111262,-2.06354052510241E-11));
#38819=CARTESIAN_POINT('Ctrl Pts',(8.59489616869782,-147.88675111262,-4.9622656166752));
#38820=CARTESIAN_POINT('Ctrl Pts',(5.72993077911996,-147.71175111262,-9.92453123332976));
#38821=CARTESIAN_POINT('Ctrl Pts',(-1.78726082715848E-11,-147.53675111262,
-9.92453123331945));
#38822=CARTESIAN_POINT('Ctrl Pts',(-5.7299307791557,-147.36175111262,-9.92453123330913));
#38823=CARTESIAN_POINT('Ctrl Pts',(-8.59489616871569,-147.18675111262,-4.96226561664425));
#38824=CARTESIAN_POINT('Ctrl Pts',(-11.4598615582757,-147.01175111262,2.06368086793017E-11));
#38825=CARTESIAN_POINT('Ctrl Pts',(-8.59489616869782,-146.83675111262,4.9622656166752));
#38826=CARTESIAN_POINT('Ctrl Pts',(-5.72993077911996,-146.66175111262,9.92453123332977));
#38827=CARTESIAN_POINT('Ctrl Pts',(1.7871392867044E-11,-146.48675111262,
9.92453123331945));
#38828=CARTESIAN_POINT('Ctrl Pts',(5.7299307791557,-146.31175111262,9.92453123330913));
#38829=CARTESIAN_POINT('Ctrl Pts',(8.59489616871569,-146.13675111262,4.96226561664425));
#38830=CARTESIAN_POINT('Ctrl Pts',(11.4598615582757,-145.96175111262,-2.06354052510241E-11));
#38831=CARTESIAN_POINT('Ctrl Pts',(8.59489616869782,-145.78675111262,-4.9622656166752));
#38832=CARTESIAN_POINT('Ctrl Pts',(5.72993077911996,-145.61175111262,-9.92453123332976));
#38833=CARTESIAN_POINT('Ctrl Pts',(-1.78726082715848E-11,-145.43675111262,
-9.92453123331945));
#38834=CARTESIAN_POINT('Ctrl Pts',(-5.7299307791557,-145.26175111262,-9.92453123330913));
#38835=CARTESIAN_POINT('Ctrl Pts',(-8.59489616871569,-145.08675111262,-4.96226561664425));
#38836=CARTESIAN_POINT('Ctrl Pts',(-11.4598615582757,-144.91175111262,2.06368086793017E-11));
#38837=CARTESIAN_POINT('Ctrl Pts',(-8.59489616869782,-144.73675111262,4.9622656166752));
#38838=CARTESIAN_POINT('Ctrl Pts',(-5.72993077911996,-144.56175111262,9.92453123332977));
#38839=CARTESIAN_POINT('Ctrl Pts',(1.7871392867044E-11,-144.38675111262,
9.92453123331945));
#38840=CARTESIAN_POINT('Ctrl Pts',(5.7299307791557,-144.21175111262,9.92453123330913));
#38841=CARTESIAN_POINT('Ctrl Pts',(8.59489616871569,-144.03675111262,4.96226561664425));
#38842=CARTESIAN_POINT('Ctrl Pts',(11.4598615582757,-143.86175111262,-2.06354052510241E-11));
#38843=CARTESIAN_POINT('Ctrl Pts',(8.59489616869782,-143.68675111262,-4.9622656166752));
#38844=CARTESIAN_POINT('Ctrl Pts',(5.72993077911996,-143.51175111262,-9.92453123332976));
#38845=CARTESIAN_POINT('Ctrl Pts',(-1.78726082715848E-11,-143.33675111262,
-9.92453123331945));
#38846=CARTESIAN_POINT('Ctrl Pts',(-5.7299307791557,-143.16175111262,-9.92453123330913));
#38847=CARTESIAN_POINT('Ctrl Pts',(-8.59489616871569,-142.98675111262,-4.96226561664425));
#38848=CARTESIAN_POINT('Ctrl Pts',(-11.4598615582757,-142.81175111262,2.06368086793017E-11));
#38849=CARTESIAN_POINT('Ctrl Pts',(-8.59489616869782,-142.63675111262,4.9622656166752));
#38850=CARTESIAN_POINT('Ctrl Pts',(-5.72993077911996,-142.46175111262,9.92453123332977));
#38851=CARTESIAN_POINT('Ctrl Pts',(1.7871392867044E-11,-142.28675111262,
9.92453123331945));
#38852=CARTESIAN_POINT('Ctrl Pts',(5.7299307791557,-142.11175111262,9.92453123330913));
#38853=CARTESIAN_POINT('Ctrl Pts',(8.59489616871569,-141.93675111262,4.96226561664425));
#38854=CARTESIAN_POINT('Ctrl Pts',(11.4598615582757,-141.76175111262,-2.06354052510241E-11));
#38855=CARTESIAN_POINT('Ctrl Pts',(8.59489616869782,-141.58675111262,-4.9622656166752));
#38856=CARTESIAN_POINT('Ctrl Pts',(5.72993077911996,-141.41175111262,-9.92453123332976));
#38857=CARTESIAN_POINT('Ctrl Pts',(-1.78726082715848E-11,-141.23675111262,
-9.92453123331945));
#38858=CARTESIAN_POINT('Ctrl Pts',(-5.7299307791557,-141.06175111262,-9.92453123330913));
#38859=CARTESIAN_POINT('Ctrl Pts',(-8.59489616871569,-140.88675111262,-4.96226561664425));
#38860=CARTESIAN_POINT('Ctrl Pts',(-11.4598615582757,-140.71175111262,2.06368086793017E-11));
#38861=CARTESIAN_POINT('Ctrl Pts',(-8.59489616869782,-140.53675111262,4.9622656166752));
#38862=CARTESIAN_POINT('Ctrl Pts',(-5.72993077911996,-140.36175111262,9.92453123332977));
#38863=CARTESIAN_POINT('Ctrl Pts',(1.7871392867044E-11,-140.18675111262,
9.92453123331945));
#38864=CARTESIAN_POINT('Ctrl Pts',(5.7299307791557,-140.01175111262,9.92453123330913));
#38865=CARTESIAN_POINT('Ctrl Pts',(8.59489616871569,-139.83675111262,4.96226561664425));
#38866=CARTESIAN_POINT('Ctrl Pts',(11.4598615582757,-139.66175111262,-2.06354052510241E-11));
#38867=CARTESIAN_POINT('Ctrl Pts',(8.59489616869782,-139.48675111262,-4.9622656166752));
#38868=CARTESIAN_POINT('Ctrl Pts',(5.72993077911996,-139.31175111262,-9.92453123332976));
#38869=CARTESIAN_POINT('Ctrl Pts',(-1.78726082715848E-11,-139.13675111262,
-9.92453123331945));
#38870=CARTESIAN_POINT('Ctrl Pts',(-5.7299307791557,-138.96175111262,-9.92453123330913));
#38871=CARTESIAN_POINT('Ctrl Pts',(-8.59489616871569,-138.78675111262,-4.96226561664425));
#38872=CARTESIAN_POINT('Ctrl Pts',(-11.4598615582757,-138.61175111262,2.06368086793017E-11));
#38873=CARTESIAN_POINT('Ctrl Pts',(-8.59489616869782,-138.43675111262,4.9622656166752));
#38874=CARTESIAN_POINT('Ctrl Pts',(-5.72993077911996,-138.26175111262,9.92453123332977));
#38875=CARTESIAN_POINT('Ctrl Pts',(1.7871392867044E-11,-138.08675111262,
9.92453123331945));
#38876=CARTESIAN_POINT('Ctrl Pts',(5.7299307791557,-137.91175111262,9.92453123330913));
#38877=CARTESIAN_POINT('Ctrl Pts',(8.59489616871569,-137.73675111262,4.96226561664425));
#38878=CARTESIAN_POINT('Ctrl Pts',(11.4598615582757,-137.56175111262,-2.06354052510241E-11));
#38879=CARTESIAN_POINT('Ctrl Pts',(8.59489616869782,-137.38675111262,-4.9622656166752));
#38880=CARTESIAN_POINT('Ctrl Pts',(5.72993077911996,-137.21175111262,-9.92453123332976));
#38881=CARTESIAN_POINT('Ctrl Pts',(-1.78726082715848E-11,-137.03675111262,
-9.92453123331945));
#38882=CARTESIAN_POINT('Ctrl Pts',(-5.7299307791557,-136.86175111262,-9.92453123330913));
#38883=CARTESIAN_POINT('Ctrl Pts',(-8.59489616871569,-136.68675111262,-4.96226561664425));
#38884=CARTESIAN_POINT('Ctrl Pts',(-11.4598615582757,-136.51175111262,2.06368086793017E-11));
#38885=CARTESIAN_POINT('Ctrl Pts',(-8.59489616869782,-136.33675111262,4.9622656166752));
#38886=CARTESIAN_POINT('Ctrl Pts',(-5.72993077911996,-136.16175111262,9.92453123332977));
#38887=CARTESIAN_POINT('Ctrl Pts',(1.7871392867044E-11,-135.98675111262,
9.92453123331945));
#38888=CARTESIAN_POINT('Ctrl Pts',(5.7299307791557,-135.81175111262,9.92453123330913));
#38889=CARTESIAN_POINT('Ctrl Pts',(8.59489616871569,-135.63675111262,4.96226561664425));
#38890=CARTESIAN_POINT('Ctrl Pts',(11.4598615582757,-135.46175111262,-2.06354052510241E-11));
#38891=CARTESIAN_POINT('Ctrl Pts',(8.59489616869782,-135.28675111262,-4.9622656166752));
#38892=CARTESIAN_POINT('Ctrl Pts',(5.72993077911996,-135.11175111262,-9.92453123332976));
#38893=CARTESIAN_POINT('Ctrl Pts',(-1.78726082715848E-11,-134.93675111262,
-9.92453123331945));
#38894=CARTESIAN_POINT('Ctrl Pts',(-5.7299307791557,-134.76175111262,-9.92453123330913));
#38895=CARTESIAN_POINT('Ctrl Pts',(-8.59489616871569,-134.58675111262,-4.96226561664425));
#38896=CARTESIAN_POINT('Ctrl Pts',(-11.4598615582757,-134.41175111262,2.06368086793017E-11));
#38897=CARTESIAN_POINT('Ctrl Pts',(-8.59489616869782,-134.23675111262,4.9622656166752));
#38898=CARTESIAN_POINT('Ctrl Pts',(-5.72993077911996,-134.06175111262,9.92453123332977));
#38899=CARTESIAN_POINT('Ctrl Pts',(1.7871392867044E-11,-133.88675111262,
9.92453123331945));
#38900=CARTESIAN_POINT('Ctrl Pts',(5.7299307791557,-133.71175111262,9.92453123330913));
#38901=CARTESIAN_POINT('Ctrl Pts',(8.59489616871569,-133.53675111262,4.96226561664425));
#38902=CARTESIAN_POINT('Ctrl Pts',(11.4598615582757,-133.36175111262,-2.06354052510241E-11));
#38903=CARTESIAN_POINT('Ctrl Pts',(8.59489616869782,-133.18675111262,-4.9622656166752));
#38904=CARTESIAN_POINT('Ctrl Pts',(5.72993077911996,-133.01175111262,-9.92453123332976));
#38905=CARTESIAN_POINT('Ctrl Pts',(-1.78726082715848E-11,-132.83675111262,
-9.92453123331945));
#38906=CARTESIAN_POINT('Ctrl Pts',(-5.7299307791557,-132.66175111262,-9.92453123330913));
#38907=CARTESIAN_POINT('Ctrl Pts',(-8.59489616871569,-132.48675111262,-4.96226561664425));
#38908=CARTESIAN_POINT('Ctrl Pts',(-11.4598615582757,-132.31175111262,2.06368086793017E-11));
#38909=CARTESIAN_POINT('Ctrl Pts',(-8.59489616869782,-132.13675111262,4.9622656166752));
#38910=CARTESIAN_POINT('Ctrl Pts',(-5.72993077911996,-131.96175111262,9.92453123332977));
#38911=CARTESIAN_POINT('Ctrl Pts',(1.7871392867044E-11,-131.78675111262,
9.92453123331945));
#38912=CARTESIAN_POINT('Ctrl Pts',(5.7299307791557,-131.61175111262,9.92453123330913));
#38913=CARTESIAN_POINT('Ctrl Pts',(8.59489616871569,-131.43675111262,4.96226561664425));
#38914=CARTESIAN_POINT('Ctrl Pts',(11.4598615582757,-131.26175111262,-2.06354052510241E-11));
#38915=CARTESIAN_POINT('Ctrl Pts',(8.59489616869782,-131.08675111262,-4.9622656166752));
#38916=CARTESIAN_POINT('Ctrl Pts',(5.72993077911996,-130.91175111262,-9.92453123332976));
#38917=CARTESIAN_POINT('Ctrl Pts',(-1.78726082715848E-11,-130.73675111262,
-9.92453123331945));
#38918=CARTESIAN_POINT('Ctrl Pts',(-5.7299307791557,-130.56175111262,-9.92453123330913));
#38919=CARTESIAN_POINT('Ctrl Pts',(-8.59489616871569,-130.38675111262,-4.96226561664425));
#38920=CARTESIAN_POINT('Ctrl Pts',(-11.4598615582757,-130.21175111262,2.06368086793017E-11));
#38921=CARTESIAN_POINT('Ctrl Pts',(-8.59489616869782,-130.03675111262,4.9622656166752));
#38922=CARTESIAN_POINT('Ctrl Pts',(-5.72993077911996,-129.86175111262,9.92453123332977));
#38923=CARTESIAN_POINT('Ctrl Pts',(1.7871392867044E-11,-129.68675111262,
9.92453123331945));
#38924=CARTESIAN_POINT('Ctrl Pts',(5.7299307791557,-129.51175111262,9.92453123330913));
#38925=CARTESIAN_POINT('Ctrl Pts',(8.59489616871569,-129.33675111262,4.96226561664425));
#38926=CARTESIAN_POINT('Ctrl Pts',(11.4598615582757,-129.16175111262,-2.06354052510241E-11));
#38927=CARTESIAN_POINT('Ctrl Pts',(8.59489616869782,-128.98675111262,-4.9622656166752));
#38928=CARTESIAN_POINT('Ctrl Pts',(5.72993077911996,-128.81175111262,-9.92453123332976));
#38929=CARTESIAN_POINT('Ctrl Pts',(-1.78726082715848E-11,-128.63675111262,
-9.92453123331945));
#38930=CARTESIAN_POINT('Ctrl Pts',(-5.7299307791557,-128.46175111262,-9.92453123330913));
#38931=CARTESIAN_POINT('Ctrl Pts',(-8.59489616871569,-128.28675111262,-4.96226561664425));
#38932=CARTESIAN_POINT('Ctrl Pts',(-11.4598615582757,-128.11175111262,2.06368086793017E-11));
#38933=CARTESIAN_POINT('Ctrl Pts',(-8.59489616869782,-127.93675111262,4.9622656166752));
#38934=CARTESIAN_POINT('Ctrl Pts',(-5.72993077911996,-127.76175111262,9.92453123332977));
#38935=CARTESIAN_POINT('Ctrl Pts',(1.7871392867044E-11,-127.58675111262,
9.92453123331945));
#38936=CARTESIAN_POINT('Ctrl Pts',(5.7299307791557,-127.41175111262,9.92453123330913));
#38937=CARTESIAN_POINT('Ctrl Pts',(8.59489616871569,-127.23675111262,4.96226561664425));
#38938=CARTESIAN_POINT('Ctrl Pts',(11.4598615582757,-127.06175111262,-2.06354052510241E-11));
#38939=CARTESIAN_POINT('Ctrl Pts',(8.59489616869782,-126.88675111262,-4.9622656166752));
#38940=CARTESIAN_POINT('Ctrl Pts',(5.72993077911996,-126.71175111262,-9.92453123332976));
#38941=CARTESIAN_POINT('Ctrl Pts',(-1.78726082715848E-11,-126.53675111262,
-9.92453123331945));
#38942=CARTESIAN_POINT('Ctrl Pts',(-5.7299307791557,-126.36175111262,-9.92453123330913));
#38943=CARTESIAN_POINT('Ctrl Pts',(-8.59489616871569,-126.18675111262,-4.96226561664425));
#38944=CARTESIAN_POINT('Ctrl Pts',(-11.4598615582757,-126.01175111262,2.06368086793017E-11));
#38945=CARTESIAN_POINT('Ctrl Pts',(-8.59489616869782,-125.83675111262,4.9622656166752));
#38946=CARTESIAN_POINT('Ctrl Pts',(-5.72993077911996,-125.66175111262,9.92453123332977));
#38947=CARTESIAN_POINT('Ctrl Pts',(1.7871392867044E-11,-125.48675111262,
9.92453123331945));
#38948=CARTESIAN_POINT('Ctrl Pts',(5.7299307791557,-125.31175111262,9.92453123330913));
#38949=CARTESIAN_POINT('Ctrl Pts',(8.59489616871569,-125.13675111262,4.96226561664425));
#38950=CARTESIAN_POINT('Ctrl Pts',(11.4598615582757,-124.96175111262,-2.06354052510241E-11));
#38951=CARTESIAN_POINT('Ctrl Pts',(8.59489616869782,-124.78675111262,-4.9622656166752));
#38952=CARTESIAN_POINT('Ctrl Pts',(5.72993077911996,-124.61175111262,-9.92453123332976));
#38953=CARTESIAN_POINT('Ctrl Pts',(-1.78726082715848E-11,-124.43675111262,
-9.92453123331945));
#38954=CARTESIAN_POINT('Ctrl Pts',(-5.7299307791557,-124.26175111262,-9.92453123330913));
#38955=CARTESIAN_POINT('Ctrl Pts',(-8.59489616871569,-124.08675111262,-4.96226561664425));
#38956=CARTESIAN_POINT('Ctrl Pts',(-11.4598615582757,-123.91175111262,2.06368086793017E-11));
#38957=CARTESIAN_POINT('Ctrl Pts',(-8.59489616869782,-123.73675111262,4.9622656166752));
#38958=CARTESIAN_POINT('Ctrl Pts',(-5.72993077911996,-123.56175111262,9.92453123332977));
#38959=CARTESIAN_POINT('Ctrl Pts',(1.7871392867044E-11,-123.38675111262,
9.92453123331945));
#38960=CARTESIAN_POINT('Ctrl Pts',(5.7299307791557,-123.21175111262,9.92453123330913));
#38961=CARTESIAN_POINT('Ctrl Pts',(8.59489616871569,-123.03675111262,4.96226561664425));
#38962=CARTESIAN_POINT('Ctrl Pts',(11.4598615582757,-122.86175111262,-2.06354052510241E-11));
#38963=CARTESIAN_POINT('Ctrl Pts',(8.59489616869782,-122.68675111262,-4.9622656166752));
#38964=CARTESIAN_POINT('Ctrl Pts',(5.72993077911996,-122.51175111262,-9.92453123332976));
#38965=CARTESIAN_POINT('Ctrl Pts',(-1.78726082715848E-11,-122.33675111262,
-9.92453123331945));
#38966=CARTESIAN_POINT('Ctrl Pts',(-5.7299307791557,-122.16175111262,-9.92453123330913));
#38967=CARTESIAN_POINT('Ctrl Pts',(-8.59489616871569,-121.98675111262,-4.96226561664425));
#38968=CARTESIAN_POINT('Ctrl Pts',(-11.4598615582757,-121.81175111262,2.06368086793017E-11));
#38969=CARTESIAN_POINT('Ctrl Pts',(-8.59489616869782,-121.63675111262,4.9622656166752));
#38970=CARTESIAN_POINT('Ctrl Pts',(-5.72993077911996,-121.46175111262,9.92453123332977));
#38971=CARTESIAN_POINT('Ctrl Pts',(1.7871392867044E-11,-121.28675111262,
9.92453123331945));
#38972=CARTESIAN_POINT('Ctrl Pts',(5.7299307791557,-121.11175111262,9.92453123330913));
#38973=CARTESIAN_POINT('Ctrl Pts',(8.59489616871569,-120.93675111262,4.96226561664425));
#38974=CARTESIAN_POINT('Ctrl Pts',(11.4598615582757,-120.76175111262,-2.06354052510241E-11));
#38975=CARTESIAN_POINT('Ctrl Pts',(8.59489616869782,-120.58675111262,-4.9622656166752));
#38976=CARTESIAN_POINT('Ctrl Pts',(5.72993077911996,-120.41175111262,-9.92453123332976));
#38977=CARTESIAN_POINT('Ctrl Pts',(-1.78726082715848E-11,-120.23675111262,
-9.92453123331945));
#38978=CARTESIAN_POINT('Ctrl Pts',(-5.7299307791557,-120.06175111262,-9.92453123330913));
#38979=CARTESIAN_POINT('Ctrl Pts',(-8.59489616871569,-119.88675111262,-4.96226561664425));
#38980=CARTESIAN_POINT('Ctrl Pts',(-11.4598615582757,-119.71175111262,2.06368086793017E-11));
#38981=CARTESIAN_POINT('Ctrl Pts',(-8.59489616869782,-119.53675111262,4.9622656166752));
#38982=CARTESIAN_POINT('Ctrl Pts',(-5.72993077911996,-119.36175111262,9.92453123332977));
#38983=CARTESIAN_POINT('Ctrl Pts',(1.7871392867044E-11,-119.18675111262,
9.92453123331945));
#38984=CARTESIAN_POINT('Ctrl Pts',(5.7299307791557,-119.01175111262,9.92453123330913));
#38985=CARTESIAN_POINT('Ctrl Pts',(8.59489616871569,-118.83675111262,4.96226561664425));
#38986=CARTESIAN_POINT('Ctrl Pts',(11.4598615582757,-118.66175111262,-2.06354052510241E-11));
#38987=CARTESIAN_POINT('Ctrl Pts',(8.59489616869782,-118.48675111262,-4.9622656166752));
#38988=CARTESIAN_POINT('Ctrl Pts',(5.72993077911996,-118.31175111262,-9.92453123332976));
#38989=CARTESIAN_POINT('Ctrl Pts',(-1.78726082715848E-11,-118.13675111262,
-9.92453123331945));
#38990=CARTESIAN_POINT('Ctrl Pts',(-5.7299307791557,-117.96175111262,-9.92453123330913));
#38991=CARTESIAN_POINT('Ctrl Pts',(-8.59489616871569,-117.78675111262,-4.96226561664425));
#38992=CARTESIAN_POINT('Ctrl Pts',(-11.4598615582757,-117.61175111262,2.06368086793017E-11));
#38993=CARTESIAN_POINT('Ctrl Pts',(-8.59489616869782,-117.43675111262,4.9622656166752));
#38994=CARTESIAN_POINT('Ctrl Pts',(-5.72993077911996,-117.26175111262,9.92453123332977));
#38995=CARTESIAN_POINT('Ctrl Pts',(1.7871392867044E-11,-117.08675111262,
9.92453123331945));
#38996=CARTESIAN_POINT('Ctrl Pts',(5.7299307791557,-116.91175111262,9.92453123330913));
#38997=CARTESIAN_POINT('Ctrl Pts',(8.59489616871569,-116.73675111262,4.96226561664425));
#38998=CARTESIAN_POINT('Ctrl Pts',(11.4598615582757,-116.56175111262,-2.06354052510241E-11));
#38999=CARTESIAN_POINT('Ctrl Pts',(8.59489616869782,-116.38675111262,-4.9622656166752));
#39000=CARTESIAN_POINT('Ctrl Pts',(5.72993077911996,-116.21175111262,-9.92453123332976));
#39001=CARTESIAN_POINT('Ctrl Pts',(-1.78726082715848E-11,-116.03675111262,
-9.92453123331945));
#39002=CARTESIAN_POINT('Ctrl Pts',(-5.7299307791557,-115.86175111262,-9.92453123330913));
#39003=CARTESIAN_POINT('Ctrl Pts',(-8.59489616871569,-115.68675111262,-4.96226561664425));
#39004=CARTESIAN_POINT('Ctrl Pts',(-11.4598615582757,-115.51175111262,2.06368086793017E-11));
#39005=CARTESIAN_POINT('Ctrl Pts',(-8.59489616869782,-115.33675111262,4.9622656166752));
#39006=CARTESIAN_POINT('Ctrl Pts',(-5.72993077911996,-115.16175111262,9.92453123332977));
#39007=CARTESIAN_POINT('Ctrl Pts',(1.7871392867044E-11,-114.98675111262,
9.92453123331945));
#39008=CARTESIAN_POINT('Ctrl Pts',(5.7299307791557,-114.81175111262,9.92453123330913));
#39009=CARTESIAN_POINT('Ctrl Pts',(8.59489616871569,-114.63675111262,4.96226561664425));
#39010=CARTESIAN_POINT('Ctrl Pts',(11.4598615582757,-114.46175111262,-2.06354052510241E-11));
#39011=CARTESIAN_POINT('Ctrl Pts',(8.59489616869782,-114.28675111262,-4.9622656166752));
#39012=CARTESIAN_POINT('Ctrl Pts',(5.72993077911996,-114.11175111262,-9.92453123332976));
#39013=CARTESIAN_POINT('Ctrl Pts',(-1.78726082715848E-11,-113.93675111262,
-9.92453123331945));
#39014=CARTESIAN_POINT('Ctrl Pts',(-5.7299307791557,-113.76175111262,-9.92453123330913));
#39015=CARTESIAN_POINT('Ctrl Pts',(-8.59489616871569,-113.58675111262,-4.96226561664425));
#39016=CARTESIAN_POINT('Ctrl Pts',(-11.4598615582757,-113.41175111262,2.06368086793017E-11));
#39017=CARTESIAN_POINT('Ctrl Pts',(-8.59489616869782,-113.23675111262,4.9622656166752));
#39018=CARTESIAN_POINT('Ctrl Pts',(-5.72993077911996,-113.06175111262,9.92453123332977));
#39019=CARTESIAN_POINT('Ctrl Pts',(1.7871392867044E-11,-112.88675111262,
9.92453123331945));
#39020=CARTESIAN_POINT('Ctrl Pts',(5.7299307791557,-112.71175111262,9.92453123330913));
#39021=CARTESIAN_POINT('Ctrl Pts',(8.59489616871569,-112.53675111262,4.96226561664425));
#39022=CARTESIAN_POINT('Ctrl Pts',(11.4598615582757,-112.36175111262,-2.06354052510241E-11));
#39023=CARTESIAN_POINT('Ctrl Pts',(8.59489616869782,-112.18675111262,-4.9622656166752));
#39024=CARTESIAN_POINT('Ctrl Pts',(5.72993077911996,-112.01175111262,-9.92453123332976));
#39025=CARTESIAN_POINT('Ctrl Pts',(-1.78726082715848E-11,-111.83675111262,
-9.92453123331945));
#39026=CARTESIAN_POINT('Ctrl Pts',(-5.7299307791557,-111.66175111262,-9.92453123330913));
#39027=CARTESIAN_POINT('Ctrl Pts',(-8.59489616871569,-111.48675111262,-4.96226561664425));
#39028=CARTESIAN_POINT('Ctrl Pts',(-11.4598615582757,-111.31175111262,2.06368086793017E-11));
#39029=CARTESIAN_POINT('Ctrl Pts',(-8.59489616869782,-111.13675111262,4.9622656166752));
#39030=CARTESIAN_POINT('Ctrl Pts',(-5.72993077911996,-110.96175111262,9.92453123332977));
#39031=CARTESIAN_POINT('Ctrl Pts',(1.7871392867044E-11,-110.78675111262,
9.92453123331945));
#39032=CARTESIAN_POINT('Ctrl Pts',(5.7299307791557,-110.61175111262,9.92453123330913));
#39033=CARTESIAN_POINT('Ctrl Pts',(8.59489616871569,-110.43675111262,4.96226561664425));
#39034=CARTESIAN_POINT('Ctrl Pts',(11.4598615582757,-110.26175111262,-2.06354052510241E-11));
#39035=CARTESIAN_POINT('Ctrl Pts',(8.59489616869782,-110.08675111262,-4.9622656166752));
#39036=CARTESIAN_POINT('Ctrl Pts',(5.72993077911996,-109.91175111262,-9.92453123332976));
#39037=CARTESIAN_POINT('Ctrl Pts',(-1.78726082715848E-11,-109.73675111262,
-9.92453123331945));
#39038=CARTESIAN_POINT('Ctrl Pts',(-5.7299307791557,-109.56175111262,-9.92453123330913));
#39039=CARTESIAN_POINT('Ctrl Pts',(-8.59489616871569,-109.38675111262,-4.96226561664425));
#39040=CARTESIAN_POINT('Ctrl Pts',(-11.4598615582757,-109.21175111262,2.06368086793017E-11));
#39041=CARTESIAN_POINT('Ctrl Pts',(-8.59489616869782,-109.03675111262,4.9622656166752));
#39042=CARTESIAN_POINT('Ctrl Pts',(-5.72993077911996,-108.86175111262,9.92453123332977));
#39043=CARTESIAN_POINT('Ctrl Pts',(1.7871392867044E-11,-108.68675111262,
9.92453123331945));
#39044=CARTESIAN_POINT('Ctrl Pts',(5.7299307791557,-108.51175111262,9.92453123330913));
#39045=CARTESIAN_POINT('Ctrl Pts',(8.59489616871569,-108.33675111262,4.96226561664425));
#39046=CARTESIAN_POINT('Ctrl Pts',(11.4598615582757,-108.16175111262,-2.06354052510241E-11));
#39047=CARTESIAN_POINT('Ctrl Pts',(8.59489616869782,-107.98675111262,-4.9622656166752));
#39048=CARTESIAN_POINT('Ctrl Pts',(5.72993077911996,-107.81175111262,-9.92453123332976));
#39049=CARTESIAN_POINT('Ctrl Pts',(-1.78726082715848E-11,-107.63675111262,
-9.92453123331945));
#39050=CARTESIAN_POINT('Ctrl Pts',(-5.7299307791557,-107.46175111262,-9.92453123330913));
#39051=CARTESIAN_POINT('Ctrl Pts',(-8.59489616871569,-107.28675111262,-4.96226561664425));
#39052=CARTESIAN_POINT('Ctrl Pts',(-11.4598615582757,-107.11175111262,2.06368086793017E-11));
#39053=CARTESIAN_POINT('Ctrl Pts',(-8.59489616869782,-106.93675111262,4.9622656166752));
#39054=CARTESIAN_POINT('Ctrl Pts',(-5.72993077911996,-106.76175111262,9.92453123332977));
#39055=CARTESIAN_POINT('Ctrl Pts',(1.7871392867044E-11,-106.58675111262,
9.92453123331945));
#39056=CARTESIAN_POINT('Ctrl Pts',(5.7299307791557,-106.41175111262,9.92453123330913));
#39057=CARTESIAN_POINT('Ctrl Pts',(8.59489616871569,-106.23675111262,4.96226561664425));
#39058=CARTESIAN_POINT('Ctrl Pts',(11.4598615582757,-106.06175111262,-2.06354052510241E-11));
#39059=CARTESIAN_POINT('Ctrl Pts',(8.59489616869782,-105.88675111262,-4.9622656166752));
#39060=CARTESIAN_POINT('Ctrl Pts',(5.72993077911996,-105.71175111262,-9.92453123332976));
#39061=CARTESIAN_POINT('Ctrl Pts',(-1.78726082715848E-11,-105.53675111262,
-9.92453123331945));
#39062=CARTESIAN_POINT('Ctrl Pts',(-5.7299307791557,-105.36175111262,-9.92453123330913));
#39063=CARTESIAN_POINT('Ctrl Pts',(-8.59489616871569,-105.18675111262,-4.96226561664425));
#39064=CARTESIAN_POINT('Ctrl Pts',(-11.4598615582757,-105.01175111262,2.06368086793017E-11));
#39065=CARTESIAN_POINT('Ctrl Pts',(-8.59489616869782,-104.83675111262,4.9622656166752));
#39066=CARTESIAN_POINT('Ctrl Pts',(-5.72993077911996,-104.66175111262,9.92453123332977));
#39067=CARTESIAN_POINT('Ctrl Pts',(1.7871392867044E-11,-104.48675111262,
9.92453123331945));
#39068=CARTESIAN_POINT('Ctrl Pts',(5.7299307791557,-104.31175111262,9.92453123330913));
#39069=CARTESIAN_POINT('Ctrl Pts',(8.59489616871569,-104.13675111262,4.96226561664425));
#39070=CARTESIAN_POINT('Ctrl Pts',(11.4598615582757,-103.96175111262,-2.06354052510241E-11));
#39071=CARTESIAN_POINT('Ctrl Pts',(8.59489616869782,-103.78675111262,-4.9622656166752));
#39072=CARTESIAN_POINT('Ctrl Pts',(5.72993077911996,-103.61175111262,-9.92453123332976));
#39073=CARTESIAN_POINT('Ctrl Pts',(-1.78726082715848E-11,-103.43675111262,
-9.92453123331945));
#39074=CARTESIAN_POINT('Ctrl Pts',(-5.7299307791557,-103.26175111262,-9.92453123330913));
#39075=CARTESIAN_POINT('Ctrl Pts',(-8.59489616871569,-103.08675111262,-4.96226561664425));
#39076=CARTESIAN_POINT('Ctrl Pts',(-11.4598615582757,-102.91175111262,2.06368086793017E-11));
#39077=CARTESIAN_POINT('Ctrl Pts',(-8.59489616869782,-102.73675111262,4.9622656166752));
#39078=CARTESIAN_POINT('Ctrl Pts',(-5.72993077911996,-102.56175111262,9.92453123332977));
#39079=CARTESIAN_POINT('Ctrl Pts',(1.7871392867044E-11,-102.38675111262,
9.92453123331945));
#39080=CARTESIAN_POINT('Ctrl Pts',(5.7299307791557,-102.21175111262,9.92453123330913));
#39081=CARTESIAN_POINT('Ctrl Pts',(8.59489616871569,-102.03675111262,4.96226561664425));
#39082=CARTESIAN_POINT('Ctrl Pts',(11.4598615582757,-101.86175111262,-2.06354052510241E-11));
#39083=CARTESIAN_POINT('Ctrl Pts',(8.59489616869782,-101.68675111262,-4.9622656166752));
#39084=CARTESIAN_POINT('Ctrl Pts',(5.72993077911996,-101.51175111262,-9.92453123332976));
#39085=CARTESIAN_POINT('Ctrl Pts',(-1.78726082715848E-11,-101.33675111262,
-9.92453123331945));
#39086=CARTESIAN_POINT('Ctrl Pts',(-5.7299307791557,-101.16175111262,-9.92453123330913));
#39087=CARTESIAN_POINT('Ctrl Pts',(-8.59489616871569,-100.98675111262,-4.96226561664425));
#39088=CARTESIAN_POINT('Ctrl Pts',(-11.4598615582757,-100.81175111262,2.06368086793017E-11));
#39089=CARTESIAN_POINT('Ctrl Pts',(-8.59489616869782,-100.63675111262,4.9622656166752));
#39090=CARTESIAN_POINT('Ctrl Pts',(-5.72993077911996,-100.46175111262,9.92453123332977));
#39091=CARTESIAN_POINT('Ctrl Pts',(1.7871392867044E-11,-100.28675111262,
9.92453123331945));
#39092=CARTESIAN_POINT('Ctrl Pts',(5.7299307791557,-100.11175111262,9.92453123330913));
#39093=CARTESIAN_POINT('Ctrl Pts',(8.59489616871569,-99.9367511126202,4.96226561664425));
#39094=CARTESIAN_POINT('Ctrl Pts',(11.4598615582757,-99.7617511126202,-2.06354052510241E-11));
#39095=CARTESIAN_POINT('Ctrl Pts',(8.59489616869782,-99.5867511126202,-4.9622656166752));
#39096=CARTESIAN_POINT('Ctrl Pts',(5.72993077911996,-99.4117511126202,-9.92453123332976));
#39097=CARTESIAN_POINT('Ctrl Pts',(-1.78726082715848E-11,-99.2367511126202,
-9.92453123331945));
#39098=CARTESIAN_POINT('Ctrl Pts',(-5.7299307791557,-99.0617511126202,-9.92453123330913));
#39099=CARTESIAN_POINT('Ctrl Pts',(-8.59489616871569,-98.8867511126202,
-4.96226561664425));
#39100=CARTESIAN_POINT('Ctrl Pts',(-11.4598615582757,-98.7117511126202,
2.06368086793017E-11));
#39101=CARTESIAN_POINT('Ctrl Pts',(-8.59489616869782,-98.5367511126202,
4.9622656166752));
#39102=CARTESIAN_POINT('Ctrl Pts',(-5.72993077911996,-98.3617511126202,
9.92453123332977));
#39103=CARTESIAN_POINT('Ctrl Pts',(1.7871392867044E-11,-98.1867511126202,
9.92453123331945));
#39104=CARTESIAN_POINT('Ctrl Pts',(5.7299307791557,-98.0117511126202,9.92453123330913));
#39105=CARTESIAN_POINT('Ctrl Pts',(8.59489616871569,-97.8367511126202,4.96226561664425));
#39106=CARTESIAN_POINT('Ctrl Pts',(11.4598615582757,-97.6617511126202,-2.06354052510241E-11));
#39107=CARTESIAN_POINT('Ctrl Pts',(8.59489616869782,-97.4867511126202,-4.9622656166752));
#39108=CARTESIAN_POINT('Ctrl Pts',(5.72993077911996,-97.3117511126202,-9.92453123332976));
#39109=CARTESIAN_POINT('Ctrl Pts',(-1.78726082715848E-11,-97.1367511126202,
-9.92453123331945));
#39110=CARTESIAN_POINT('Ctrl Pts',(-5.7299307791557,-96.9617511126202,-9.92453123330913));
#39111=CARTESIAN_POINT('Ctrl Pts',(-8.59489616871569,-96.7867511126202,
-4.96226561664425));
#39112=CARTESIAN_POINT('Ctrl Pts',(-11.4598615582757,-96.6117511126202,
2.06368086793017E-11));
#39113=CARTESIAN_POINT('Ctrl Pts',(-8.59489616869782,-96.4367511126202,
4.9622656166752));
#39114=CARTESIAN_POINT('Ctrl Pts',(-5.72993077911996,-96.2617511126202,
9.92453123332977));
#39115=CARTESIAN_POINT('Ctrl Pts',(1.7871392867044E-11,-96.0867511126202,
9.92453123331945));
#39116=CARTESIAN_POINT('Ctrl Pts',(5.7299307791557,-95.9117511126202,9.92453123330913));
#39117=CARTESIAN_POINT('Ctrl Pts',(8.59489616871569,-95.7367511126202,4.96226561664425));
#39118=CARTESIAN_POINT('Ctrl Pts',(11.4598615582757,-95.5617511126202,-2.06354052510241E-11));
#39119=CARTESIAN_POINT('Ctrl Pts',(8.59489616869782,-95.3867511126202,-4.9622656166752));
#39120=CARTESIAN_POINT('Ctrl Pts',(5.72993077911996,-95.2117511126202,-9.92453123332976));
#39121=CARTESIAN_POINT('Ctrl Pts',(-1.78726082715848E-11,-95.0367511126202,
-9.92453123331945));
#39122=CARTESIAN_POINT('Ctrl Pts',(-5.7299307791557,-94.8617511126203,-9.92453123330913));
#39123=CARTESIAN_POINT('Ctrl Pts',(-8.59489616871569,-94.6867511126202,
-4.96226561664425));
#39124=CARTESIAN_POINT('Ctrl Pts',(-11.4598615582757,-94.5117511126202,
2.06368086793017E-11));
#39125=CARTESIAN_POINT('Ctrl Pts',(-8.59489616869782,-94.3367511126202,
4.9622656166752));
#39126=CARTESIAN_POINT('Ctrl Pts',(-5.72993077911996,-94.1617511126202,
9.92453123332977));
#39127=CARTESIAN_POINT('Ctrl Pts',(1.7871392867044E-11,-93.9867511126202,
9.92453123331945));
#39128=CARTESIAN_POINT('Ctrl Pts',(5.7299307791557,-93.8117511126202,9.92453123330913));
#39129=CARTESIAN_POINT('Ctrl Pts',(8.59489616871569,-93.6367511126202,4.96226561664425));
#39130=CARTESIAN_POINT('Ctrl Pts',(11.4598615582757,-93.4617511126202,-2.06354052510241E-11));
#39131=CARTESIAN_POINT('Ctrl Pts',(8.59489616869782,-93.2867511126202,-4.9622656166752));
#39132=CARTESIAN_POINT('Ctrl Pts',(5.72993077911996,-93.1117511126202,-9.92453123332976));
#39133=CARTESIAN_POINT('Ctrl Pts',(-1.78726082715848E-11,-92.9367511126202,
-9.92453123331945));
#39134=CARTESIAN_POINT('Ctrl Pts',(-5.7299307791557,-92.7617511126202,-9.92453123330913));
#39135=CARTESIAN_POINT('Ctrl Pts',(-8.59489616871569,-92.5867511126202,
-4.96226561664425));
#39136=CARTESIAN_POINT('Ctrl Pts',(-11.4598615582757,-92.4117511126202,
2.06368086793017E-11));
#39137=CARTESIAN_POINT('Ctrl Pts',(-8.59489616869782,-92.2367511126202,
4.9622656166752));
#39138=CARTESIAN_POINT('Ctrl Pts',(-5.72993077911996,-92.0617511126202,
9.92453123332977));
#39139=CARTESIAN_POINT('Ctrl Pts',(1.7871392867044E-11,-91.8867511126202,
9.92453123331945));
#39140=CARTESIAN_POINT('Ctrl Pts',(5.7299307791557,-91.7117511126202,9.92453123330913));
#39141=CARTESIAN_POINT('Ctrl Pts',(8.59489616871569,-91.5367511126202,4.96226561664425));
#39142=CARTESIAN_POINT('Ctrl Pts',(11.4598615582757,-91.3617511126203,-2.06354052510241E-11));
#39143=CARTESIAN_POINT('Ctrl Pts',(8.59489616869782,-91.1867511126202,-4.9622656166752));
#39144=CARTESIAN_POINT('Ctrl Pts',(5.72993077911996,-91.0117511126202,-9.92453123332976));
#39145=CARTESIAN_POINT('Ctrl Pts',(-1.78726082715848E-11,-90.8367511126202,
-9.92453123331945));
#39146=CARTESIAN_POINT('Ctrl Pts',(-5.7299307791557,-90.6617511126203,-9.92453123330913));
#39147=CARTESIAN_POINT('Ctrl Pts',(-8.59489616871569,-90.4867511126203,
-4.96226561664425));
#39148=CARTESIAN_POINT('Ctrl Pts',(-11.4598615582757,-90.3117511126203,
2.06368086793017E-11));
#39149=CARTESIAN_POINT('Ctrl Pts',(-8.59489616869782,-90.1367511126202,
4.9622656166752));
#39150=CARTESIAN_POINT('Ctrl Pts',(-5.72993077911996,-89.9617511126202,
9.92453123332977));
#39151=CARTESIAN_POINT('Ctrl Pts',(1.7871392867044E-11,-89.7867511126202,
9.92453123331945));
#39152=CARTESIAN_POINT('Ctrl Pts',(5.7299307791557,-89.6117511126202,9.92453123330913));
#39153=CARTESIAN_POINT('Ctrl Pts',(8.59489616871569,-89.4367511126202,4.96226561664425));
#39154=CARTESIAN_POINT('Ctrl Pts',(11.4598615582757,-89.2617511126202,-2.06354052510241E-11));
#39155=CARTESIAN_POINT('Ctrl Pts',(8.59489616869782,-89.0867511126202,-4.9622656166752));
#39156=CARTESIAN_POINT('Ctrl Pts',(5.72993077911996,-88.9117511126203,-9.92453123332976));
#39157=CARTESIAN_POINT('Ctrl Pts',(-1.78726082715848E-11,-88.7367511126203,
-9.92453123331945));
#39158=CARTESIAN_POINT('Ctrl Pts',(-5.7299307791557,-88.5617511126202,-9.92453123330913));
#39159=CARTESIAN_POINT('Ctrl Pts',(-8.59489616871569,-88.3867511126203,
-4.96226561664425));
#39160=CARTESIAN_POINT('Ctrl Pts',(-11.4598615582757,-88.2117511126202,
2.06368086793017E-11));
#39161=CARTESIAN_POINT('Ctrl Pts',(-8.59489616869782,-88.0367511126202,
4.9622656166752));
#39162=CARTESIAN_POINT('Ctrl Pts',(-5.72993077911996,-87.8617511126202,
9.92453123332977));
#39163=CARTESIAN_POINT('Ctrl Pts',(1.7871392867044E-11,-87.6867511126203,
9.92453123331945));
#39164=CARTESIAN_POINT('Ctrl Pts',(5.7299307791557,-87.5117511126203,9.92453123330913));
#39165=CARTESIAN_POINT('Ctrl Pts',(8.59489616871569,-87.3367511126202,4.96226561664425));
#39166=CARTESIAN_POINT('Ctrl Pts',(11.4598615582757,-87.1617511126203,-2.06354052510241E-11));
#39167=CARTESIAN_POINT('Ctrl Pts',(8.59489616869782,-86.9867511126203,-4.9622656166752));
#39168=CARTESIAN_POINT('Ctrl Pts',(5.72993077911996,-86.8117511126202,-9.92453123332976));
#39169=CARTESIAN_POINT('Ctrl Pts',(-1.78726082715848E-11,-86.6367511126203,
-9.92453123331945));
#39170=CARTESIAN_POINT('Ctrl Pts',(-5.7299307791557,-86.4617511126202,-9.92453123330913));
#39171=CARTESIAN_POINT('Ctrl Pts',(-8.59489616871569,-86.2867511126203,
-4.96226561664425));
#39172=CARTESIAN_POINT('Ctrl Pts',(-11.4598615582757,-86.1117511126203,
2.06368086793017E-11));
#39173=CARTESIAN_POINT('Ctrl Pts',(-8.59489616869782,-85.9367511126203,
4.9622656166752));
#39174=CARTESIAN_POINT('Ctrl Pts',(-5.72993077911996,-85.7617511126202,
9.92453123332977));
#39175=CARTESIAN_POINT('Ctrl Pts',(1.7871392867044E-11,-85.5867511126203,
9.92453123331945));
#39176=CARTESIAN_POINT('Ctrl Pts',(5.7299307791557,-85.4117511126203,9.92453123330913));
#39177=CARTESIAN_POINT('Ctrl Pts',(8.59489616871569,-85.2367511126202,4.96226561664425));
#39178=CARTESIAN_POINT('Ctrl Pts',(11.4598615582757,-85.0617511126203,-2.06354052510241E-11));
#39179=CARTESIAN_POINT('Ctrl Pts',(8.59489616869782,-84.8867511126203,-4.9622656166752));
#39180=CARTESIAN_POINT('Ctrl Pts',(5.72993077911996,-84.7117511126202,-9.92453123332976));
#39181=CARTESIAN_POINT('Ctrl Pts',(-1.78726082715848E-11,-84.5367511126202,
-9.92453123331945));
#39182=CARTESIAN_POINT('Ctrl Pts',(-5.7299307791557,-84.3617511126203,-9.92453123330913));
#39183=CARTESIAN_POINT('Ctrl Pts',(-8.59489616871569,-84.1867511126203,
-4.96226561664425));
#39184=CARTESIAN_POINT('Ctrl Pts',(-11.4598615582757,-84.0117511126203,
2.06368086793017E-11));
#39185=CARTESIAN_POINT('Ctrl Pts',(-8.59489616869782,-83.8367511126203,
4.9622656166752));
#39186=CARTESIAN_POINT('Ctrl Pts',(-5.72993077911996,-83.6617511126203,
9.92453123332977));
#39187=CARTESIAN_POINT('Ctrl Pts',(1.7871392867044E-11,-83.4867511126202,
9.92453123331945));
#39188=CARTESIAN_POINT('Ctrl Pts',(5.7299307791557,-83.3117511126203,9.92453123330913));
#39189=CARTESIAN_POINT('Ctrl Pts',(8.59489616871569,-83.1367511126203,4.96226561664425));
#39190=CARTESIAN_POINT('Ctrl Pts',(11.4598615582757,-82.9617511126203,-2.06354052510241E-11));
#39191=CARTESIAN_POINT('Ctrl Pts',(8.59489616869782,-82.7867511126203,-4.9622656166752));
#39192=CARTESIAN_POINT('Ctrl Pts',(5.72993077911996,-82.6117511126203,-9.92453123332976));
#39193=CARTESIAN_POINT('Ctrl Pts',(-1.78726082715848E-11,-82.4367511126202,
-9.92453123331945));
#39194=CARTESIAN_POINT('Ctrl Pts',(-5.7299307791557,-82.2617511126203,-9.92453123330913));
#39195=CARTESIAN_POINT('Ctrl Pts',(-8.59489616871569,-82.0867511126203,
-4.96226561664425));
#39196=CARTESIAN_POINT('Ctrl Pts',(-11.4598615582757,-81.9117511126203,
2.06368086793017E-11));
#39197=CARTESIAN_POINT('Ctrl Pts',(-8.59489616869782,-81.7367511126203,
4.9622656166752));
#39198=CARTESIAN_POINT('Ctrl Pts',(-5.72993077911996,-81.5617511126202,
9.92453123332977));
#39199=CARTESIAN_POINT('Ctrl Pts',(1.7871392867044E-11,-81.3867511126203,
9.92453123331945));
#39200=CARTESIAN_POINT('Ctrl Pts',(5.7299307791557,-81.2117511126203,9.92453123330913));
#39201=CARTESIAN_POINT('Ctrl Pts',(8.59489616871569,-81.0367511126203,4.96226561664425));
#39202=CARTESIAN_POINT('Ctrl Pts',(11.4598615582757,-80.8617511126203,-2.06354052510241E-11));
#39203=CARTESIAN_POINT('Ctrl Pts',(8.59489616869782,-80.6867511126203,-4.9622656166752));
#39204=CARTESIAN_POINT('Ctrl Pts',(5.72993077911996,-80.5117511126203,-9.92453123332976));
#39205=CARTESIAN_POINT('Ctrl Pts',(-1.78726082715848E-11,-80.3367511126203,
-9.92453123331945));
#39206=CARTESIAN_POINT('Ctrl Pts',(-5.7299307791557,-80.1617511126202,-9.92453123330913));
#39207=CARTESIAN_POINT('Ctrl Pts',(-8.59489616871569,-79.9867511126203,
-4.96226561664425));
#39208=CARTESIAN_POINT('Ctrl Pts',(-11.4598615582757,-79.8117511126203,
2.06368086793017E-11));
#39209=CARTESIAN_POINT('Ctrl Pts',(-8.59489616869782,-79.6367511126202,
4.9622656166752));
#39210=CARTESIAN_POINT('Ctrl Pts',(-5.72993077911996,-79.4617511126203,
9.92453123332977));
#39211=CARTESIAN_POINT('Ctrl Pts',(1.7871392867044E-11,-79.2867511126203,
9.92453123331945));
#39212=CARTESIAN_POINT('Ctrl Pts',(5.7299307791557,-79.1117511126203,9.92453123330913));
#39213=CARTESIAN_POINT('Ctrl Pts',(8.59489616871569,-78.9367511126203,4.96226561664425));
#39214=CARTESIAN_POINT('Ctrl Pts',(11.4598615582757,-78.7617511126203,-2.06354052510241E-11));
#39215=CARTESIAN_POINT('Ctrl Pts',(8.59489616869782,-78.5867511126203,-4.9622656166752));
#39216=CARTESIAN_POINT('Ctrl Pts',(5.72993077911996,-78.4117511126203,-9.92453123332976));
#39217=CARTESIAN_POINT('Ctrl Pts',(-1.78726082715848E-11,-78.2367511126203,
-9.92453123331945));
#39218=CARTESIAN_POINT('Ctrl Pts',(-5.7299307791557,-78.0617511126203,-9.92453123330913));
#39219=CARTESIAN_POINT('Ctrl Pts',(-8.59489616871569,-77.8867511126203,
-4.96226561664425));
#39220=CARTESIAN_POINT('Ctrl Pts',(-11.4598615582757,-77.7117511126203,
2.06368086793017E-11));
#39221=CARTESIAN_POINT('Ctrl Pts',(-8.59489616869782,-77.5367511126203,
4.9622656166752));
#39222=CARTESIAN_POINT('Ctrl Pts',(-5.72993077911996,-77.3617511126203,
9.92453123332977));
#39223=CARTESIAN_POINT('Ctrl Pts',(1.7871392867044E-11,-77.1867511126203,
9.92453123331945));
#39224=CARTESIAN_POINT('Ctrl Pts',(5.7299307791557,-77.0117511126203,9.92453123330913));
#39225=CARTESIAN_POINT('Ctrl Pts',(8.59489616871569,-76.8367511126203,4.96226561664425));
#39226=CARTESIAN_POINT('Ctrl Pts',(11.4598615582757,-76.6617511126203,-2.06354052510241E-11));
#39227=CARTESIAN_POINT('Ctrl Pts',(8.59489616869782,-76.4867511126203,-4.9622656166752));
#39228=CARTESIAN_POINT('Ctrl Pts',(5.72993077911996,-76.3117511126203,-9.92453123332976));
#39229=CARTESIAN_POINT('Ctrl Pts',(-1.78726082715848E-11,-76.1367511126203,
-9.92453123331945));
#39230=CARTESIAN_POINT('Ctrl Pts',(-5.7299307791557,-75.9617511126203,-9.92453123330913));
#39231=CARTESIAN_POINT('Ctrl Pts',(-8.59489616871569,-75.7867511126203,
-4.96226561664425));
#39232=CARTESIAN_POINT('Ctrl Pts',(-11.4598615582757,-75.6117511126203,
2.06368086793017E-11));
#39233=CARTESIAN_POINT('Ctrl Pts',(-8.59489616869782,-75.4367511126203,
4.9622656166752));
#39234=CARTESIAN_POINT('Ctrl Pts',(-5.72993077911996,-75.2617511126203,
9.92453123332977));
#39235=CARTESIAN_POINT('Ctrl Pts',(1.7871392867044E-11,-75.0867511126203,
9.92453123331945));
#39236=CARTESIAN_POINT('Ctrl Pts',(5.7299307791557,-74.9117511126203,9.92453123330913));
#39237=CARTESIAN_POINT('Ctrl Pts',(8.59489616871569,-74.7367511126203,4.96226561664425));
#39238=CARTESIAN_POINT('Ctrl Pts',(11.4598615582757,-74.5617511126203,-2.06354052510241E-11));
#39239=CARTESIAN_POINT('Ctrl Pts',(8.59489616869782,-74.3867511126203,-4.9622656166752));
#39240=CARTESIAN_POINT('Ctrl Pts',(5.72993077911996,-74.2117511126203,-9.92453123332976));
#39241=CARTESIAN_POINT('Ctrl Pts',(-1.78726082715848E-11,-74.0367511126203,
-9.92453123331945));
#39242=CARTESIAN_POINT('Ctrl Pts',(-5.7299307791557,-73.8617511126203,-9.92453123330913));
#39243=CARTESIAN_POINT('Ctrl Pts',(-8.59489616871569,-73.6867511126203,
-4.96226561664425));
#39244=CARTESIAN_POINT('Ctrl Pts',(-11.4598615582757,-73.5117511126203,
2.06368086793017E-11));
#39245=CARTESIAN_POINT('Ctrl Pts',(-8.59489616869782,-73.3367511126203,
4.9622656166752));
#39246=CARTESIAN_POINT('Ctrl Pts',(-5.72993077911996,-73.1617511126203,
9.92453123332977));
#39247=CARTESIAN_POINT('Ctrl Pts',(1.7871392867044E-11,-72.9867511126203,
9.92453123331945));
#39248=CARTESIAN_POINT('Ctrl Pts',(5.7299307791557,-72.8117511126203,9.92453123330913));
#39249=CARTESIAN_POINT('Ctrl Pts',(8.59489616871569,-72.6367511126203,4.96226561664425));
#39250=CARTESIAN_POINT('Ctrl Pts',(11.4598615582757,-72.4617511126203,-2.06354052510241E-11));
#39251=CARTESIAN_POINT('Ctrl Pts',(8.59489616869782,-72.2867511126203,-4.9622656166752));
#39252=CARTESIAN_POINT('Ctrl Pts',(5.72993077911996,-72.1117511126203,-9.92453123332976));
#39253=CARTESIAN_POINT('Ctrl Pts',(-1.78726082715848E-11,-71.9367511126203,
-9.92453123331945));
#39254=CARTESIAN_POINT('Ctrl Pts',(-5.7299307791557,-71.7617511126203,-9.92453123330913));
#39255=CARTESIAN_POINT('Ctrl Pts',(-8.59489616871569,-71.5867511126203,
-4.96226561664425));
#39256=CARTESIAN_POINT('Ctrl Pts',(-11.4598615582757,-71.4117511126203,
2.06368086793017E-11));
#39257=CARTESIAN_POINT('Ctrl Pts',(-8.59489616869782,-71.2367511126203,
4.9622656166752));
#39258=CARTESIAN_POINT('Ctrl Pts',(-5.72993077911996,-71.0617511126203,
9.92453123332977));
#39259=CARTESIAN_POINT('Ctrl Pts',(1.7871392867044E-11,-70.8867511126203,
9.92453123331945));
#39260=CARTESIAN_POINT('Ctrl Pts',(5.7299307791557,-70.7117511126203,9.92453123330913));
#39261=CARTESIAN_POINT('Ctrl Pts',(8.59489616871569,-70.5367511126203,4.96226561664425));
#39262=CARTESIAN_POINT('Ctrl Pts',(11.4598615582757,-70.3617511126203,-2.06354052510241E-11));
#39263=CARTESIAN_POINT('Ctrl Pts',(8.59489616869782,-70.1867511126203,-4.9622656166752));
#39264=CARTESIAN_POINT('Ctrl Pts',(5.72993077911996,-70.0117511126203,-9.92453123332976));
#39265=CARTESIAN_POINT('Ctrl Pts',(-1.78726082715848E-11,-69.8367511126203,
-9.92453123331945));
#39266=CARTESIAN_POINT('Ctrl Pts',(-5.7299307791557,-69.6617511126203,-9.92453123330913));
#39267=CARTESIAN_POINT('Ctrl Pts',(-8.59489616871569,-69.4867511126203,
-4.96226561664425));
#39268=CARTESIAN_POINT('Ctrl Pts',(-11.4598615582757,-69.3117511126203,
2.06368086793017E-11));
#39269=CARTESIAN_POINT('Ctrl Pts',(-8.59489616869782,-69.1367511126203,
4.9622656166752));
#39270=CARTESIAN_POINT('Ctrl Pts',(-5.72993077911996,-68.9617511126203,
9.92453123332977));
#39271=CARTESIAN_POINT('Ctrl Pts',(1.7871392867044E-11,-68.7867511126203,
9.92453123331945));
#39272=CARTESIAN_POINT('Ctrl Pts',(5.7299307791557,-68.6117511126203,9.92453123330913));
#39273=CARTESIAN_POINT('Ctrl Pts',(8.59489616871569,-68.4367511126203,4.96226561664425));
#39274=CARTESIAN_POINT('Ctrl Pts',(11.4598615582757,-68.2617511126203,-2.06354052510241E-11));
#39275=CARTESIAN_POINT('Ctrl Pts',(8.59489616869782,-68.0867511126203,-4.9622656166752));
#39276=CARTESIAN_POINT('Ctrl Pts',(5.72993077911996,-67.9117511126203,-9.92453123332976));
#39277=CARTESIAN_POINT('Ctrl Pts',(-1.78726082715848E-11,-67.7367511126203,
-9.92453123331945));
#39278=CARTESIAN_POINT('Ctrl Pts',(-5.7299307791557,-67.5617511126203,-9.92453123330913));
#39279=CARTESIAN_POINT('Ctrl Pts',(-8.59489616871569,-67.3867511126203,
-4.96226561664425));
#39280=CARTESIAN_POINT('Ctrl Pts',(-11.4598615582757,-67.2117511126203,
2.06368086793017E-11));
#39281=CARTESIAN_POINT('Ctrl Pts',(-8.59489616869782,-67.0367511126203,
4.9622656166752));
#39282=CARTESIAN_POINT('Ctrl Pts',(-5.72993077911996,-66.8617511126203,
9.92453123332977));
#39283=CARTESIAN_POINT('Ctrl Pts',(1.7871392867044E-11,-66.6867511126203,
9.92453123331945));
#39284=CARTESIAN_POINT('Ctrl Pts',(5.7299307791557,-66.5117511126203,9.92453123330913));
#39285=CARTESIAN_POINT('Ctrl Pts',(8.59489616871569,-66.3367511126203,4.96226561664425));
#39286=CARTESIAN_POINT('Ctrl Pts',(11.4598615582757,-66.1617511126203,-2.06354052510241E-11));
#39287=CARTESIAN_POINT('Ctrl Pts',(8.59489616869782,-65.9867511126203,-4.9622656166752));
#39288=CARTESIAN_POINT('Ctrl Pts',(5.72993077911996,-65.8117511126203,-9.92453123332976));
#39289=CARTESIAN_POINT('Ctrl Pts',(-1.78726082715848E-11,-65.6367511126203,
-9.92453123331945));
#39290=CARTESIAN_POINT('Ctrl Pts',(-5.7299307791557,-65.4617511126203,-9.92453123330913));
#39291=CARTESIAN_POINT('Ctrl Pts',(-8.59489616871569,-65.2867511126203,
-4.96226561664425));
#39292=CARTESIAN_POINT('Ctrl Pts',(-11.4598615582757,-65.1117511126203,
2.06368086793017E-11));
#39293=CARTESIAN_POINT('Ctrl Pts',(-8.59489616869782,-64.9367511126203,
4.9622656166752));
#39294=CARTESIAN_POINT('Ctrl Pts',(-5.72993077911996,-64.7617511126203,
9.92453123332977));
#39295=CARTESIAN_POINT('Ctrl Pts',(1.7871392867044E-11,-64.5867511126203,
9.92453123331945));
#39296=CARTESIAN_POINT('Ctrl Pts',(5.7299307791557,-64.4117511126203,9.92453123330913));
#39297=CARTESIAN_POINT('Ctrl Pts',(8.59489616871569,-64.2367511126203,4.96226561664425));
#39298=CARTESIAN_POINT('Ctrl Pts',(11.4598615582757,-64.0617511126203,-2.06354052510241E-11));
#39299=CARTESIAN_POINT('Ctrl Pts',(8.59489616869782,-63.8867511126203,-4.9622656166752));
#39300=CARTESIAN_POINT('Ctrl Pts',(5.72993077911996,-63.7117511126203,-9.92453123332976));
#39301=CARTESIAN_POINT('Ctrl Pts',(-1.78726082715848E-11,-63.5367511126203,
-9.92453123331945));
#39302=CARTESIAN_POINT('Ctrl Pts',(-5.7299307791557,-63.3617511126203,-9.92453123330913));
#39303=CARTESIAN_POINT('Ctrl Pts',(-8.59489616871569,-63.1867511126203,
-4.96226561664425));
#39304=CARTESIAN_POINT('Ctrl Pts',(-11.4598615582757,-63.0117511126203,
2.06368086793017E-11));
#39305=CARTESIAN_POINT('Ctrl Pts',(-8.59489616869782,-62.8367511126203,
4.9622656166752));
#39306=CARTESIAN_POINT('Ctrl Pts',(-5.72993077911996,-62.6617511126203,
9.92453123332977));
#39307=CARTESIAN_POINT('Ctrl Pts',(1.7871392867044E-11,-62.4867511126203,
9.92453123331945));
#39308=CARTESIAN_POINT('Ctrl Pts',(5.7299307791557,-62.3117511126203,9.92453123330913));
#39309=CARTESIAN_POINT('Ctrl Pts',(8.59489616871569,-62.1367511126203,4.96226561664425));
#39310=CARTESIAN_POINT('Ctrl Pts',(11.4598615582757,-61.9617511126203,-2.06354052510241E-11));
#39311=CARTESIAN_POINT('Ctrl Pts',(8.59489616869782,-61.7867511126203,-4.9622656166752));
#39312=CARTESIAN_POINT('Ctrl Pts',(5.72993077911996,-61.6117511126203,-9.92453123332976));
#39313=CARTESIAN_POINT('Ctrl Pts',(-1.78726082715848E-11,-61.4367511126203,
-9.92453123331945));
#39314=CARTESIAN_POINT('Ctrl Pts',(-5.7299307791557,-61.2617511126203,-9.92453123330913));
#39315=CARTESIAN_POINT('Ctrl Pts',(-8.59489616871569,-61.0867511126203,
-4.96226561664425));
#39316=CARTESIAN_POINT('Ctrl Pts',(-11.4598615582757,-60.9117511126203,
2.06368086793017E-11));
#39317=CARTESIAN_POINT('Ctrl Pts',(-8.59489616869782,-60.7367511126203,
4.9622656166752));
#39318=CARTESIAN_POINT('Ctrl Pts',(-5.72993077911996,-60.5617511126203,
9.92453123332977));
#39319=CARTESIAN_POINT('Ctrl Pts',(1.7871392867044E-11,-60.3867511126203,
9.92453123331945));
#39320=CARTESIAN_POINT('Ctrl Pts',(5.7299307791557,-60.2117511126203,9.92453123330913));
#39321=CARTESIAN_POINT('Ctrl Pts',(8.59489616871569,-60.0367511126203,4.96226561664425));
#39322=CARTESIAN_POINT('Ctrl Pts',(11.4598615582757,-59.8617511126203,-2.06354052510241E-11));
#39323=CARTESIAN_POINT('Ctrl Pts',(8.59489616869782,-59.6867511126203,-4.9622656166752));
#39324=CARTESIAN_POINT('Ctrl Pts',(5.72993077911996,-59.5117511126203,-9.92453123332976));
#39325=CARTESIAN_POINT('Ctrl Pts',(-1.78726082715848E-11,-59.3367511126203,
-9.92453123331945));
#39326=CARTESIAN_POINT('Ctrl Pts',(-5.7299307791557,-59.1617511126203,-9.92453123330913));
#39327=CARTESIAN_POINT('Ctrl Pts',(-8.59489616871569,-58.9867511126203,
-4.96226561664425));
#39328=CARTESIAN_POINT('Ctrl Pts',(-11.4598615582757,-58.8117511126203,
2.06368086793017E-11));
#39329=CARTESIAN_POINT('Ctrl Pts',(-8.59489616869782,-58.6367511126203,
4.9622656166752));
#39330=CARTESIAN_POINT('Ctrl Pts',(-5.72993077911996,-58.4617511126203,
9.92453123332977));
#39331=CARTESIAN_POINT('Ctrl Pts',(1.7871392867044E-11,-58.2867511126203,
9.92453123331945));
#39332=CARTESIAN_POINT('Ctrl Pts',(5.7299307791557,-58.1117511126203,9.92453123330913));
#39333=CARTESIAN_POINT('Ctrl Pts',(8.59489616871569,-57.9367511126203,4.96226561664425));
#39334=CARTESIAN_POINT('Ctrl Pts',(11.4598615582757,-57.7617511126203,-2.06354052510241E-11));
#39335=CARTESIAN_POINT('Ctrl Pts',(8.59489616869782,-57.5867511126203,-4.9622656166752));
#39336=CARTESIAN_POINT('Ctrl Pts',(5.72993077911996,-57.4117511126203,-9.92453123332976));
#39337=CARTESIAN_POINT('Ctrl Pts',(-1.78726082715848E-11,-57.2367511126203,
-9.92453123331945));
#39338=CARTESIAN_POINT('Ctrl Pts',(-5.7299307791557,-57.0617511126203,-9.92453123330913));
#39339=CARTESIAN_POINT('Ctrl Pts',(-8.59489616871569,-56.8867511126203,
-4.96226561664425));
#39340=CARTESIAN_POINT('Ctrl Pts',(-11.4598615582757,-56.7117511126203,
2.06368086793017E-11));
#39341=CARTESIAN_POINT('Ctrl Pts',(-8.59489616869782,-56.5367511126203,
4.9622656166752));
#39342=CARTESIAN_POINT('Ctrl Pts',(-5.72993077911996,-56.3617511126203,
9.92453123332977));
#39343=CARTESIAN_POINT('Ctrl Pts',(1.7871392867044E-11,-56.1867511126203,
9.92453123331945));
#39344=CARTESIAN_POINT('Ctrl Pts',(5.7299307791557,-56.0117511126203,9.92453123330913));
#39345=CARTESIAN_POINT('Ctrl Pts',(8.59489616871569,-55.8367511126203,4.96226561664425));
#39346=CARTESIAN_POINT('Ctrl Pts',(11.4598615582757,-55.6617511126203,-2.06354052510241E-11));
#39347=CARTESIAN_POINT('Ctrl Pts',(8.59489616869782,-55.4867511126203,-4.9622656166752));
#39348=CARTESIAN_POINT('Ctrl Pts',(5.72993077911996,-55.3117511126203,-9.92453123332976));
#39349=CARTESIAN_POINT('Ctrl Pts',(-1.78726082715848E-11,-55.1367511126203,
-9.92453123331945));
#39350=CARTESIAN_POINT('Ctrl Pts',(-5.7299307791557,-54.9617511126203,-9.92453123330913));
#39351=CARTESIAN_POINT('Ctrl Pts',(-8.59489616871569,-54.7867511126203,
-4.96226561664425));
#39352=CARTESIAN_POINT('Ctrl Pts',(-11.4598615582757,-54.6117511126203,
2.06368086793017E-11));
#39353=CARTESIAN_POINT('Ctrl Pts',(-8.59489616869782,-54.4367511126203,
4.9622656166752));
#39354=CARTESIAN_POINT('Ctrl Pts',(-5.72993077911996,-54.2617511126203,
9.92453123332977));
#39355=CARTESIAN_POINT('Ctrl Pts',(1.7871392867044E-11,-54.0867511126203,
9.92453123331945));
#39356=CARTESIAN_POINT('Ctrl Pts',(5.7299307791557,-53.9117511126203,9.92453123330913));
#39357=CARTESIAN_POINT('Ctrl Pts',(8.59489616871569,-53.7367511126203,4.96226561664425));
#39358=CARTESIAN_POINT('Ctrl Pts',(11.4598615582757,-53.5617511126203,-2.06354052510241E-11));
#39359=CARTESIAN_POINT('Ctrl Pts',(8.59489616869782,-53.3867511126203,-4.9622656166752));
#39360=CARTESIAN_POINT('Ctrl Pts',(5.72993077911996,-53.2117511126203,-9.92453123332976));
#39361=CARTESIAN_POINT('Ctrl Pts',(-1.78726082715848E-11,-53.0367511126203,
-9.92453123331945));
#39362=CARTESIAN_POINT('Ctrl Pts',(-5.7299307791557,-52.8617511126203,-9.92453123330913));
#39363=CARTESIAN_POINT('Ctrl Pts',(-8.59489616871569,-52.6867511126203,
-4.96226561664425));
#39364=CARTESIAN_POINT('Ctrl Pts',(-11.4598615582757,-52.5117511126203,
2.06368086793017E-11));
#39365=CARTESIAN_POINT('Ctrl Pts',(-8.59489616869782,-52.3367511126203,
4.9622656166752));
#39366=CARTESIAN_POINT('Ctrl Pts',(-5.72993077911996,-52.1617511126203,
9.92453123332977));
#39367=CARTESIAN_POINT('Ctrl Pts',(1.7871392867044E-11,-51.9867511126203,
9.92453123331945));
#39368=CARTESIAN_POINT('Ctrl Pts',(5.7299307791557,-51.8117511126203,9.92453123330913));
#39369=CARTESIAN_POINT('Ctrl Pts',(8.59489616871569,-51.6367511126203,4.96226561664425));
#39370=CARTESIAN_POINT('Ctrl Pts',(11.4598615582757,-51.4617511126203,-2.06354052510241E-11));
#39371=CARTESIAN_POINT('Ctrl Pts',(8.59489616869782,-51.2867511126203,-4.9622656166752));
#39372=CARTESIAN_POINT('Ctrl Pts',(5.72993077911996,-51.1117511126203,-9.92453123332976));
#39373=CARTESIAN_POINT('Ctrl Pts',(-1.78726082715848E-11,-50.9367511126203,
-9.92453123331945));
#39374=CARTESIAN_POINT('Ctrl Pts',(-5.7299307791557,-50.7617511126203,-9.92453123330913));
#39375=CARTESIAN_POINT('Ctrl Pts',(-8.59489616871569,-50.5867511126203,
-4.96226561664425));
#39376=CARTESIAN_POINT('Ctrl Pts',(-11.4598615582757,-50.4117511126203,
2.06368086793017E-11));
#39377=CARTESIAN_POINT('Ctrl Pts',(-8.59489616869782,-50.2367511126203,
4.9622656166752));
#39378=CARTESIAN_POINT('Ctrl Pts',(-5.72993077911996,-50.0617511126203,
9.92453123332977));
#39379=CARTESIAN_POINT('Ctrl Pts',(1.7871392867044E-11,-49.8867511126203,
9.92453123331945));
#39380=CARTESIAN_POINT('Ctrl Pts',(5.7299307791557,-49.7117511126203,9.92453123330913));
#39381=CARTESIAN_POINT('Ctrl Pts',(8.59489616871569,-49.5367511126204,4.96226561664425));
#39382=CARTESIAN_POINT('Ctrl Pts',(11.4598615582757,-49.3617511126203,-2.06354052510241E-11));
#39383=CARTESIAN_POINT('Ctrl Pts',(8.59489616869782,-49.1867511126203,-4.9622656166752));
#39384=CARTESIAN_POINT('Ctrl Pts',(5.72993077911996,-49.0117511126203,-9.92453123332976));
#39385=CARTESIAN_POINT('Ctrl Pts',(-1.78726082715848E-11,-48.8367511126203,
-9.92453123331945));
#39386=CARTESIAN_POINT('Ctrl Pts',(-5.7299307791557,-48.6617511126203,-9.92453123330913));
#39387=CARTESIAN_POINT('Ctrl Pts',(-8.59489616871569,-48.4867511126203,
-4.96226561664425));
#39388=CARTESIAN_POINT('Ctrl Pts',(-11.4598615582757,-48.3117511126203,
2.06368086793017E-11));
#39389=CARTESIAN_POINT('Ctrl Pts',(-8.59489616869782,-48.1367511126203,
4.9622656166752));
#39390=CARTESIAN_POINT('Ctrl Pts',(-5.72993077911996,-47.9617511126203,
9.92453123332977));
#39391=CARTESIAN_POINT('Ctrl Pts',(1.7871392867044E-11,-47.7867511126204,
9.92453123331945));
#39392=CARTESIAN_POINT('Ctrl Pts',(5.7299307791557,-47.6117511126203,9.92453123330913));
#39393=CARTESIAN_POINT('Ctrl Pts',(8.59489616871569,-47.4367511126203,4.96226561664425));
#39394=CARTESIAN_POINT('Ctrl Pts',(11.4598615582757,-47.2617511126203,-2.06354052510241E-11));
#39395=CARTESIAN_POINT('Ctrl Pts',(8.59489616869782,-47.0867511126203,-4.9622656166752));
#39396=CARTESIAN_POINT('Ctrl Pts',(5.72993077911996,-46.9117511126203,-9.92453123332976));
#39397=CARTESIAN_POINT('Ctrl Pts',(-1.78726082715848E-11,-46.7367511126204,
-9.92453123331945));
#39398=CARTESIAN_POINT('Ctrl Pts',(-5.7299307791557,-46.5617511126203,-9.92453123330913));
#39399=CARTESIAN_POINT('Ctrl Pts',(-8.59489616871569,-46.3867511126203,
-4.96226561664425));
#39400=CARTESIAN_POINT('Ctrl Pts',(-11.4598615582757,-46.2117511126204,
2.06368086793017E-11));
#39401=CARTESIAN_POINT('Ctrl Pts',(-8.59489616869782,-46.0367511126203,
4.9622656166752));
#39402=CARTESIAN_POINT('Ctrl Pts',(-5.72993077911996,-45.8617511126203,
9.92453123332977));
#39403=CARTESIAN_POINT('Ctrl Pts',(1.7871392867044E-11,-45.6867511126204,
9.92453123331945));
#39404=CARTESIAN_POINT('Ctrl Pts',(5.7299307791557,-45.5117511126203,9.92453123330913));
#39405=CARTESIAN_POINT('Ctrl Pts',(8.59489616871569,-45.3367511126203,4.96226561664425));
#39406=CARTESIAN_POINT('Ctrl Pts',(11.4598615582757,-45.1617511126204,-2.06354052510241E-11));
#39407=CARTESIAN_POINT('Ctrl Pts',(8.59489616869782,-44.9867511126203,-4.9622656166752));
#39408=CARTESIAN_POINT('Ctrl Pts',(5.72993077911996,-44.8117511126203,-9.92453123332976));
#39409=CARTESIAN_POINT('Ctrl Pts',(-1.78726082715848E-11,-44.6367511126204,
-9.92453123331945));
#39410=CARTESIAN_POINT('Ctrl Pts',(-5.7299307791557,-44.4617511126204,-9.92453123330913));
#39411=CARTESIAN_POINT('Ctrl Pts',(-8.59489616871569,-44.2867511126203,
-4.96226561664425));
#39412=CARTESIAN_POINT('Ctrl Pts',(-11.4598615582757,-44.1117511126203,
2.06368086793017E-11));
#39413=CARTESIAN_POINT('Ctrl Pts',(-8.59489616869782,-43.9367511126204,
4.9622656166752));
#39414=CARTESIAN_POINT('Ctrl Pts',(-5.72993077911996,-43.7617511126204,
9.92453123332977));
#39415=CARTESIAN_POINT('Ctrl Pts',(1.7871392867044E-11,-43.5867511126203,
9.92453123331945));
#39416=CARTESIAN_POINT('Ctrl Pts',(5.7299307791557,-43.4117511126204,9.92453123330913));
#39417=CARTESIAN_POINT('Ctrl Pts',(8.59489616871569,-43.2367511126203,4.96226561664425));
#39418=CARTESIAN_POINT('Ctrl Pts',(11.4598615582757,-43.0617511126203,-2.06354052510241E-11));
#39419=CARTESIAN_POINT('Ctrl Pts',(8.59489616869782,-42.8867511126204,-4.9622656166752));
#39420=CARTESIAN_POINT('Ctrl Pts',(5.72993077911996,-42.7117511126203,-9.92453123332976));
#39421=CARTESIAN_POINT('Ctrl Pts',(-1.78726082715848E-11,-42.5367511126203,
-9.92453123331945));
#39422=CARTESIAN_POINT('Ctrl Pts',(-0.219644606349529,-212.63,-9.92210040505701));
#39423=CARTESIAN_POINT('Ctrl Pts',(-1.4533920550627,-212.63,-9.8213661461777));
#39424=CARTESIAN_POINT('Ctrl Pts',(-2.65597646823175,-212.63,-9.48288190087395));
#39425=CARTESIAN_POINT('Ctrl Pts',(-4.86098942222034,-212.63,-8.36949832183372));
#39426=CARTESIAN_POINT('Ctrl Pts',(-5.8434616897038,-212.63,-7.60704909264757));
#39427=CARTESIAN_POINT('Ctrl Pts',(-7.32939714963465,-212.63,-5.90751715922259));
#39428=CARTESIAN_POINT('Ctrl Pts',(-7.99853353868902,-212.63,-4.89381432117256));
#39429=CARTESIAN_POINT('Ctrl Pts',(-8.80359152553002,-212.63,-2.62789349339889));
#39430=CARTESIAN_POINT('Ctrl Pts',(-8.97717635487367,-212.63,-1.54602428959771));
#39431=CARTESIAN_POINT('Ctrl Pts',(-8.92442457723671,-212.63,0.700721770435771));
#39432=CARTESIAN_POINT('Ctrl Pts',(-8.67060378400234,-212.63,1.84439401565503));
#39433=CARTESIAN_POINT('Ctrl Pts',(-7.91777274084501,-212.63,3.56131387525748));
#39434=CARTESIAN_POINT('Ctrl Pts',(-7.5464292751167,-212.630000000324,4.19442289602148));
#39435=CARTESIAN_POINT('Ctrl Pts',(-6.6871605411885,-212.630000000324,5.2990234415664));
#39436=CARTESIAN_POINT('Ctrl Pts',(-6.20599255820334,-212.63,5.78118301177607));
#39437=CARTESIAN_POINT('Ctrl Pts',(-5.67113674141197,-212.63,6.19885209091273));
#39438=CARTESIAN_POINT('Origin',(0.,-212.63,9.93750000000001));
#39439=CARTESIAN_POINT('Origin',(-10.8677182860469,-15.875,-3.00462919747432E-15));
#39440=CARTESIAN_POINT('',(-10.8677182860469,-15.875,-6.27448007792623));
#39441=CARTESIAN_POINT('',(-10.8677182860469,-0.848960155852393,-6.27448007792623));
#39442=CARTESIAN_POINT('',(-10.8677182860469,-15.875,-6.27448007792623));
#39443=CARTESIAN_POINT('',(-10.8677182860469,-15.875,6.27448007792622));
#39444=CARTESIAN_POINT('',(-10.8677182860469,-15.875,-3.00462919747432E-15));
#39445=CARTESIAN_POINT('',(-10.8677182860469,-0.848960155852389,6.27448007792622));
#39446=CARTESIAN_POINT('',(-10.8677182860469,-15.875,6.27448007792622));
#39447=CARTESIAN_POINT('',(-10.8677182860469,0.,4.33390115890082));
#39448=CARTESIAN_POINT('Ctrl Pts',(-10.8677182860469,4.31956443403523E-15,
4.33390115890082));
#39449=CARTESIAN_POINT('Ctrl Pts',(-10.8677182860469,-0.34683042785844,
5.27022062193468));
#39450=CARTESIAN_POINT('Ctrl Pts',(-10.8677182860469,-0.848960155837252,
6.27448007789594));
#39451=CARTESIAN_POINT('',(-10.8677182860469,0.,-4.33390115890083));
#39452=CARTESIAN_POINT('',(-10.8677182860469,0.,-3.00462919747432E-15));
#39453=CARTESIAN_POINT('Ctrl Pts',(-10.8677182860469,-0.84896015583725,
-6.27448007789595));
#39454=CARTESIAN_POINT('Ctrl Pts',(-10.8677182860469,-0.346830427858437,
-5.27022062193468));
#39455=CARTESIAN_POINT('Ctrl Pts',(-10.8677182860469,6.60639266381858E-15,
-4.33390115890082));
#39456=CARTESIAN_POINT('Origin',(-5.43385914302348,-15.875,9.41172011688933));
#39457=CARTESIAN_POINT('',(-6.07153216591882E-15,-15.875,12.5489601558524));
#39458=CARTESIAN_POINT('',(-5.43385914302348,-15.875,9.41172011688933));
#39459=CARTESIAN_POINT('',(-6.07153216591882E-15,-0.848960155852391,12.5489601558524));
#39460=CARTESIAN_POINT('',(-6.07153216591882E-15,-15.875,12.5489601558524));
#39461=CARTESIAN_POINT('',(-1.68059064192455,0.,11.5786706963397));
#39462=CARTESIAN_POINT('Ctrl Pts',(-1.68059064192455,2.28682822978336E-15,
11.5786706963397));
#39463=CARTESIAN_POINT('Ctrl Pts',(-0.869714200879427,-0.34683042785844,
12.0468304278567));
#39464=CARTESIAN_POINT('Ctrl Pts',(-2.62300655575992E-11,-0.848960155837252,
12.5489601558373));
#39465=CARTESIAN_POINT('',(-9.18712764412241,0.,7.24476953743892));
#39466=CARTESIAN_POINT('',(-5.43385914302348,0.,9.41172011688933));
#39467=CARTESIAN_POINT('Ctrl Pts',(-10.8677182860207,-0.848960155837241,
6.27448007794137));
#39468=CARTESIAN_POINT('Ctrl Pts',(-9.99800408516752,-0.346830427858434,
6.776609805922));
#39469=CARTESIAN_POINT('Ctrl Pts',(-9.1871276441224,4.82774848509819E-15,
7.24476953743893));
#39470=CARTESIAN_POINT('Origin',(5.43385914302347,-15.875,9.41172011688934));
#39471=CARTESIAN_POINT('',(10.8677182860469,-15.875,6.27448007792623));
#39472=CARTESIAN_POINT('',(5.43385914302347,-15.875,9.41172011688934));
#39473=CARTESIAN_POINT('',(10.8677182860469,-0.848960155852389,6.27448007792623));
#39474=CARTESIAN_POINT('',(10.8677182860469,-15.875,6.27448007792623));
#39475=CARTESIAN_POINT('',(9.1871276441224,0.,7.24476953743893));
#39476=CARTESIAN_POINT('Ctrl Pts',(9.1871276441224,0.,7.24476953743893));
#39477=CARTESIAN_POINT('Ctrl Pts',(9.99800408516752,-0.346830427858443,
6.776609805922));
#39478=CARTESIAN_POINT('Ctrl Pts',(10.8677182860207,-0.848960155837255,
6.27448007794137));
#39479=CARTESIAN_POINT('',(1.68059064192454,0.,11.5786706963397));
#39480=CARTESIAN_POINT('',(5.43385914302347,0.,9.41172011688934));
#39481=CARTESIAN_POINT('Ctrl Pts',(2.6228483654321E-11,-0.848960155837241,
12.5489601558373));
#39482=CARTESIAN_POINT('Ctrl Pts',(0.869714200879426,-0.34683042785843,
12.0468304278567));
#39483=CARTESIAN_POINT('Ctrl Pts',(1.68059064192455,1.11800491233853E-14,
11.5786706963397));
#39484=CARTESIAN_POINT('Origin',(10.8677182860469,-15.875,0.));
#39485=CARTESIAN_POINT('',(10.8677182860469,-15.875,-6.27448007792623));
#39486=CARTESIAN_POINT('',(10.8677182860469,-15.875,0.));
#39487=CARTESIAN_POINT('',(10.8677182860469,-0.848960155852391,-6.27448007792623));
#39488=CARTESIAN_POINT('',(10.8677182860469,-15.875,-6.27448007792623));
#39489=CARTESIAN_POINT('',(10.8677182860469,0.,-4.33390115890083));
#39490=CARTESIAN_POINT('Ctrl Pts',(10.8677182860469,3.0491043063778E-15,
-4.33390115890084));
#39491=CARTESIAN_POINT('Ctrl Pts',(10.8677182860469,-0.346830427858442,
-5.27022062193469));
#39492=CARTESIAN_POINT('Ctrl Pts',(10.8677182860469,-0.848960155837254,
-6.27448007789596));
#39493=CARTESIAN_POINT('',(10.8677182860469,0.,4.33390115890083));
#39494=CARTESIAN_POINT('',(10.8677182860469,0.,0.));
#39495=CARTESIAN_POINT('Ctrl Pts',(10.8677182860469,-0.848960155837236,
6.27448007789593));
#39496=CARTESIAN_POINT('Ctrl Pts',(10.8677182860469,-0.346830427858437,
5.27022062193468));
#39497=CARTESIAN_POINT('Ctrl Pts',(10.8677182860469,1.27046012765742E-15,
4.33390115890084));
#39498=CARTESIAN_POINT('Origin',(5.43385914302348,-15.875,-9.41172011688934));
#39499=CARTESIAN_POINT('',(3.46944695195361E-15,-15.875,-12.5489601558525));
#39500=CARTESIAN_POINT('',(5.43385914302348,-15.875,-9.41172011688934));
#39501=CARTESIAN_POINT('',(3.46944695195361E-15,-15.875,-12.5489601558525));
#39502=CARTESIAN_POINT('',(9.18712764412239,0.,-7.24476953743894));
#39503=CARTESIAN_POINT('',(5.43385914302348,0.,-9.41172011688934));
#39504=CARTESIAN_POINT('Ctrl Pts',(10.8677182860207,-0.848960155837252,
-6.27448007794137));
#39505=CARTESIAN_POINT('Ctrl Pts',(9.99800408516752,-0.346830427858437,
-6.77660980592201));
#39506=CARTESIAN_POINT('Ctrl Pts',(9.18712764412239,6.60639266381857E-15,
-7.24476953743894));
#39507=CARTESIAN_POINT('Origin',(-5.43385914302347,-15.875,-9.41172011688934));
#39508=CARTESIAN_POINT('',(-5.43385914302347,-15.875,-9.41172011688934));
#39509=CARTESIAN_POINT('',(-9.18712764412239,0.,-7.24476953743893));
#39510=CARTESIAN_POINT('Ctrl Pts',(-9.18712764412239,2.54092025531484E-15,
-7.24476953743893));
#39511=CARTESIAN_POINT('Ctrl Pts',(-9.99800408516753,-0.346830427858443,
-6.776609805922));
#39512=CARTESIAN_POINT('Ctrl Pts',(-10.8677182860207,-0.848960155837259,
-6.27448007794136));
#39513=CARTESIAN_POINT('',(-5.43385914302347,0.,-9.41172011688934));
#39514=CARTESIAN_POINT('Origin',(0.,-15.875,0.));
#39515=CARTESIAN_POINT('Origin',(0.,-0.999999999999945,0.));
#39516=CARTESIAN_POINT('Origin',(0.,0.,0.));
#39517=CARTESIAN_POINT('Origin',(0.,-0.999999999999945,0.));
#39518=CARTESIAN_POINT('Origin',(0.,0.,0.));
#39519=CARTESIAN_POINT('Origin',(0.,-0.999999999999945,0.));
#39520=CARTESIAN_POINT('Origin',(0.,0.,0.));
#39521=CARTESIAN_POINT('Origin',(0.,-0.999999999999945,0.));
#39522=CARTESIAN_POINT('Origin',(0.,0.,0.));
#39523=CARTESIAN_POINT('Origin',(0.,-0.999999999999945,0.));
#39524=CARTESIAN_POINT('Origin',(0.,0.,0.));
#39525=CARTESIAN_POINT('Origin',(0.,0.,0.));
#39526=CARTESIAN_POINT('Ctrl Pts',(-0.194315056459259,-26.7212227391133,
-12.1981274139594));
#39527=CARTESIAN_POINT('Ctrl Pts',(-0.203067890482931,-26.7208823204558,
-12.6983912923613));
#39528=CARTESIAN_POINT('Ctrl Pts',(-0.222506667109496,-27.2208450130247,
-12.6980506686299));
#39529=CARTESIAN_POINT('Ctrl Pts',(0.134166779161007,-26.7339981836376,
-12.2044589641634));
#39530=CARTESIAN_POINT('Ctrl Pts',(0.139777617995481,-26.7347920529262,
-12.7038236374003));
#39531=CARTESIAN_POINT('Ctrl Pts',(0.153629648332412,-27.2348979165139,
-12.7046416675251));
#39532=CARTESIAN_POINT('Ctrl Pts',(0.472996743962122,-26.7137256552718,
-12.1943004586851));
#39533=CARTESIAN_POINT('Ctrl Pts',(0.496088949698769,-26.7124000235208,
-12.6949661157068));
#39534=CARTESIAN_POINT('Ctrl Pts',(0.541620041925868,-27.2125982196052,
-12.6940668718406));
#39535=CARTESIAN_POINT('Ctrl Pts',(1.13102669670067,-26.6067914943918,-12.1418208766917));
#39536=CARTESIAN_POINT('Ctrl Pts',(1.18251789112393,-26.5959733556708,-12.6500253820366));
#39537=CARTESIAN_POINT('Ctrl Pts',(1.29511827496423,-27.0949706450248,-12.6394364854779));
#39538=CARTESIAN_POINT('Ctrl Pts',(1.44820857041315,-26.5218354596063,-12.1003567529811));
#39539=CARTESIAN_POINT('Ctrl Pts',(1.51413351942913,-26.5025539703757,-12.6142304394117));
#39540=CARTESIAN_POINT('Ctrl Pts',(1.65831751887342,-27.0015190056013,-12.596273014076));
#39541=CARTESIAN_POINT('Ctrl Pts',(2.06065319481642,-26.2923457172244,-11.9924294251706));
#39542=CARTESIAN_POINT('Ctrl Pts',(2.1480929495222,-26.2540473941778,-12.5230572090411));
#39543=CARTESIAN_POINT('Ctrl Pts',(2.35961681393454,-26.7490802889125,-12.483922433672));
#39544=CARTESIAN_POINT('Ctrl Pts',(2.35854389520533,-26.145712314138,-11.9250475278437));
#39545=CARTESIAN_POINT('Ctrl Pts',(2.4554509163846,-26.09432187406,-12.4661578446707));
#39546=CARTESIAN_POINT('Ctrl Pts',(2.70072608321809,-26.5877835449747,-12.4137789851734));
#39547=CARTESIAN_POINT('Ctrl Pts',(2.9104768853475,-25.803547654477,-11.776582758216));
#39548=CARTESIAN_POINT('Ctrl Pts',(3.01814234426553,-25.727851383016,-12.3439902212264));
#39549=CARTESIAN_POINT('Ctrl Pts',(3.33273459746412,-26.2114024205019,-12.2592295912986));
#39550=CARTESIAN_POINT('Ctrl Pts',(3.16675759630227,-25.6078668562775,-11.6953386900839));
#39551=CARTESIAN_POINT('Ctrl Pts',(3.27655230794715,-25.5181571512881,-12.2779126330183));
#39552=CARTESIAN_POINT('Ctrl Pts',(3.62619701879906,-25.9961535423151,-12.1746558505725));
#39553=CARTESIAN_POINT('Ctrl Pts',(3.52278337011958,-25.2769360215998,-11.5690410381704));
#39554=CARTESIAN_POINT('Ctrl Pts',(3.62723458607873,-25.1735020601709,-12.1792044217791));
#39555=CARTESIAN_POINT('Ctrl Pts',(4.03387571115309,-25.6321296235549,-12.0431820637955));
#39556=CARTESIAN_POINT('Ctrl Pts',(3.63691595191385,-25.1599641836089,-11.5260929344709));
#39557=CARTESIAN_POINT('Ctrl Pts',(3.73963755328883,-25.0511426623102,-12.1457738319626));
#39558=CARTESIAN_POINT('Ctrl Pts',(4.16456687282794,-25.5034606017804,-11.9984737931225));
#39559=CARTESIAN_POINT('Ctrl Pts',(3.85121707642186,-24.9178456922059,-11.4415520283336));
#39560=CARTESIAN_POINT('Ctrl Pts',(3.94898113658373,-24.8000160592407,-12.0809829287729));
#39561=CARTESIAN_POINT('Ctrl Pts',(4.40995922601222,-25.2371302616159,-11.9104680943871));
#39562=CARTESIAN_POINT('Ctrl Pts',(3.95198070070556,-24.7922056825208,-11.3997592507804));
#39563=CARTESIAN_POINT('Ctrl Pts',(4.04625813149204,-24.6705623727243,-12.0494916609173));
#39564=CARTESIAN_POINT('Ctrl Pts',(4.52534183541223,-25.0989262507882,-11.8669624993707));
#39565=CARTESIAN_POINT('Ctrl Pts',(4.23558744018011,-24.401454308808,-11.2775109794014));
#39566=CARTESIAN_POINT('Ctrl Pts',(4.3203397283013,-24.2676859595634,-11.9580183198169));
#39567=CARTESIAN_POINT('Ctrl Pts',(4.85009479778453,-24.6690997396581,-11.7397040511128));
#39568=CARTESIAN_POINT('Ctrl Pts',(4.40029129520591,-24.1219950623208,-11.1999546753906));
#39569=CARTESIAN_POINT('Ctrl Pts',(4.47234649383105,-23.9871950107587,-11.9032777424555));
#39570=CARTESIAN_POINT('Ctrl Pts',(5.03869421244281,-24.3616945682431,-11.6589692124176));
#39571=CARTESIAN_POINT('Ctrl Pts',(4.67633642519072,-23.5250073471767,-11.0637813849082));
#39572=CARTESIAN_POINT('Ctrl Pts',(4.72346035897912,-23.401295578245,-11.8103646186347));
#39573=CARTESIAN_POINT('Ctrl Pts',(5.35478851329005,-23.7050080822041,-11.5172150470738));
#39574=CARTESIAN_POINT('Ctrl Pts',(4.78350043752076,-23.216754789204,-11.007350870447));
#39575=CARTESIAN_POINT('Ctrl Pts',(4.81587476821909,-23.1073726626684,-11.7745863820089));
#39576=CARTESIAN_POINT('Ctrl Pts',(5.47750009197968,-23.3659302682378,-11.458471808437));
#39577=CARTESIAN_POINT('Ctrl Pts',(4.89876860580401,-22.7393314761495,-10.9455338368082));
#39578=CARTESIAN_POINT('Ctrl Pts',(4.91470009013209,-22.6607732404412,-11.7361393743978));
#39579=CARTESIAN_POINT('Ctrl Pts',(5.6094915916466,-22.8407646237077,-11.3941212887981));
#39580=CARTESIAN_POINT('Ctrl Pts',(4.92955208184883,-22.5776667539846,-10.9287329128092));
#39581=CARTESIAN_POINT('Ctrl Pts',(4.94074128439299,-22.5103984492741,-11.725920546492));
#39582=CARTESIAN_POINT('Ctrl Pts',(5.64474119604575,-22.6629334294602,-11.3766318028864));
#39583=CARTESIAN_POINT('Ctrl Pts',(4.97523170289568,-22.2490170068924,-10.9036572997793));
#39584=CARTESIAN_POINT('Ctrl Pts',(4.97935760333758,-22.2060010603353,-11.7107367920172));
#39585=CARTESIAN_POINT('Ctrl Pts',(5.69704810501006,-22.3014187075044,-11.350528500382));
#39586=CARTESIAN_POINT('Ctrl Pts',(4.9900614685414,-22.0812569558744,-10.8954209365004));
#39587=CARTESIAN_POINT('Ctrl Pts',(4.99169258536863,-22.052002659175,-11.7058637040127));
#39588=CARTESIAN_POINT('Ctrl Pts',(5.71402940255624,-22.1168826514477,-11.3419545814996));
#39589=CARTESIAN_POINT('Ctrl Pts',(5.00902637313877,-21.5829271070114,-10.8848943478805));
#39590=CARTESIAN_POINT('Ctrl Pts',(5.0075744573728,-21.5937822825219,-11.6995920372639));
#39591=CARTESIAN_POINT('Ctrl Pts',(5.73574577388715,-21.5687198177408,-11.3309965751315));
#39592=CARTESIAN_POINT('Ctrl Pts',(4.98870840505789,-21.2534958170338,-10.8963611248835));
#39593=CARTESIAN_POINT('Ctrl Pts',(4.99120040430745,-21.2953972536494,-11.7061066151783));
#39594=CARTESIAN_POINT('Ctrl Pts',(5.71248003454301,-21.206345398664,-11.3429333016361));
#39595=CARTESIAN_POINT('Ctrl Pts',(4.90945823057519,-20.7634378238772,-10.9396841355917));
#39596=CARTESIAN_POINT('Ctrl Pts',(4.92366751892991,-20.838223666219,-11.7326137010596));
#39597=CARTESIAN_POINT('Ctrl Pts',(5.62173208850429,-20.6672816063015,-11.3880318463151));
#39598=CARTESIAN_POINT('Ctrl Pts',(4.87455989872081,-20.5998021506003,-10.9586262653569));
#39599=CARTESIAN_POINT('Ctrl Pts',(4.89400424310528,-20.6854463533553,-11.7442263723397));
#39600=CARTESIAN_POINT('Ctrl Pts',(5.58177063740257,-20.4872823658008,-11.4077502922669));
#39601=CARTESIAN_POINT('Ctrl Pts',(4.78945908598975,-20.2798404689652,-11.0039362410179));
#39602=CARTESIAN_POINT('Ctrl Pts',(4.82020327496675,-20.3830544594789,-11.7728329898822));
#39603=CARTESIAN_POINT('Ctrl Pts',(5.48432323279469,-20.1353245157212,-11.4549172348609));
#39604=CARTESIAN_POINT('Ctrl Pts',(4.73937502306188,-20.1234268906168,-11.030240976236));
#39605=CARTESIAN_POINT('Ctrl Pts',(4.77648918248447,-20.2339643104042,-11.789668542258));
#39606=CARTESIAN_POINT('Ctrl Pts',(5.42697287433976,-19.9632695797551,-11.4823000321756));
#39607=CARTESIAN_POINT('Ctrl Pts',(4.56731216496254,-19.6642943627305,-11.1183794655812));
#39608=CARTESIAN_POINT('Ctrl Pts',(4.62447523913058,-19.7943682502535,-11.8473111221715));
#39609=CARTESIAN_POINT('Ctrl Pts',(5.22994679958899,-19.4582237988502,-11.5740507560812));
#39610=CARTESIAN_POINT('Ctrl Pts',(4.4225017548533,-19.3696333894946,-11.1899943284984));
#39611=CARTESIAN_POINT('Ctrl Pts',(4.49417778960582,-19.5042750964007,-11.8958840070277));
#39612=CARTESIAN_POINT('Ctrl Pts',(5.06412700816816,-19.1340967289438,-11.6486006523686));
#39613=CARTESIAN_POINT('Ctrl Pts',(4.07922497844486,-18.8153269570627,-11.3466863829177));
#39614=CARTESIAN_POINT('Ctrl Pts',(4.17144753969082,-18.9460643318112,-12.0086673192177));
#39615=CARTESIAN_POINT('Ctrl Pts',(4.67104696430523,-18.5243596522693,-11.8117145144333));
#39616=CARTESIAN_POINT('Ctrl Pts',(3.88357483934998,-18.5592589877753,-11.4304872091369));
#39617=CARTESIAN_POINT('Ctrl Pts',(3.98456712315329,-18.6823627389427,-12.0711495294318));
#39618=CARTESIAN_POINT('Ctrl Pts',(4.44701151665401,-18.2426848863307,-11.8989497983692));
#39619=CARTESIAN_POINT('Ctrl Pts',(3.44456423424596,-18.08644988691,-11.599515766087));
#39620=CARTESIAN_POINT('Ctrl Pts',(3.55363139810777,-18.190115999482,-12.2017033779511));
#39621=CARTESIAN_POINT('Ctrl Pts',(3.94430838975052,-17.7225948758231,-12.0749057578065));
#39622=CARTESIAN_POINT('Ctrl Pts',(3.19881952916763,-17.8685825627143,-11.6853630222093));
#39623=CARTESIAN_POINT('Ctrl Pts',(3.30880170180714,-17.9587265964904,-12.2701736879534));
#39624=CARTESIAN_POINT('Ctrl Pts',(3.66291055880196,-17.4829408191597,-12.1642713417504));
#39625=CARTESIAN_POINT('Ctrl Pts',(2.67586340966611,-17.4889456042686,-11.8433556306518));
#39626=CARTESIAN_POINT('Ctrl Pts',(2.7799526126078,-17.5545379722142,-12.3984078601019));
#39627=CARTESIAN_POINT('Ctrl Pts',(3.06408293755109,-17.0653401645214,-12.3287390591788));
#39628=CARTESIAN_POINT('Ctrl Pts',(2.39714240324113,-17.3248873383762,-11.916286264565));
#39629=CARTESIAN_POINT('Ctrl Pts',(2.49456444142712,-17.3767916845148,-12.4592374659268));
#39630=CARTESIAN_POINT('Ctrl Pts',(2.74492453899815,-16.8848760712784,-12.4046586511814));
#39631=CARTESIAN_POINT('Ctrl Pts',(1.95126020128702,-17.1185475242902,-12.0108596275047));
#39632=CARTESIAN_POINT('Ctrl Pts',(2.03243224842994,-17.1527631933337,-12.538948153782));
#39633=CARTESIAN_POINT('Ctrl Pts',(2.23435286973199,-16.6579022771869,-12.5031079735321));
#39634=CARTESIAN_POINT('Ctrl Pts',(1.79708542715294,-17.0562076265249,-12.0400265737317));
#39635=CARTESIAN_POINT('Ctrl Pts',(1.87292847323085,-17.0851427079614,-12.5635973650709));
#39636=CARTESIAN_POINT('Ctrl Pts',(2.05781011604666,-16.5893283894317,-12.5334702855318));
#39637=CARTESIAN_POINT('Ctrl Pts',(1.48587265051063,-16.9480427335416,-12.0912569680729));
#39638=CARTESIAN_POINT('Ctrl Pts',(1.55038574292973,-16.9679145460432,-12.6069707100262));
#39639=CARTESIAN_POINT('Ctrl Pts',(1.70144597780252,-16.4703470066414,-12.5868002866746));
#39640=CARTESIAN_POINT('Ctrl Pts',(1.32830296766848,-16.9018752765432,-12.1134730678806));
#39641=CARTESIAN_POINT('Ctrl Pts',(1.38646382234108,-16.9176368740355,-12.6259247675388));
#39642=CARTESIAN_POINT('Ctrl Pts',(1.52101577525149,-16.4195628041692,-12.6099268818699));
#39643=CARTESIAN_POINT('Ctrl Pts',(0.849712379879955,-16.7868148719163,
-12.1692615728115));
#39644=CARTESIAN_POINT('Ctrl Pts',(0.890021886410261,-16.792984727058,-12.6733512894767));
#39645=CARTESIAN_POINT('Ctrl Pts',(0.97299032356098,-16.2929963591646,-12.6680018017417));
#39646=CARTESIAN_POINT('Ctrl Pts',(0.522843528836518,-16.7411087801806,
-12.192015621403));
#39647=CARTESIAN_POINT('Ctrl Pts',(0.546774053144795,-16.7425758435111,
-12.6931350453388));
#39648=CARTESIAN_POINT('Ctrl Pts',(0.598698193236015,-16.2427196426588,
-12.6916884026848));
#39649=CARTESIAN_POINT('Ctrl Pts',(0.187614356002326,-16.7285211545107,
-12.1982543436608));
#39650=CARTESIAN_POINT('Ctrl Pts',(0.196065836120502,-16.7288385017964,
-12.6985003258571));
#39651=CARTESIAN_POINT('Ctrl Pts',(0.214833815848565,-16.2288732699618,
-12.6981828003682));
#39652=CARTESIAN_POINT('Ctrl Pts',(-4.99974790012545,-21.7752089154545,
10.8900436331349));
#39653=CARTESIAN_POINT('Ctrl Pts',(-4.9997892831013,-21.7710880447939,11.7026661900649));
#39654=CARTESIAN_POINT('Ctrl Pts',(-5.7251211610453,-21.780229807,11.3363568967879));
#39655=CARTESIAN_POINT('Ctrl Pts',(-5.00304595984301,-21.4467918007238,
10.888211476959));
#39656=CARTESIAN_POINT('Ctrl Pts',(-5.00254692109715,-21.4695196042577,
11.7015768786492));
#39657=CARTESIAN_POINT('Ctrl Pts',(-5.72889771294517,-21.4189707623668,
11.3344496511539));
#39658=CARTESIAN_POINT('Ctrl Pts',(-4.97288676993301,-21.1079790011279,
10.9051863195259));
#39659=CARTESIAN_POINT('Ctrl Pts',(-4.97816559108657,-21.1617339230278,
11.7112712509762));
#39660=CARTESIAN_POINT('Ctrl Pts',(-5.69436296373837,-21.046276901468,11.3521201845275));
#39661=CARTESIAN_POINT('Ctrl Pts',(-4.8475766924768,-20.4556230070702,10.9732455674719));
#39662=CARTESIAN_POINT('Ctrl Pts',(-4.87122044600907,-20.5529478534329,
11.7531280385312));
#39663=CARTESIAN_POINT('Ctrl Pts',(-5.55087265674237,-20.3286853075499,
11.4229687470194));
#39664=CARTESIAN_POINT('Ctrl Pts',(-4.75402318349561,-20.1421071640224,
11.0233953157927));
#39665=CARTESIAN_POINT('Ctrl Pts',(-4.79168297279574,-20.2572142470778,
11.7841890508463));
#39666=CARTESIAN_POINT('Ctrl Pts',(-5.44374621873778,-19.9838178803991,
11.4751738113353));
#39667=CARTESIAN_POINT('Ctrl Pts',(-4.50822613582157,-19.5381796443928,
11.1476441824275));
#39668=CARTESIAN_POINT('Ctrl Pts',(-4.57102076787078,-19.6706340339177,
11.8671679629395));
#39669=CARTESIAN_POINT('Ctrl Pts',(-5.16228845264427,-19.3194976088576,
11.604514846648));
#39670=CARTESIAN_POINT('Ctrl Pts',(-4.35399453240018,-19.2456108462244,
11.222580760125));
#39671=CARTESIAN_POINT('Ctrl Pts',(-4.43086369345143,-19.3804837094271,
11.918784057563));
#39672=CARTESIAN_POINT('Ctrl Pts',(-4.98568062344723,-18.9976719311581,
11.6825225934331));
#39673=CARTESIAN_POINT('Ctrl Pts',(-3.99822324535597,-18.7052566591967,
11.3816435002527));
#39674=CARTESIAN_POINT('Ctrl Pts',(-4.09403979594845,-18.8333578011231,
12.0345832241545));
#39675=CARTESIAN_POINT('Ctrl Pts',(-4.57829334009813,-18.403282324805,11.8481043005667));
#39676=CARTESIAN_POINT('Ctrl Pts',(-3.79614074972304,-18.4547671323408,
11.4661525699866));
#39677=CARTESIAN_POINT('Ctrl Pts',(-3.89978361880875,-18.5742120955944,
12.0982534904074));
#39678=CARTESIAN_POINT('Ctrl Pts',(-4.34689231755036,-18.1277438450899,
11.9360768542446));
#39679=CARTESIAN_POINT('Ctrl Pts',(-3.4555666172681,-18.1076340724598,11.5934834098038));
#39680=CARTESIAN_POINT('Ctrl Pts',(-3.56063728772652,-18.208019782401,12.1983493706666));
#39681=CARTESIAN_POINT('Ctrl Pts',(-3.95690701991751,-17.7458974799482,
12.0686261731993));
#39682=CARTESIAN_POINT('Ctrl Pts',(-3.33556657674612,-17.9967092756542,
11.6360572166061));
#39683=CARTESIAN_POINT('Ctrl Pts',(-3.44136644280938,-18.091181004224,12.2319898021103));
#39684=CARTESIAN_POINT('Ctrl Pts',(-3.81949713715775,-17.6238802033987,
12.1129448069321));
#39685=CARTESIAN_POINT('Ctrl Pts',(-3.08765794162476,-17.7889455607588,
11.7185578736022));
#39686=CARTESIAN_POINT('Ctrl Pts',(-3.19301676454295,-17.8715401644258,
12.2979092990021));
#39687=CARTESIAN_POINT('Ctrl Pts',(-3.53562143018988,-17.3953401166556,
12.1988266394323));
#39688=CARTESIAN_POINT('Ctrl Pts',(-2.95917839859145,-17.6914812338737,
11.7587096839202));
#39689=CARTESIAN_POINT('Ctrl Pts',(-3.06344399393121,-17.7677610739344,
12.3304098410213));
#39690=CARTESIAN_POINT('Ctrl Pts',(-3.38850182188745,-17.2881293572017,
12.2406240146649));
#39691=CARTESIAN_POINT('Ctrl Pts',(-2.56004783110733,-17.4180060566589,
11.874403875677));
#39692=CARTESIAN_POINT('Ctrl Pts',(-2.66175717787732,-17.4782425461364,
12.424067645299));
#39693=CARTESIAN_POINT('Ctrl Pts',(-2.93146460681647,-16.9873066624433,
12.3610597733481));
#39694=CARTESIAN_POINT('Ctrl Pts',(-2.27486874631425,-17.2602612803891,
11.9454237793291));
#39695=CARTESIAN_POINT('Ctrl Pts',(-2.36897880880302,-17.3070252858775,
12.4835705284405));
#39696=CARTESIAN_POINT('Ctrl Pts',(-2.60491117878045,-16.8137874091111,
12.4349903271314));
#39697=CARTESIAN_POINT('Ctrl Pts',(-1.66829057301287,-16.9999892898167,
12.0659549491969));
#39698=CARTESIAN_POINT('Ctrl Pts',(-1.74288242177667,-17.0257586318796,
12.5848852122335));
#39699=CARTESIAN_POINT('Ctrl Pts',(-1.91032945162938,-16.5274882181152,
12.5604613001046));
#39700=CARTESIAN_POINT('Ctrl Pts',(-1.35602206747909,-16.901197524674,12.1136733746908));
#39701=CARTESIAN_POINT('Ctrl Pts',(-1.41703878619547,-16.917247264823,12.6259413073311));
#39702=CARTESIAN_POINT('Ctrl Pts',(-1.55275641664969,-16.4188172766958,
12.6101353975839));
#39703=CARTESIAN_POINT('Ctrl Pts',(-0.874041288385835,-16.7992494614212,
12.1633518858597));
#39704=CARTESIAN_POINT('Ctrl Pts',(-0.913364126384539,-16.8060095815626,
12.6685169960183));
#39705=CARTESIAN_POINT('Ctrl Pts',(-1.00084891791217,-16.3066744077861,
12.6618499142987));
#39706=CARTESIAN_POINT('Ctrl Pts',(-0.711103423472234,-16.7730315381214,
12.1762593351104));
#39707=CARTESIAN_POINT('Ctrl Pts',(-0.743134712400736,-16.7773731884659,
12.679611525474));
#39708=CARTESIAN_POINT('Ctrl Pts',(-0.814271707084701,-16.2778346913951,
12.6752863566669));
#39709=CARTESIAN_POINT('Ctrl Pts',(-0.380466742863404,-16.7367232651056,
12.1941787863531));
#39710=CARTESIAN_POINT('Ctrl Pts',(-0.397886608443954,-16.7378146965554,
12.6949839945871));
#39711=CARTESIAN_POINT('Ctrl Pts',(-0.435665606334057,-16.2378955921547,
12.6939402123975));
#39712=CARTESIAN_POINT('Ctrl Pts',(-0.212389997256555,-16.726751349885,
12.1991315303899));
#39713=CARTESIAN_POINT('Ctrl Pts',(-0.22198786823178,-16.7269094835482,
12.6992537577252));
#39714=CARTESIAN_POINT('Ctrl Pts',(-0.243203955872194,-16.2269264852237,
12.6990959375268));
#39715=CARTESIAN_POINT('Ctrl Pts',(0.285977783389921,-16.7221395157718,
12.2014184689124));
#39716=CARTESIAN_POINT('Ctrl Pts',(0.298771981497033,-16.7218825451742,
12.701218322749));
#39717=CARTESIAN_POINT('Ctrl Pts',(0.327468002777916,-16.2218534666486,
12.7014766025767));
#39718=CARTESIAN_POINT('Ctrl Pts',(0.61472139864815,-16.7518908218649,12.1865389231491));
#39719=CARTESIAN_POINT('Ctrl Pts',(0.644365017122131,-16.7547284026901,
12.6882557475219));
#39720=CARTESIAN_POINT('Ctrl Pts',(0.703906388566332,-16.2545799035585,
12.6859872398608));
#39721=CARTESIAN_POINT('Ctrl Pts',(1.10267114335561,-16.8452929725738,12.1408822967383));
#39722=CARTESIAN_POINT('Ctrl Pts',(1.15158356010911,-16.8560859875697,12.6493167720793));
#39723=CARTESIAN_POINT('Ctrl Pts',(1.26264884196562,-16.3573222700776,12.6384594399526));
#39724=CARTESIAN_POINT('Ctrl Pts',(1.26533226414711,-16.8849300158631,12.121617968646));
#39725=CARTESIAN_POINT('Ctrl Pts',(1.32111739439795,-16.8993078832869,12.6328274609239));
#39726=CARTESIAN_POINT('Ctrl Pts',(1.44890915812603,-16.4009230179359,12.6184055908425));
#39727=CARTESIAN_POINT('Ctrl Pts',(1.58235492966266,-16.979107453112,12.0764753436775));
#39728=CARTESIAN_POINT('Ctrl Pts',(1.6504058732465,-17.0015359945446,12.5944605703878));
#39729=CARTESIAN_POINT('Ctrl Pts',(1.81192609576926,-16.5045181979368,12.571412857232));
#39730=CARTESIAN_POINT('Ctrl Pts',(1.73719161826021,-17.0336380495884,12.0505998841791));
#39731=CARTESIAN_POINT('Ctrl Pts',(1.81102761429328,-17.0607993356339,12.5724903400979));
#39732=CARTESIAN_POINT('Ctrl Pts',(1.98922679567035,-16.5645018547241,12.5444769290866));
#39733=CARTESIAN_POINT('Ctrl Pts',(2.03985290921885,-17.1570998503607,11.9930699877706));
#39734=CARTESIAN_POINT('Ctrl Pts',(2.12375845988698,-17.1943173681734,12.5240400570731));
#39735=CARTESIAN_POINT('Ctrl Pts',(2.33579878210691,-16.7003098352198,12.4845892490906));
#39736=CARTESIAN_POINT('Ctrl Pts',(2.18767675415801,-17.2260321119876,11.9614136149928));
#39737=CARTESIAN_POINT('Ctrl Pts',(2.27614008230909,-17.2688969498113,12.4974526711999));
#39738=CARTESIAN_POINT('Ctrl Pts',(2.50506920142481,-16.7761353230868,12.4516354848906));
#39739=CARTESIAN_POINT('Ctrl Pts',(2.4764397755925,-17.3782900170458,11.8930970814406));
#39740=CARTESIAN_POINT('Ctrl Pts',(2.57238648290045,-17.4327114608064,12.4406234530185));
#39741=CARTESIAN_POINT('Ctrl Pts',(2.83572652977311,-16.94361901885,12.3805190925443));
#39742=CARTESIAN_POINT('Ctrl Pts',(2.61807236646183,-17.4621017397464,11.8562300451449));
#39743=CARTESIAN_POINT('Ctrl Pts',(2.71713597356284,-17.522827623315,12.4101082654188));
#39744=CARTESIAN_POINT('Ctrl Pts',(2.99790745559855,-17.035811914121,12.3421411132669));
#39745=CARTESIAN_POINT('Ctrl Pts',(3.02646929124701,-17.7316428155805,11.7410636200549));
#39746=CARTESIAN_POINT('Ctrl Pts',(3.13548340049963,-17.8131259362093,12.3150866370692));
#39747=CARTESIAN_POINT('Ctrl Pts',(3.46555540992292,-17.3323070963386,12.2222547506283));
#39748=CARTESIAN_POINT('Ctrl Pts',(3.2768849260661,-17.9347368076371,11.658393449684));
#39749=CARTESIAN_POINT('Ctrl Pts',(3.38675242237018,-18.0299754494791,12.2483628505514));
#39750=CARTESIAN_POINT('Ctrl Pts',(3.75230183806937,-17.5557104881875,12.136196461057));
#39751=CARTESIAN_POINT('Ctrl Pts',(3.73678197419356,-18.3872566959992,11.4897869691041));
#39752=CARTESIAN_POINT('Ctrl Pts',(3.84184833985507,-18.5039941659567,12.1163869493151));
#39753=CARTESIAN_POINT('Ctrl Pts',(4.27892165345747,-18.0534823658125,11.9606798765339));
#39754=CARTESIAN_POINT('Ctrl Pts',(3.94731113881133,-18.639068823405,11.4032110584955));
#39755=CARTESIAN_POINT('Ctrl Pts',(4.0451517869323,-18.7653492151445,12.0507009440076));
#39756=CARTESIAN_POINT('Ctrl Pts',(4.51999480434176,-18.330475705872,11.8705557752602));
#39757=CARTESIAN_POINT('Ctrl Pts',(4.31140221038992,-19.1723450226265,11.2425461846842));
#39758=CARTESIAN_POINT('Ctrl Pts',(4.39127065776726,-19.307031058039,11.9329509628929));
#39759=CARTESIAN_POINT('Ctrl Pts',(4.93690892421083,-18.9170795247627,11.7033062729678));
#39760=CARTESIAN_POINT('Ctrl Pts',(4.46721666360654,-19.4553892620641,11.1676980332676));
#39761=CARTESIAN_POINT('Ctrl Pts',(4.53369372541373,-19.5890447445447,11.8809138577861));
#39762=CARTESIAN_POINT('Ctrl Pts',(5.11532924657178,-19.2284281878553,11.6253905765652));
#39763=CARTESIAN_POINT('Ctrl Pts',(4.66055289221914,-19.9067491525735,11.0708606665398));
#39764=CARTESIAN_POINT('Ctrl Pts',(4.70663959852945,-20.0253941374096,11.8162652162982));
#39765=CARTESIAN_POINT('Ctrl Pts',(5.33671507340206,-19.7249240680384,11.5245844638735));
#39766=CARTESIAN_POINT('Ctrl Pts',(4.71841700146108,-20.0625785423806,11.0410534672954));
#39767=CARTESIAN_POINT('Ctrl Pts',(4.75782043068565,-20.1754680451165,11.7967713101401));
#39768=CARTESIAN_POINT('Ctrl Pts',(5.40297422211345,-19.8963363966978,11.4935556590183));
#39769=CARTESIAN_POINT('Ctrl Pts',(4.81755437339946,-20.3765661077494,10.989129292382));
#39770=CARTESIAN_POINT('Ctrl Pts',(4.84482745319202,-20.475027517611,11.763343730263));
#39771=CARTESIAN_POINT('Ctrl Pts',(5.51649463909981,-20.2417227184453,11.4395034432688));
#39772=CARTESIAN_POINT('Ctrl Pts',(4.85917039071759,-20.5353092899111,10.9668478951731));
#39773=CARTESIAN_POINT('Ctrl Pts',(4.88061071522663,-20.6245738078917,11.7494242977742));
#39774=CARTESIAN_POINT('Ctrl Pts',(5.56414839021614,-20.4163402188943,11.4163088747902));
#39775=CARTESIAN_POINT('Ctrl Pts',(4.96045166571747,-21.0168172842587,10.9120800914172));
#39776=CARTESIAN_POINT('Ctrl Pts',(4.96782306317245,-21.0775974027918,11.7153595058825));
#39777=CARTESIAN_POINT('Ctrl Pts',(5.6801237512663,-20.9459990127004,11.359296487993));
#39778=CARTESIAN_POINT('Ctrl Pts',(4.99680880416774,-21.3448363866039,10.8916763988236));
#39779=CARTESIAN_POINT('Ctrl Pts',(4.99733458881033,-21.3762759056631,11.7036358385787));
#39780=CARTESIAN_POINT('Ctrl Pts',(5.72175565143888,-21.3068199155008,11.3380565795594));
#39781=CARTESIAN_POINT('Ctrl Pts',(4.99980122230293,-21.6804159506306,10.890014011117));
#39782=CARTESIAN_POINT('Ctrl Pts',(4.99983385337131,-21.6840753054423,11.7026485840482));
#39783=CARTESIAN_POINT('Ctrl Pts',(5.72518221930917,-21.6759575456936,11.3363260607529));
#39784=CARTESIAN_POINT('',(0.,0.,0.));
#39785=CARTESIAN_POINT('Origin',(0.,0.,-100.));
#39786=CARTESIAN_POINT('',(-4.975,0.,-100.));
#39787=CARTESIAN_POINT('',(4.975,-6.09261782575808E-16,-100.));
#39788=CARTESIAN_POINT('Origin',(0.,0.,-100.));
#39789=CARTESIAN_POINT('',(-3.04630891287904E-16,-3.73065245937137E-32,
-104.975));
#39790=CARTESIAN_POINT('Origin',(0.,0.,-100.));
#39791=CARTESIAN_POINT('Origin',(0.,0.,-100.));
#39792=CARTESIAN_POINT('Origin',(0.,0.,100.));
#39793=CARTESIAN_POINT('',(4.975,6.09261782575808E-16,100.));
#39794=CARTESIAN_POINT('',(-4.975,-6.09261782575808E-16,100.));
#39795=CARTESIAN_POINT('Origin',(0.,0.,100.));
#39796=CARTESIAN_POINT('',(-3.04630891287904E-16,-3.73065245937137E-32,
104.975));
#39797=CARTESIAN_POINT('Origin',(0.,0.,100.));
#39798=CARTESIAN_POINT('Origin',(0.,0.,100.));
#39799=CARTESIAN_POINT('Origin',(0.,0.,100.));
#39800=CARTESIAN_POINT('',(4.975,-6.09261782575808E-16,100.));
#39801=CARTESIAN_POINT('',(0.,0.,0.));
#39802=CARTESIAN_POINT('Origin',(0.,0.,-3.52818915102791));
#39803=CARTESIAN_POINT('',(-2.5527,-3.12615588418345E-16,-3.52818915102791));
#39804=CARTESIAN_POINT('Origin',(0.,0.,-3.52818915102791));
#39805=CARTESIAN_POINT('',(-3.175,-3.88825358729285E-16,-3.09245));
#39806=CARTESIAN_POINT('',(-2.5527,-3.12615588418345E-16,-3.52818915102791));
#39807=CARTESIAN_POINT('',(3.175,3.88825358729285E-16,-3.09245));
#39808=CARTESIAN_POINT('Origin',(0.,0.,-3.09245));
#39809=CARTESIAN_POINT('Origin',(0.,0.,-3.09245));
#39810=CARTESIAN_POINT('Origin',(0.,0.,-3.09245));
#39811=CARTESIAN_POINT('',(-2.5527,3.12615588418345E-16,-2.65671084897211));
#39812=CARTESIAN_POINT('',(2.5527,-3.12615588418345E-16,-2.65671084897211));
#39813=CARTESIAN_POINT('Origin',(0.,0.,-2.65671084897211));
#39814=CARTESIAN_POINT('Origin',(0.,0.,-2.65671084897211));
#39815=CARTESIAN_POINT('',(3.175,-3.88825358729285E-16,-3.09245));
#39816=CARTESIAN_POINT('Origin',(0.,0.,-2.50583915102791));
#39817=CARTESIAN_POINT('',(-2.5527,-3.12615588418345E-16,-2.50583915102791));
#39818=CARTESIAN_POINT('Origin',(0.,0.,-2.50583915102791));
#39819=CARTESIAN_POINT('',(-3.175,-3.88825358729285E-16,-2.0701));
#39820=CARTESIAN_POINT('',(-2.5527,-3.12615588418345E-16,-2.50583915102791));
#39821=CARTESIAN_POINT('',(3.175,3.88825358729285E-16,-2.0701));
#39822=CARTESIAN_POINT('Origin',(0.,0.,-2.0701));
#39823=CARTESIAN_POINT('Origin',(0.,0.,-2.0701));
#39824=CARTESIAN_POINT('Origin',(0.,0.,-2.0701));
#39825=CARTESIAN_POINT('',(-2.5527,3.12615588418345E-16,-1.63436084897211));
#39826=CARTESIAN_POINT('',(2.5527,-3.12615588418345E-16,-1.63436084897211));
#39827=CARTESIAN_POINT('Origin',(0.,0.,-1.63436084897211));
#39828=CARTESIAN_POINT('Origin',(0.,0.,-1.63436084897211));
#39829=CARTESIAN_POINT('',(3.175,-3.88825358729285E-16,-2.0701));
#39830=CARTESIAN_POINT('Origin',(0.,0.,-1.48348915102791));
#39831=CARTESIAN_POINT('',(-2.5527,-3.12615588418345E-16,-1.48348915102791));
#39832=CARTESIAN_POINT('Origin',(0.,0.,-1.48348915102791));
#39833=CARTESIAN_POINT('',(-3.175,-3.88825358729285E-16,-1.04775));
#39834=CARTESIAN_POINT('',(-2.5527,-3.12615588418345E-16,-1.48348915102791));
#39835=CARTESIAN_POINT('',(3.175,3.88825358729285E-16,-1.04775));
#39836=CARTESIAN_POINT('Origin',(0.,0.,-1.04775));
#39837=CARTESIAN_POINT('Origin',(0.,0.,-1.04775));
#39838=CARTESIAN_POINT('Origin',(0.,0.,-1.04775));
#39839=CARTESIAN_POINT('',(-2.5527,3.12615588418345E-16,-0.612010848972106));
#39840=CARTESIAN_POINT('',(2.5527,-3.12615588418345E-16,-0.612010848972106));
#39841=CARTESIAN_POINT('Origin',(0.,0.,-0.612010848972106));
#39842=CARTESIAN_POINT('Origin',(0.,0.,-0.612010848972106));
#39843=CARTESIAN_POINT('',(3.175,-3.88825358729285E-16,-1.04775));
#39844=CARTESIAN_POINT('Origin',(0.,0.,-0.461139151027908));
#39845=CARTESIAN_POINT('',(-2.5527,-3.12615588418345E-16,-0.461139151027908));
#39846=CARTESIAN_POINT('Origin',(0.,0.,-0.461139151027908));
#39847=CARTESIAN_POINT('',(-3.175,-3.88825358729285E-16,-0.0253999999999998));
#39848=CARTESIAN_POINT('',(-2.5527,-3.12615588418345E-16,-0.461139151027908));
#39849=CARTESIAN_POINT('',(3.175,3.88825358729285E-16,-0.0254));
#39850=CARTESIAN_POINT('Origin',(0.,0.,-0.0254));
#39851=CARTESIAN_POINT('Origin',(0.,0.,-0.0254));
#39852=CARTESIAN_POINT('Origin',(0.,0.,-0.0254));
#39853=CARTESIAN_POINT('',(-3.15686252031437,3.87714758407204E-16,-0.0126999999999979));
#39854=CARTESIAN_POINT('',(3.15686252031437,-3.86604158085124E-16,-0.0126999999999974));
#39855=CARTESIAN_POINT('Origin',(0.,0.,-0.0126999999999979));
#39856=CARTESIAN_POINT('',(3.175,-3.88825358729285E-16,-0.0254));
#39857=CARTESIAN_POINT('Origin',(0.,0.,-0.0126999999999979));
#39858=CARTESIAN_POINT('Origin',(0.,0.,-25.0375057290932));
#39859=CARTESIAN_POINT('',(-3.175,-3.88825358729285E-16,-4.1402));
#39860=CARTESIAN_POINT('Origin',(0.,0.,-4.1402));
#39861=CARTESIAN_POINT('',(-3.175,-3.88825358729285E-16,-4.1148));
#39862=CARTESIAN_POINT('',(-3.175,-3.88825358729285E-16,-25.0375057290932));
#39863=CARTESIAN_POINT('',(3.175,3.88825358729285E-16,-4.1148));
#39864=CARTESIAN_POINT('Origin',(0.,0.,-4.1148));
#39865=CARTESIAN_POINT('Origin',(0.,0.,-4.1148));
#39866=CARTESIAN_POINT('Origin',(0.,0.,-4.1148));
#39867=CARTESIAN_POINT('',(-2.5527,3.12615588418345E-16,-3.6790608489721));
#39868=CARTESIAN_POINT('',(2.5527,-3.12615588418345E-16,-3.6790608489721));
#39869=CARTESIAN_POINT('Origin',(0.,0.,-3.6790608489721));
#39870=CARTESIAN_POINT('',(3.175,-3.88825358729285E-16,-4.1148));
#39871=CARTESIAN_POINT('Origin',(0.,0.,-3.6790608489721));
#39872=CARTESIAN_POINT('Origin',(0.,0.,-0.479313066130693));
#39873=CARTESIAN_POINT('',(-3.175,-3.88825358729285E-16,3.67761376907083E-15));
#39874=CARTESIAN_POINT('',(-2.49047,-3.04994611387251E-16,-0.479313066130693));
#39875=CARTESIAN_POINT('Origin',(0.,0.,3.46944695195361E-15));
#39876=CARTESIAN_POINT('Origin',(0.,0.,-4.1402));
#39877=CARTESIAN_POINT('',(-2.5527,-3.12615588418345E-16,-4.1402));
#39878=CARTESIAN_POINT('Origin',(0.,0.,-4.1402));
#39879=CARTESIAN_POINT('',(-2.5527,-3.12615588418345E-16,-4.1402));
#39880=CARTESIAN_POINT('Origin',(0.,0.,-4.1402));
#39881=CARTESIAN_POINT('',(-2.5527,-3.12615588418345E-16,-4.1402));
#39882=CARTESIAN_POINT('Origin',(0.,0.,-4.1402));
#39883=CARTESIAN_POINT('',(-2.5527,-3.12615588418345E-16,-4.1402));
#39884=CARTESIAN_POINT('Origin',(1.99537910293273E-15,6.41580486636973,
-4.1402));
#39885=CARTESIAN_POINT('',(-5.55625,3.20790243318489,-3.5052));
#39886=CARTESIAN_POINT('',(-5.55625,3.20790243318485,-0.634999999999985));
#39887=CARTESIAN_POINT('',(-5.55625,3.20790243318485,-4.1402));
#39888=CARTESIAN_POINT('',(-2.77812500000002,4.81185364977728,0.));
#39889=CARTESIAN_POINT('Ctrl Pts',(-5.55625000003183,3.20790243316647,-0.635000000013559));
#39890=CARTESIAN_POINT('Ctrl Pts',(-4.06745729956738,4.06745729954718,-1.60982338570648E-15));
#39891=CARTESIAN_POINT('Ctrl Pts',(-2.77812500000002,4.81185364977728,-1.09237954906549E-15));
#39892=CARTESIAN_POINT('',(2.60208521396521E-15,6.41580486636973,-0.635));
#39893=CARTESIAN_POINT('Ctrl Pts',(-2.77812500000002,4.81185364977728,-1.09237954906549E-15));
#39894=CARTESIAN_POINT('Ctrl Pts',(-1.48879270043265,5.55625000000739,-4.28910830115607E-16));
#39895=CARTESIAN_POINT('Ctrl Pts',(3.18280067889636E-11,6.41580486638811,
-0.635000000013576));
#39896=CARTESIAN_POINT('',(2.60208521396521E-15,6.41580486636973,-3.5052));
#39897=CARTESIAN_POINT('',(1.99537910293273E-15,6.41580486636973,-4.1402));
#39898=CARTESIAN_POINT('',(-2.77812500000002,4.81185364977728,-4.1402));
#39899=CARTESIAN_POINT('Ctrl Pts',(-2.77812500000001,4.81185364977728,-4.1402));
#39900=CARTESIAN_POINT('Ctrl Pts',(-1.48879270043264,5.55625000000739,-4.1402));
#39901=CARTESIAN_POINT('Ctrl Pts',(3.18250646004606E-11,6.4158048663881,
-3.50519999998643));
#39902=CARTESIAN_POINT('Ctrl Pts',(-5.55625000003182,3.20790243316648,-3.50519999998644));
#39903=CARTESIAN_POINT('Ctrl Pts',(-4.06745729956737,4.06745729954718,-4.1402));
#39904=CARTESIAN_POINT('Ctrl Pts',(-2.77812500000001,4.81185364977728,-4.1402));
#39905=CARTESIAN_POINT('Origin',(5.55625,3.20790243318484,-4.1402));
#39906=CARTESIAN_POINT('',(2.77812500000002,4.81185364977728,0.));
#39907=CARTESIAN_POINT('Ctrl Pts',(-3.18247703816102E-11,6.41580486638811,
-0.635000000013577));
#39908=CARTESIAN_POINT('Ctrl Pts',(1.48879270043264,5.55625000000739,-3.83026943495679E-15));
#39909=CARTESIAN_POINT('Ctrl Pts',(2.77812500000001,4.81185364977728,-2.18475909813097E-15));
#39910=CARTESIAN_POINT('',(5.55625,3.20790243318488,-0.635));
#39911=CARTESIAN_POINT('Ctrl Pts',(2.77812500000001,4.81185364977728,-2.18475909813097E-15));
#39912=CARTESIAN_POINT('Ctrl Pts',(4.06745729956737,4.06745729954718,-5.70175753880392E-16));
#39913=CARTESIAN_POINT('Ctrl Pts',(5.55625000003182,3.20790243316648,-0.635000000013555));
#39914=CARTESIAN_POINT('',(5.55625,3.20790243318488,-3.5052));
#39915=CARTESIAN_POINT('',(5.55625,3.20790243318484,-4.1402));
#39916=CARTESIAN_POINT('',(2.77812500000002,4.81185364977728,-4.1402));
#39917=CARTESIAN_POINT('Ctrl Pts',(2.77812500000002,4.81185364977728,-4.1402));
#39918=CARTESIAN_POINT('Ctrl Pts',(4.06745729956737,4.06745729954718,-4.1402));
#39919=CARTESIAN_POINT('Ctrl Pts',(5.55625000003181,3.20790243316648,-3.50519999998645));
#39920=CARTESIAN_POINT('Ctrl Pts',(-3.18250646004606E-11,6.4158048663881,
-3.50519999998643));
#39921=CARTESIAN_POINT('Ctrl Pts',(1.48879270043265,5.55625000000739,-4.1402));
#39922=CARTESIAN_POINT('Ctrl Pts',(2.77812500000002,4.81185364977728,-4.1402));
#39923=CARTESIAN_POINT('Origin',(5.55625,3.20790243318484,-4.1402));
#39924=CARTESIAN_POINT('',(5.55625,-3.20790243318489,-0.635));
#39925=CARTESIAN_POINT('',(5.55625,0.,0.));
#39926=CARTESIAN_POINT('Ctrl Pts',(5.55625,-3.20790243322164,-0.635000000013576));
#39927=CARTESIAN_POINT('Ctrl Pts',(5.55625,-1.48879270046021,-1.77635683940025E-15));
#39928=CARTESIAN_POINT('Ctrl Pts',(5.55625,-1.09237954906549E-15,-1.63856932359823E-15));
#39929=CARTESIAN_POINT('',(5.55625,-3.20790243318489,-3.5052));
#39930=CARTESIAN_POINT('',(5.55625,-3.20790243318489,-4.1402));
#39931=CARTESIAN_POINT('',(5.55625,0.,-4.1402));
#39932=CARTESIAN_POINT('Ctrl Pts',(5.55625,-3.20790243322163,-3.50519999998643));
#39933=CARTESIAN_POINT('Ctrl Pts',(5.55625,-1.4887927004602,-4.1402));
#39934=CARTESIAN_POINT('Ctrl Pts',(5.55625,7.64665684345841E-15,-4.1402));
#39935=CARTESIAN_POINT('Ctrl Pts',(5.55625,7.64665684345841E-15,-4.1402));
#39936=CARTESIAN_POINT('Ctrl Pts',(5.55625,1.48879270046021,-4.1402));
#39937=CARTESIAN_POINT('Ctrl Pts',(5.55625,3.20790243322163,-3.50519999998643));
#39938=CARTESIAN_POINT('Ctrl Pts',(5.55625,-1.09237954906549E-15,-1.63856932359823E-15));
#39939=CARTESIAN_POINT('Ctrl Pts',(5.55625,1.4887927004602,-1.41042199544234E-15));
#39940=CARTESIAN_POINT('Ctrl Pts',(5.55625,3.20790243322162,-0.635000000013571));
#39941=CARTESIAN_POINT('Origin',(7.33180410152027E-16,-6.41580486636977,
-4.1402));
#39942=CARTESIAN_POINT('',(2.77812500000002,-4.81185364977728,0.));
#39943=CARTESIAN_POINT('Ctrl Pts',(5.55625000003183,-3.20790243316651,-0.635000000013574));
#39944=CARTESIAN_POINT('Ctrl Pts',(4.06745729956739,-4.06745729954721,-2.75335310107039E-14));
#39945=CARTESIAN_POINT('Ctrl Pts',(2.77812500000003,-4.81185364977731,-2.78556785011701E-14));
#39946=CARTESIAN_POINT('',(-7.06899816460549E-14,-6.41580486636973,-0.635));
#39947=CARTESIAN_POINT('Ctrl Pts',(2.77812500000003,-4.81185364977731,-2.78556785011701E-14));
#39948=CARTESIAN_POINT('Ctrl Pts',(1.48879270043264,-5.55625000000743,-2.85795084241335E-14));
#39949=CARTESIAN_POINT('Ctrl Pts',(-3.18624303944503E-11,-6.41580486638817,
-0.63500000001362));
#39950=CARTESIAN_POINT('',(-7.06899816460549E-14,-6.41580486636973,-3.5052));
#39951=CARTESIAN_POINT('',(7.33180410152027E-16,-6.41580486636977,-4.1402));
#39952=CARTESIAN_POINT('',(2.77812500000002,-4.81185364977728,-4.1402));
#39953=CARTESIAN_POINT('Ctrl Pts',(2.77812500000004,-4.81185364977731,-4.14019999999997));
#39954=CARTESIAN_POINT('Ctrl Pts',(1.48879270043264,-5.55625000000743,-4.14019999999997));
#39955=CARTESIAN_POINT('Ctrl Pts',(-3.18500732027373E-11,-6.41580486638816,
-3.50519999998639));
#39956=CARTESIAN_POINT('Ctrl Pts',(5.55625000003182,-3.20790243316652,-3.50519999998643));
#39957=CARTESIAN_POINT('Ctrl Pts',(4.06745729956738,-4.06745729954721,-4.14019999999997));
#39958=CARTESIAN_POINT('Ctrl Pts',(2.77812500000004,-4.81185364977731,-4.14019999999997));
#39959=CARTESIAN_POINT('Origin',(-5.55625,-3.20790243318488,-4.1402));
#39960=CARTESIAN_POINT('',(-2.77812500000002,-4.81185364977727,0.));
#39961=CARTESIAN_POINT('Ctrl Pts',(3.17573942648891E-11,-6.41580486638811,
-0.635000000013576));
#39962=CARTESIAN_POINT('Ctrl Pts',(-1.48879270043268,-5.5562500000074,-2.71449529520851E-14));
#39963=CARTESIAN_POINT('Ctrl Pts',(-2.77812500000004,-4.81185364977731,
-2.68998463957378E-14));
#39964=CARTESIAN_POINT('',(-5.55625,-3.20790243318489,-0.635));
#39965=CARTESIAN_POINT('Ctrl Pts',(-2.77812500000004,-4.81185364977731,
-2.68998463957378E-14));
#39966=CARTESIAN_POINT('Ctrl Pts',(-4.06745729956739,-4.06745729954721,
-2.66940704394404E-14));
#39967=CARTESIAN_POINT('Ctrl Pts',(-5.55625000003183,-3.20790243316651,
-0.635000000013575));
#39968=CARTESIAN_POINT('',(-5.55625,-3.20790243318489,-3.5052));
#39969=CARTESIAN_POINT('',(-5.55625,-3.20790243318488,-4.1402));
#39970=CARTESIAN_POINT('',(-2.77812500000002,-4.81185364977727,-4.1402));
#39971=CARTESIAN_POINT('Ctrl Pts',(-2.77812500000003,-4.81185364977731,
-4.14019999999998));
#39972=CARTESIAN_POINT('Ctrl Pts',(-4.06745729956739,-4.06745729954721,
-4.14019999999998));
#39973=CARTESIAN_POINT('Ctrl Pts',(-5.55625000003182,-3.20790243316651,
-3.50519999998643));
#39974=CARTESIAN_POINT('Ctrl Pts',(3.17612191099431E-11,-6.41580486638811,
-3.50519999998642));
#39975=CARTESIAN_POINT('Ctrl Pts',(-1.48879270043268,-5.55625000000741,
-4.14019999999997));
#39976=CARTESIAN_POINT('Ctrl Pts',(-2.77812500000003,-4.81185364977731,
-4.14019999999998));
#39977=CARTESIAN_POINT('Origin',(-5.55625,3.20790243318485,-4.1402));
#39978=CARTESIAN_POINT('',(-5.55625,0.,0.));
#39979=CARTESIAN_POINT('Ctrl Pts',(-5.55625,-3.20790243322164,-0.635000000013575));
#39980=CARTESIAN_POINT('Ctrl Pts',(-5.55625,-1.48879270046021,-1.0547118733939E-15));
#39981=CARTESIAN_POINT('Ctrl Pts',(-5.55625,-3.82332842172921E-15,-2.73094887266373E-16));
#39982=CARTESIAN_POINT('Ctrl Pts',(-5.55625,-3.82332842172921E-15,-2.73094887266373E-16));
#39983=CARTESIAN_POINT('Ctrl Pts',(-5.55625,1.48879270046019,3.24241151997365E-16));
#39984=CARTESIAN_POINT('Ctrl Pts',(-5.55625,3.2079024332216,-0.63500000001356));
#39985=CARTESIAN_POINT('',(-5.55625,0.,-4.1402));
#39986=CARTESIAN_POINT('Ctrl Pts',(-5.55625,2.73094887266372E-15,-4.1402));
#39987=CARTESIAN_POINT('Ctrl Pts',(-5.55625,1.48879270046021,-4.1402));
#39988=CARTESIAN_POINT('Ctrl Pts',(-5.55625,3.20790243322164,-3.50519999998643));
#39989=CARTESIAN_POINT('Ctrl Pts',(-5.55625,-3.20790243322165,-3.50519999998642));
#39990=CARTESIAN_POINT('Ctrl Pts',(-5.55625,-1.48879270046021,-4.1402));
#39991=CARTESIAN_POINT('Ctrl Pts',(-5.55625,2.73094887266372E-15,-4.1402));
#39992=CARTESIAN_POINT('Origin',(-11.1125,-1.43114686768087E-14,0.));
#39993=CARTESIAN_POINT('Origin',(0.,0.,0.));
#39994=CARTESIAN_POINT('Origin',(0.,0.,0.));
#39995=CARTESIAN_POINT('Origin',(0.,0.,0.));
#39996=CARTESIAN_POINT('Origin',(0.,0.,0.));
#39997=CARTESIAN_POINT('Origin',(0.,0.,0.));
#39998=CARTESIAN_POINT('Origin',(0.,0.,0.));
#39999=CARTESIAN_POINT('Origin',(-11.1125,-1.43114686768087E-14,-4.1402));
#40000=CARTESIAN_POINT('Origin',(0.,0.,-4.1402));
#40001=CARTESIAN_POINT('Origin',(0.,0.,-4.1402));
#40002=CARTESIAN_POINT('Origin',(0.,0.,-4.1402));
#40003=CARTESIAN_POINT('Origin',(0.,0.,-4.1402));
#40004=CARTESIAN_POINT('Origin',(0.,0.,-4.1402));
#40005=CARTESIAN_POINT('Origin',(0.,0.,-4.1402));
#40006=CARTESIAN_POINT('Origin',(0.,0.,-4.1402));
#40007=CARTESIAN_POINT('Origin',(0.,0.,-4.1402));
#40008=CARTESIAN_POINT('Origin',(0.,0.,-4.1402));
#40009=CARTESIAN_POINT('Origin',(0.,0.,-4.1402));
#40010=CARTESIAN_POINT('Origin',(0.,0.,-4.1402));
#40011=CARTESIAN_POINT('Origin',(0.,0.,-4.1402));
#40012=CARTESIAN_POINT('Origin',(0.,0.,0.));
#40013=CARTESIAN_POINT('Origin',(0.,0.,0.));
#40014=CARTESIAN_POINT('Origin',(0.,0.,0.));
#40015=CARTESIAN_POINT('Origin',(0.,0.,0.));
#40016=CARTESIAN_POINT('Origin',(0.,0.,0.));
#40017=CARTESIAN_POINT('Origin',(0.,0.,0.));
#40018=CARTESIAN_POINT('',(0.,0.,0.));
#40019=CARTESIAN_POINT('Origin',(-1.89735380184963E-16,0.,-22.352));
#40020=CARTESIAN_POINT('',(3.302,-4.04378373078456E-16,-22.352));
#40021=CARTESIAN_POINT('Origin',(-1.89735380184963E-16,0.,-22.352));
#40022=CARTESIAN_POINT('',(3.302,-4.04378373078456E-16,-3.302));
#40023=CARTESIAN_POINT('',(3.302,-4.04378373078456E-16,-22.352));
#40024=CARTESIAN_POINT('Origin',(-2.80290902545968E-17,0.,-3.302));
#40025=CARTESIAN_POINT('Origin',(1.73472347597681E-15,0.,-9.31007692307692));
#40026=CARTESIAN_POINT('',(7.112,8.70968803553597E-16,-3.302));
#40027=CARTESIAN_POINT('Origin',(-2.80290902545968E-17,0.,-3.302));
#40028=CARTESIAN_POINT('Origin',(-3.302,0.,-22.352));
#40029=CARTESIAN_POINT('Origin',(-7.112,0.,-3.302));
#40030=CARTESIAN_POINT('',(0.,0.,0.));
#40031=CARTESIAN_POINT('Origin',(42.2402,0.,0.));
#40032=CARTESIAN_POINT('',(41.4932323672501,-3.87762075403097E-16,-3.16631763274988));
#40033=CARTESIAN_POINT('',(41.4932323672501,-3.16631763274987,-3.87762075403096E-16));
#40034=CARTESIAN_POINT('Origin',(41.4932323672501,0.,0.));
#40035=CARTESIAN_POINT('Origin',(41.4932323672501,0.,0.));
#40036=CARTESIAN_POINT('',(42.2402,-2.96284923351715E-16,-2.41935));
#40037=CARTESIAN_POINT('',(42.2402,-2.96284923351715E-16,-2.41935));
#40038=CARTESIAN_POINT('Origin',(42.2402,0.,0.));
#40039=CARTESIAN_POINT('Origin',(40.9702,3.22869914397977E-15,0.));
#40040=CARTESIAN_POINT('',(40.4410881737518,-3.88825358729285E-16,-3.175));
#40041=CARTESIAN_POINT('',(40.4410881737518,3.175,-3.88825358729285E-16));
#40042=CARTESIAN_POINT('Origin',(40.4410881737518,3.16390377354917E-15,
0.));
#40043=CARTESIAN_POINT('Origin',(40.4410881737518,3.16390377354917E-15,
0.));
#40044=CARTESIAN_POINT('',(40.9702,2.41935000000001,-2.96284923351715E-16));
#40045=CARTESIAN_POINT('',(40.9702,2.41935000000001,-2.96284923351715E-16));
#40046=CARTESIAN_POINT('',(40.9702,-2.41935,3.42023499377406E-16));
#40047=CARTESIAN_POINT('Origin',(40.9702,3.22869914397977E-15,0.));
#40048=CARTESIAN_POINT('Origin',(40.9702,3.22869914397977E-15,0.));
#40049=CARTESIAN_POINT('Origin',(41.4993118262482,3.29349451441038E-15,
0.));
#40050=CARTESIAN_POINT('',(41.4993118262482,-3.175,-3.88825358729285E-16));
#40051=CARTESIAN_POINT('Origin',(0.,0.,0.));
#40052=CARTESIAN_POINT('',(40.2293118262482,-3.175,-3.88825358729285E-16));
#40053=CARTESIAN_POINT('',(40.2293118262482,-3.88825358729285E-16,-3.175));
#40054=CARTESIAN_POINT('Origin',(40.2293118262482,3.29349451441038E-15,
0.));
#40055=CARTESIAN_POINT('Origin',(40.2293118262482,3.29349451441038E-15,
0.));
#40056=CARTESIAN_POINT('',(0.,-3.88825358729285E-16,-3.175));
#40057=CARTESIAN_POINT('Origin',(39.7002,3.22869914397977E-15,0.));
#40058=CARTESIAN_POINT('',(39.1710881737518,-3.88825358729285E-16,-3.175));
#40059=CARTESIAN_POINT('',(39.1710881737518,3.17500000000001,-3.88825358729285E-16));
#40060=CARTESIAN_POINT('Origin',(39.1710881737518,3.16390377354917E-15,
0.));
#40061=CARTESIAN_POINT('Origin',(39.1710881737518,3.16390377354917E-15,
0.));
#40062=CARTESIAN_POINT('',(39.7002,2.41935000000001,-2.96284923351715E-16));
#40063=CARTESIAN_POINT('',(39.7002,2.41935000000001,-2.96284923351715E-16));
#40064=CARTESIAN_POINT('',(39.7002,-2.41935,3.425551410405E-16));
#40065=CARTESIAN_POINT('Origin',(39.7002,3.22869914397977E-15,0.));
#40066=CARTESIAN_POINT('Origin',(39.7002,3.22869914397977E-15,0.));
#40067=CARTESIAN_POINT('Origin',(40.2293118262482,3.29349451441038E-15,
0.));
#40068=CARTESIAN_POINT('',(40.2293118262482,-3.175,-3.88825358729285E-16));
#40069=CARTESIAN_POINT('Origin',(0.,0.,0.));
#40070=CARTESIAN_POINT('',(38.9593118262482,-3.175,-3.88825358729285E-16));
#40071=CARTESIAN_POINT('',(38.9593118262482,-3.88825358729285E-16,-3.175));
#40072=CARTESIAN_POINT('Origin',(38.9593118262482,3.29349451441038E-15,
0.));
#40073=CARTESIAN_POINT('Origin',(38.9593118262482,3.29349451441038E-15,
0.));
#40074=CARTESIAN_POINT('',(0.,-3.88825358729285E-16,-3.175));
#40075=CARTESIAN_POINT('Origin',(38.4302,3.22869914397977E-15,0.));
#40076=CARTESIAN_POINT('',(37.9010881737518,-3.88825358729285E-16,-3.175));
#40077=CARTESIAN_POINT('',(37.9010881737518,3.17500000000001,-3.88825358729285E-16));
#40078=CARTESIAN_POINT('Origin',(37.9010881737518,3.16390377354917E-15,
0.));
#40079=CARTESIAN_POINT('Origin',(37.9010881737518,3.16390377354917E-15,
0.));
#40080=CARTESIAN_POINT('',(38.4302,2.41935000000001,-2.96284923351715E-16));
#40081=CARTESIAN_POINT('',(38.4302,2.41935000000001,-2.96284923351715E-16));
#40082=CARTESIAN_POINT('',(38.4302,-2.41935,3.425551410405E-16));
#40083=CARTESIAN_POINT('Origin',(38.4302,3.22869914397977E-15,0.));
#40084=CARTESIAN_POINT('Origin',(38.4302,3.22869914397977E-15,0.));
#40085=CARTESIAN_POINT('Origin',(38.9593118262482,3.29349451441038E-15,
0.));
#40086=CARTESIAN_POINT('',(38.9593118262482,-3.175,-3.88825358729285E-16));
#40087=CARTESIAN_POINT('Origin',(0.,0.,0.));
#40088=CARTESIAN_POINT('',(37.6893118262482,-3.175,-3.88825358729285E-16));
#40089=CARTESIAN_POINT('',(37.6893118262482,-3.88825358729285E-16,-3.175));
#40090=CARTESIAN_POINT('Origin',(37.6893118262482,3.29349451441038E-15,
0.));
#40091=CARTESIAN_POINT('Origin',(37.6893118262482,3.29349451441038E-15,
0.));
#40092=CARTESIAN_POINT('',(0.,-3.88825358729285E-16,-3.175));
#40093=CARTESIAN_POINT('Origin',(37.1602,3.22869914397977E-15,0.));
#40094=CARTESIAN_POINT('',(36.6310881737518,-3.88825358729285E-16,-3.175));
#40095=CARTESIAN_POINT('',(36.6310881737518,3.175,-3.88825358729285E-16));
#40096=CARTESIAN_POINT('Origin',(36.6310881737518,3.16390377354917E-15,
0.));
#40097=CARTESIAN_POINT('Origin',(36.6310881737518,3.16390377354917E-15,
0.));
#40098=CARTESIAN_POINT('',(37.1602,2.41935000000001,-2.96284923351715E-16));
#40099=CARTESIAN_POINT('',(37.1602,2.41935000000001,-2.96284923351715E-16));
#40100=CARTESIAN_POINT('',(37.1602,-2.41935,3.425551410405E-16));
#40101=CARTESIAN_POINT('Origin',(37.1602,3.22869914397977E-15,0.));
#40102=CARTESIAN_POINT('Origin',(37.1602,3.22869914397977E-15,0.));
#40103=CARTESIAN_POINT('Origin',(37.6893118262482,3.29349451441038E-15,
0.));
#40104=CARTESIAN_POINT('',(37.6893118262482,-3.175,-3.88825358729285E-16));
#40105=CARTESIAN_POINT('Origin',(0.,0.,0.));
#40106=CARTESIAN_POINT('',(36.4193118262482,-3.175,-3.88825358729285E-16));
#40107=CARTESIAN_POINT('',(36.4193118262482,-3.88825358729285E-16,-3.175));
#40108=CARTESIAN_POINT('Origin',(36.4193118262482,3.29349451441038E-15,
0.));
#40109=CARTESIAN_POINT('Origin',(36.4193118262482,3.29349451441038E-15,
0.));
#40110=CARTESIAN_POINT('',(0.,-3.88825358729285E-16,-3.175));
#40111=CARTESIAN_POINT('Origin',(35.8902,3.22869914397977E-15,0.));
#40112=CARTESIAN_POINT('',(35.3610881737518,-3.88825358729285E-16,-3.175));
#40113=CARTESIAN_POINT('',(35.3610881737518,3.17500000000001,-3.88825358729285E-16));
#40114=CARTESIAN_POINT('Origin',(35.3610881737518,3.16390377354917E-15,
0.));
#40115=CARTESIAN_POINT('Origin',(35.3610881737518,3.16390377354917E-15,
0.));
#40116=CARTESIAN_POINT('',(35.8902,2.41935000000001,-2.96284923351715E-16));
#40117=CARTESIAN_POINT('',(35.8902,2.41935000000001,-2.96284923351715E-16));
#40118=CARTESIAN_POINT('',(35.8902,-2.41935,3.425551410405E-16));
#40119=CARTESIAN_POINT('Origin',(35.8902,3.22869914397977E-15,0.));
#40120=CARTESIAN_POINT('Origin',(35.8902,3.22869914397977E-15,0.));
#40121=CARTESIAN_POINT('Origin',(36.4193118262482,3.29349451441038E-15,
0.));
#40122=CARTESIAN_POINT('',(36.4193118262482,-3.175,-3.88825358729285E-16));
#40123=CARTESIAN_POINT('Origin',(0.,0.,0.));
#40124=CARTESIAN_POINT('',(35.1493118262482,-3.175,-3.88825358729285E-16));
#40125=CARTESIAN_POINT('',(35.1493118262482,-3.88825358729285E-16,-3.175));
#40126=CARTESIAN_POINT('Origin',(35.1493118262482,3.29349451441038E-15,
0.));
#40127=CARTESIAN_POINT('Origin',(35.1493118262482,3.29349451441038E-15,
0.));
#40128=CARTESIAN_POINT('',(0.,-3.88825358729285E-16,-3.175));
#40129=CARTESIAN_POINT('Origin',(34.6202,3.22869914397977E-15,0.));
#40130=CARTESIAN_POINT('',(34.0910881737518,-3.88825358729285E-16,-3.175));
#40131=CARTESIAN_POINT('',(34.0910881737518,3.17500000000001,-3.88825358729285E-16));
#40132=CARTESIAN_POINT('Origin',(34.0910881737518,3.16390377354917E-15,
0.));
#40133=CARTESIAN_POINT('Origin',(34.0910881737518,3.16390377354917E-15,
0.));
#40134=CARTESIAN_POINT('',(34.6202,2.41935000000001,-2.96284923351715E-16));
#40135=CARTESIAN_POINT('',(34.6202,2.41935000000001,-2.96284923351715E-16));
#40136=CARTESIAN_POINT('',(34.6202,-2.41935,3.425551410405E-16));
#40137=CARTESIAN_POINT('Origin',(34.6202,3.22869914397977E-15,0.));
#40138=CARTESIAN_POINT('Origin',(34.6202,3.22869914397977E-15,0.));
#40139=CARTESIAN_POINT('Origin',(35.1493118262482,3.29349451441038E-15,
0.));
#40140=CARTESIAN_POINT('',(35.1493118262482,-3.175,-3.88825358729285E-16));
#40141=CARTESIAN_POINT('Origin',(0.,0.,0.));
#40142=CARTESIAN_POINT('',(33.8793118262482,-3.175,-3.88825358729285E-16));
#40143=CARTESIAN_POINT('',(33.8793118262482,-3.88825358729285E-16,-3.175));
#40144=CARTESIAN_POINT('Origin',(33.8793118262482,3.29349451441038E-15,
0.));
#40145=CARTESIAN_POINT('Origin',(33.8793118262482,3.29349451441038E-15,
0.));
#40146=CARTESIAN_POINT('',(0.,-3.88825358729285E-16,-3.175));
#40147=CARTESIAN_POINT('Origin',(33.3502,3.22869914397977E-15,0.));
#40148=CARTESIAN_POINT('',(32.8210881737518,-3.88825358729285E-16,-3.175));
#40149=CARTESIAN_POINT('',(32.8210881737518,3.175,-3.88825358729285E-16));
#40150=CARTESIAN_POINT('Origin',(32.8210881737518,3.16390377354917E-15,
0.));
#40151=CARTESIAN_POINT('Origin',(32.8210881737518,3.16390377354917E-15,
0.));
#40152=CARTESIAN_POINT('',(33.3502,2.41935000000001,-2.96284923351715E-16));
#40153=CARTESIAN_POINT('',(33.3502,2.41935000000001,-2.96284923351715E-16));
#40154=CARTESIAN_POINT('',(33.3502,-2.41935,3.425551410405E-16));
#40155=CARTESIAN_POINT('Origin',(33.3502,3.22869914397977E-15,0.));
#40156=CARTESIAN_POINT('Origin',(33.3502,3.22869914397977E-15,0.));
#40157=CARTESIAN_POINT('Origin',(33.8793118262482,3.29349451441038E-15,
0.));
#40158=CARTESIAN_POINT('',(33.8793118262482,-3.175,-3.88825358729285E-16));
#40159=CARTESIAN_POINT('Origin',(0.,0.,0.));
#40160=CARTESIAN_POINT('',(32.6093118262482,-3.175,-3.88825358729285E-16));
#40161=CARTESIAN_POINT('',(32.6093118262482,-3.88825358729285E-16,-3.175));
#40162=CARTESIAN_POINT('Origin',(32.6093118262482,3.29349451441038E-15,
0.));
#40163=CARTESIAN_POINT('Origin',(32.6093118262482,3.29349451441038E-15,
0.));
#40164=CARTESIAN_POINT('',(0.,-3.88825358729285E-16,-3.175));
#40165=CARTESIAN_POINT('Origin',(32.0802,3.22869914397977E-15,0.));
#40166=CARTESIAN_POINT('',(31.5510881737518,-3.88825358729285E-16,-3.175));
#40167=CARTESIAN_POINT('',(31.5510881737518,3.17500000000001,-3.88825358729285E-16));
#40168=CARTESIAN_POINT('Origin',(31.5510881737518,3.16390377354917E-15,
0.));
#40169=CARTESIAN_POINT('Origin',(31.5510881737518,3.16390377354917E-15,
0.));
#40170=CARTESIAN_POINT('',(32.0802,2.41935000000001,-2.96284923351715E-16));
#40171=CARTESIAN_POINT('',(32.0802,2.41935000000001,-2.96284923351715E-16));
#40172=CARTESIAN_POINT('',(32.0802,-2.41935,3.425551410405E-16));
#40173=CARTESIAN_POINT('Origin',(32.0802,3.22869914397977E-15,0.));
#40174=CARTESIAN_POINT('Origin',(32.0802,3.22869914397977E-15,0.));
#40175=CARTESIAN_POINT('Origin',(32.6093118262482,3.29349451441038E-15,
0.));
#40176=CARTESIAN_POINT('',(32.6093118262482,-3.175,-3.88825358729285E-16));
#40177=CARTESIAN_POINT('Origin',(0.,0.,0.));
#40178=CARTESIAN_POINT('',(31.3393118262482,-3.175,-3.88825358729285E-16));
#40179=CARTESIAN_POINT('',(31.3393118262482,-3.88825358729285E-16,-3.175));
#40180=CARTESIAN_POINT('Origin',(31.3393118262482,3.29349451441038E-15,
0.));
#40181=CARTESIAN_POINT('Origin',(31.3393118262482,3.29349451441038E-15,
0.));
#40182=CARTESIAN_POINT('',(0.,-3.88825358729285E-16,-3.175));
#40183=CARTESIAN_POINT('Origin',(30.8102,3.22869914397977E-15,0.));
#40184=CARTESIAN_POINT('',(30.2810881737518,-3.88825358729285E-16,-3.175));
#40185=CARTESIAN_POINT('',(30.2810881737518,3.17500000000001,-3.88825358729285E-16));
#40186=CARTESIAN_POINT('Origin',(30.2810881737518,3.16390377354917E-15,
0.));
#40187=CARTESIAN_POINT('Origin',(30.2810881737518,3.16390377354917E-15,
0.));
#40188=CARTESIAN_POINT('',(30.8102,2.41935000000001,-2.96284923351715E-16));
#40189=CARTESIAN_POINT('',(30.8102,2.41935000000001,-2.96284923351715E-16));
#40190=CARTESIAN_POINT('',(30.8102,-2.41935,3.425551410405E-16));
#40191=CARTESIAN_POINT('Origin',(30.8102,3.22869914397977E-15,0.));
#40192=CARTESIAN_POINT('Origin',(30.8102,3.22869914397977E-15,0.));
#40193=CARTESIAN_POINT('Origin',(31.3393118262482,3.29349451441038E-15,
0.));
#40194=CARTESIAN_POINT('',(31.3393118262482,-3.175,-3.88825358729285E-16));
#40195=CARTESIAN_POINT('Origin',(0.,0.,0.));
#40196=CARTESIAN_POINT('',(30.0693118262482,-3.175,-3.88825358729285E-16));
#40197=CARTESIAN_POINT('',(30.0693118262482,-3.88825358729285E-16,-3.175));
#40198=CARTESIAN_POINT('Origin',(30.0693118262482,3.29349451441038E-15,
0.));
#40199=CARTESIAN_POINT('Origin',(30.0693118262482,3.29349451441038E-15,
0.));
#40200=CARTESIAN_POINT('',(0.,-3.88825358729285E-16,-3.175));
#40201=CARTESIAN_POINT('Origin',(29.5402,3.22869914397977E-15,0.));
#40202=CARTESIAN_POINT('',(29.0110881737518,-3.88825358729285E-16,-3.175));
#40203=CARTESIAN_POINT('',(29.0110881737518,3.17500000000001,-3.88825358729285E-16));
#40204=CARTESIAN_POINT('Origin',(29.0110881737518,3.16390377354917E-15,
0.));
#40205=CARTESIAN_POINT('Origin',(29.0110881737518,3.16390377354917E-15,
0.));
#40206=CARTESIAN_POINT('',(29.5402,2.41935000000001,-2.96284923351715E-16));
#40207=CARTESIAN_POINT('',(29.5402,2.41935000000001,-2.96284923351715E-16));
#40208=CARTESIAN_POINT('',(29.5402,-2.41935,3.425551410405E-16));
#40209=CARTESIAN_POINT('Origin',(29.5402,3.22869914397977E-15,0.));
#40210=CARTESIAN_POINT('Origin',(29.5402,3.22869914397977E-15,0.));
#40211=CARTESIAN_POINT('Origin',(30.0693118262482,3.29349451441038E-15,
0.));
#40212=CARTESIAN_POINT('',(30.0693118262482,-3.175,-3.88825358729285E-16));
#40213=CARTESIAN_POINT('Origin',(0.,0.,0.));
#40214=CARTESIAN_POINT('',(28.7993118262482,-3.175,-3.88825358729285E-16));
#40215=CARTESIAN_POINT('',(28.7993118262482,-3.88825358729285E-16,-3.175));
#40216=CARTESIAN_POINT('Origin',(28.7993118262482,3.29349451441038E-15,
0.));
#40217=CARTESIAN_POINT('Origin',(28.7993118262482,3.29349451441038E-15,
0.));
#40218=CARTESIAN_POINT('',(0.,-3.88825358729285E-16,-3.175));
#40219=CARTESIAN_POINT('Origin',(28.2702,3.22869914397977E-15,0.));
#40220=CARTESIAN_POINT('',(27.7410881737518,-3.88825358729285E-16,-3.175));
#40221=CARTESIAN_POINT('',(27.7410881737518,3.17500000000001,-3.88825358729285E-16));
#40222=CARTESIAN_POINT('Origin',(27.7410881737518,3.16390377354917E-15,
0.));
#40223=CARTESIAN_POINT('Origin',(27.7410881737518,3.16390377354917E-15,
0.));
#40224=CARTESIAN_POINT('',(28.2702,2.41935000000001,-2.96284923351715E-16));
#40225=CARTESIAN_POINT('',(28.2702,2.41935000000001,-2.96284923351715E-16));
#40226=CARTESIAN_POINT('',(28.2702,-2.41935,3.425551410405E-16));
#40227=CARTESIAN_POINT('Origin',(28.2702,3.22869914397977E-15,0.));
#40228=CARTESIAN_POINT('Origin',(28.2702,3.22869914397977E-15,0.));
#40229=CARTESIAN_POINT('Origin',(28.7993118262482,3.29349451441038E-15,
0.));
#40230=CARTESIAN_POINT('',(28.7993118262482,-3.175,-3.88825358729285E-16));
#40231=CARTESIAN_POINT('Origin',(0.,0.,0.));
#40232=CARTESIAN_POINT('',(27.5293118262482,-3.175,-3.88825358729285E-16));
#40233=CARTESIAN_POINT('',(27.5293118262482,-3.88825358729285E-16,-3.175));
#40234=CARTESIAN_POINT('Origin',(27.5293118262482,3.29349451441038E-15,
0.));
#40235=CARTESIAN_POINT('Origin',(27.5293118262482,3.29349451441038E-15,
0.));
#40236=CARTESIAN_POINT('',(0.,-3.88825358729285E-16,-3.175));
#40237=CARTESIAN_POINT('Origin',(27.0002,3.22869914397977E-15,0.));
#40238=CARTESIAN_POINT('',(26.4710881737518,-3.88825358729285E-16,-3.175));
#40239=CARTESIAN_POINT('',(26.4710881737518,3.17500000000001,-3.88825358729285E-16));
#40240=CARTESIAN_POINT('Origin',(26.4710881737518,3.16390377354917E-15,
0.));
#40241=CARTESIAN_POINT('Origin',(26.4710881737518,3.16390377354917E-15,
0.));
#40242=CARTESIAN_POINT('',(27.0002,2.41935000000001,-2.96284923351715E-16));
#40243=CARTESIAN_POINT('',(27.0002,2.41935000000001,-2.96284923351715E-16));
#40244=CARTESIAN_POINT('',(27.0002,-2.41935,3.425551410405E-16));
#40245=CARTESIAN_POINT('Origin',(27.0002,3.22869914397977E-15,0.));
#40246=CARTESIAN_POINT('Origin',(27.0002,3.22869914397977E-15,0.));
#40247=CARTESIAN_POINT('Origin',(27.5293118262482,3.29349451441038E-15,
0.));
#40248=CARTESIAN_POINT('',(27.5293118262482,-3.175,-3.88825358729285E-16));
#40249=CARTESIAN_POINT('Origin',(0.,0.,0.));
#40250=CARTESIAN_POINT('',(26.2593118262482,-3.175,-3.88825358729285E-16));
#40251=CARTESIAN_POINT('',(26.2593118262482,-3.88825358729285E-16,-3.175));
#40252=CARTESIAN_POINT('Origin',(26.2593118262482,3.29349451441038E-15,
0.));
#40253=CARTESIAN_POINT('Origin',(26.2593118262482,3.29349451441038E-15,
0.));
#40254=CARTESIAN_POINT('',(0.,-3.88825358729285E-16,-3.175));
#40255=CARTESIAN_POINT('Origin',(25.7302,3.22869914397977E-15,0.));
#40256=CARTESIAN_POINT('',(25.2010881737518,-3.88825358729285E-16,-3.175));
#40257=CARTESIAN_POINT('',(25.2010881737518,3.17500000000001,-3.88825358729285E-16));
#40258=CARTESIAN_POINT('Origin',(25.2010881737518,3.16390377354917E-15,
0.));
#40259=CARTESIAN_POINT('Origin',(25.2010881737518,3.16390377354917E-15,
0.));
#40260=CARTESIAN_POINT('',(25.7302,2.41935000000001,-2.96284923351715E-16));
#40261=CARTESIAN_POINT('',(25.7302,2.41935000000001,-2.96284923351715E-16));
#40262=CARTESIAN_POINT('',(25.7302,-2.41935,3.425551410405E-16));
#40263=CARTESIAN_POINT('Origin',(25.7302,3.22869914397977E-15,0.));
#40264=CARTESIAN_POINT('Origin',(25.7302,3.22869914397977E-15,0.));
#40265=CARTESIAN_POINT('Origin',(26.2593118262482,3.29349451441038E-15,
0.));
#40266=CARTESIAN_POINT('',(26.2593118262482,-3.175,-3.88825358729285E-16));
#40267=CARTESIAN_POINT('Origin',(0.,0.,0.));
#40268=CARTESIAN_POINT('',(24.9893118262482,-3.175,-3.88825358729285E-16));
#40269=CARTESIAN_POINT('',(24.9893118262482,-3.88825358729285E-16,-3.175));
#40270=CARTESIAN_POINT('Origin',(24.9893118262482,3.29349451441038E-15,
0.));
#40271=CARTESIAN_POINT('Origin',(24.9893118262482,3.29349451441038E-15,
0.));
#40272=CARTESIAN_POINT('',(0.,-3.88825358729285E-16,-3.175));
#40273=CARTESIAN_POINT('Origin',(24.4602,3.22869914397977E-15,0.));
#40274=CARTESIAN_POINT('',(23.9310881737518,-3.88825358729285E-16,-3.175));
#40275=CARTESIAN_POINT('',(23.9310881737518,3.17500000000001,-3.88825358729285E-16));
#40276=CARTESIAN_POINT('Origin',(23.9310881737518,3.16390377354917E-15,
0.));
#40277=CARTESIAN_POINT('Origin',(23.9310881737518,3.16390377354917E-15,
0.));
#40278=CARTESIAN_POINT('',(24.4602,2.41935000000001,-2.96284923351715E-16));
#40279=CARTESIAN_POINT('',(24.4602,2.41935000000001,-2.96284923351715E-16));
#40280=CARTESIAN_POINT('',(24.4602,-2.41935,3.425551410405E-16));
#40281=CARTESIAN_POINT('Origin',(24.4602,3.22869914397977E-15,0.));
#40282=CARTESIAN_POINT('Origin',(24.4602,3.22869914397977E-15,0.));
#40283=CARTESIAN_POINT('Origin',(24.9893118262482,3.29349451441038E-15,
0.));
#40284=CARTESIAN_POINT('',(24.9893118262482,-3.175,-3.88825358729285E-16));
#40285=CARTESIAN_POINT('Origin',(0.,0.,0.));
#40286=CARTESIAN_POINT('',(23.7193118262482,-3.175,-3.88825358729285E-16));
#40287=CARTESIAN_POINT('',(23.7193118262482,-3.88825358729285E-16,-3.175));
#40288=CARTESIAN_POINT('Origin',(23.7193118262482,3.29349451441038E-15,
0.));
#40289=CARTESIAN_POINT('Origin',(23.7193118262482,3.29349451441038E-15,
0.));
#40290=CARTESIAN_POINT('',(0.,-3.88825358729285E-16,-3.175));
#40291=CARTESIAN_POINT('Origin',(23.1902,3.22869914397977E-15,0.));
#40292=CARTESIAN_POINT('',(22.6610881737518,-3.88825358729285E-16,-3.175));
#40293=CARTESIAN_POINT('',(22.6610881737518,3.17500000000001,-3.88825358729285E-16));
#40294=CARTESIAN_POINT('Origin',(22.6610881737518,3.16390377354917E-15,
0.));
#40295=CARTESIAN_POINT('Origin',(22.6610881737518,3.16390377354917E-15,
0.));
#40296=CARTESIAN_POINT('',(23.1902,2.41935000000001,-2.96284923351715E-16));
#40297=CARTESIAN_POINT('',(23.1902,2.41935000000001,-2.96284923351715E-16));
#40298=CARTESIAN_POINT('',(23.1902,-2.41935,3.425551410405E-16));
#40299=CARTESIAN_POINT('Origin',(23.1902,3.22869914397977E-15,0.));
#40300=CARTESIAN_POINT('Origin',(23.1902,3.22869914397977E-15,0.));
#40301=CARTESIAN_POINT('Origin',(23.7193118262482,3.29349451441038E-15,
0.));
#40302=CARTESIAN_POINT('',(23.7193118262482,-3.175,-3.88825358729285E-16));
#40303=CARTESIAN_POINT('Origin',(4.5212,0.,0.));
#40304=CARTESIAN_POINT('',(4.5212,3.88825358729285E-16,-3.175));
#40305=CARTESIAN_POINT('',(4.5212,-3.88825358729285E-16,3.175));
#40306=CARTESIAN_POINT('Origin',(4.5212,0.,0.));
#40307=CARTESIAN_POINT('Origin',(4.5212,0.,0.));
#40308=CARTESIAN_POINT('',(4.1402,-4.35484401776799E-16,3.556));
#40309=CARTESIAN_POINT('Origin',(4.5212,-4.35484401776799E-16,3.556));
#40310=CARTESIAN_POINT('Origin',(4.1402,0.,0.));
#40311=CARTESIAN_POINT('Origin',(0.,0.,0.));
#40312=CARTESIAN_POINT('',(3.7592,-4.81735291109131,2.78130000000001));
#40313=CARTESIAN_POINT('',(3.7592,0.,5.5626));
#40314=CARTESIAN_POINT('Origin',(3.7592,0.,0.));
#40315=CARTESIAN_POINT('',(3.7592,-4.81735291109132,-2.7813));
#40316=CARTESIAN_POINT('Origin',(3.7592,0.,0.));
#40317=CARTESIAN_POINT('',(3.7592,7.5115729936858E-16,-5.5626));
#40318=CARTESIAN_POINT('Origin',(3.7592,0.,0.));
#40319=CARTESIAN_POINT('',(4.1402,-6.81222028493707E-16,-5.5626));
#40320=CARTESIAN_POINT('',(0.,-6.81222028493707E-16,-5.5626));
#40321=CARTESIAN_POINT('Origin',(4.1402,0.,0.));
#40322=CARTESIAN_POINT('',(3.7592,4.81735291109132,-2.78130000000001));
#40323=CARTESIAN_POINT('Origin',(3.7592,0.,0.));
#40324=CARTESIAN_POINT('',(3.7592,4.81735291109131,2.78130000000001));
#40325=CARTESIAN_POINT('Origin',(3.7592,0.,0.));
#40326=CARTESIAN_POINT('Origin',(3.7592,0.,0.));
#40327=CARTESIAN_POINT('Origin',(0.,0.,0.));
#40328=CARTESIAN_POINT('',(0.,-3.88825358729285E-16,-3.175));
#40329=CARTESIAN_POINT('Origin',(4.1402,6.42313721478843,1.3010426069826E-15));
#40330=CARTESIAN_POINT('Origin',(3.7592,5.5626,0.));
#40331=CARTESIAN_POINT('',(3.7592,3.21156860739421,-5.5626));
#40332=CARTESIAN_POINT('',(3.7592,3.21156860739421,-5.5626));
#40333=CARTESIAN_POINT('',(3.7592,3.21156860739421,-5.5626));
#40334=CARTESIAN_POINT('Origin',(3.7592,5.5626,0.));
#40335=CARTESIAN_POINT('',(3.7592,6.42313721478843,0.));
#40336=CARTESIAN_POINT('',(3.7592,3.21156860739421,-5.5626));
#40337=CARTESIAN_POINT('',(3.7592,6.42313721478843,0.));
#40338=CARTESIAN_POINT('Origin',(3.7592,5.5626,0.));
#40339=CARTESIAN_POINT('',(3.7592,3.21156860739421,5.5626));
#40340=CARTESIAN_POINT('',(3.7592,6.42313721478843,0.));
#40341=CARTESIAN_POINT('',(3.7592,3.21156860739421,5.5626));
#40342=CARTESIAN_POINT('Origin',(3.7592,5.5626,0.));
#40343=CARTESIAN_POINT('',(3.7592,-3.21156860739419,5.5626));
#40344=CARTESIAN_POINT('',(3.7592,3.21156860739421,5.5626));
#40345=CARTESIAN_POINT('',(3.7592,-6.42313721478842,0.));
#40346=CARTESIAN_POINT('Origin',(3.7592,5.5626,0.));
#40347=CARTESIAN_POINT('',(3.7592,-6.42313721478842,-8.67361737988404E-16));
#40348=CARTESIAN_POINT('',(3.7592,-6.42313721478842,0.));
#40349=CARTESIAN_POINT('',(3.7592,-3.21156860739422,-5.5626));
#40350=CARTESIAN_POINT('Origin',(3.7592,5.5626,0.));
#40351=CARTESIAN_POINT('',(3.7592,-3.21156860739422,-5.5626));
#40352=CARTESIAN_POINT('',(3.7592,-3.21156860739422,-5.5626));
#40353=CARTESIAN_POINT('',(3.7592,3.21156860739421,-5.5626));
#40354=CARTESIAN_POINT('Origin',(0.,6.42313721478843,1.3010426069826E-15));
#40355=CARTESIAN_POINT('',(0.,7.5115729936858E-16,-5.5626));
#40356=CARTESIAN_POINT('',(0.,4.81735291109131,-2.78130000000001));
#40357=CARTESIAN_POINT('Origin',(0.,0.,0.));
#40358=CARTESIAN_POINT('',(0.,-4.81735291109132,-2.7813));
#40359=CARTESIAN_POINT('Origin',(0.,0.,0.));
#40360=CARTESIAN_POINT('',(0.,-4.81735291109131,2.78130000000001));
#40361=CARTESIAN_POINT('Origin',(0.,0.,0.));
#40362=CARTESIAN_POINT('',(0.,7.51157299368582E-16,5.5626));
#40363=CARTESIAN_POINT('Origin',(0.,0.,0.));
#40364=CARTESIAN_POINT('',(0.,4.81735291109131,2.78130000000001));
#40365=CARTESIAN_POINT('Origin',(0.,0.,0.));
#40366=CARTESIAN_POINT('Origin',(0.,0.,0.));
#40367=CARTESIAN_POINT('Origin',(0.,0.,0.));
#40368=CARTESIAN_POINT('',(0.496831392605788,6.42313721478843,3.39052593516398E-16));
#40369=CARTESIAN_POINT('Ctrl Pts',(0.,4.81735291109132,2.78130000000001));
#40370=CARTESIAN_POINT('Ctrl Pts',(1.11022302462516E-16,5.56260000000048,
1.49049417781655));
#40371=CARTESIAN_POINT('Ctrl Pts',(0.496831392606468,6.42313721478961,-2.03913353027845E-12));
#40372=CARTESIAN_POINT('Ctrl Pts',(0.496831392606465,6.4231372147896,2.03638537188185E-12));
#40373=CARTESIAN_POINT('Ctrl Pts',(-2.59160509497383E-15,5.56260000000047,
-1.49049417781655));
#40374=CARTESIAN_POINT('Ctrl Pts',(-1.14788227546538E-15,4.81735291109131,
-2.78130000000001));
#40375=CARTESIAN_POINT('Origin',(0.,0.,0.));
#40376=CARTESIAN_POINT('',(0.496831392605783,3.21156860739421,5.5626));
#40377=CARTESIAN_POINT('Ctrl Pts',(-2.55084950103419E-16,-3.06101940124103E-15,
5.5626));
#40378=CARTESIAN_POINT('Ctrl Pts',(-8.88178419700125E-16,1.49049417781831,
5.5626));
#40379=CARTESIAN_POINT('Ctrl Pts',(0.496831392606465,3.21156860739657,5.5626));
#40380=CARTESIAN_POINT('Ctrl Pts',(0.496831392606461,3.21156860739304,5.56260000000203));
#40381=CARTESIAN_POINT('Ctrl Pts',(0.,4.07210582218216,4.07210582218346));
#40382=CARTESIAN_POINT('Ctrl Pts',(0.,4.81735291109132,2.78130000000001));
#40383=CARTESIAN_POINT('Origin',(0.,0.,0.));
#40384=CARTESIAN_POINT('',(0.496831392605779,-3.21156860739419,5.5626));
#40385=CARTESIAN_POINT('Ctrl Pts',(0.496831392606463,-3.21156860739656,
5.5626));
#40386=CARTESIAN_POINT('Ctrl Pts',(1.23283174735618E-16,-1.49049417781831,
5.5626));
#40387=CARTESIAN_POINT('Ctrl Pts',(-2.55084950103419E-16,-3.06101940124103E-15,
5.5626));
#40388=CARTESIAN_POINT('Ctrl Pts',(-6.24958127753376E-15,-4.81735291109131,
2.7813));
#40389=CARTESIAN_POINT('Ctrl Pts',(-6.82787160144471E-15,-4.07210582218215,
4.07210582218346));
#40390=CARTESIAN_POINT('Ctrl Pts',(0.496831392606459,-3.21156860739302,
5.56260000000204));
#40391=CARTESIAN_POINT('Origin',(0.,0.,0.));
#40392=CARTESIAN_POINT('',(0.496831392605783,-6.42313721478842,3.05208903104958E-16));
#40393=CARTESIAN_POINT('Ctrl Pts',(0.496831392606464,-6.4231372147896,-2.04160687283539E-12));
#40394=CARTESIAN_POINT('Ctrl Pts',(-5.87150394869329E-15,-5.56260000000047,
1.49049417781655));
#40395=CARTESIAN_POINT('Ctrl Pts',(-6.24958127753376E-15,-4.81735291109131,
2.7813));
#40396=CARTESIAN_POINT('Ctrl Pts',(1.40296722556881E-15,-4.81735291109132,
-2.7813));
#40397=CARTESIAN_POINT('Ctrl Pts',(1.38777878078145E-15,-5.56260000000048,
-1.49049417781654));
#40398=CARTESIAN_POINT('Ctrl Pts',(0.496831392606464,-6.4231372147896,2.03720981940083E-12));
#40399=CARTESIAN_POINT('Origin',(0.,0.,0.));
#40400=CARTESIAN_POINT('',(0.496831392605783,3.21156860739421,-5.5626));
#40401=CARTESIAN_POINT('Ctrl Pts',(-1.14788227546538E-15,4.81735291109131,
-2.78130000000001));
#40402=CARTESIAN_POINT('Ctrl Pts',(4.44089209850063E-16,4.07210582218215,
-4.07210582218347));
#40403=CARTESIAN_POINT('Ctrl Pts',(0.496831392606464,3.21156860739303,-5.56260000000204));
#40404=CARTESIAN_POINT('Ctrl Pts',(0.496831392606462,3.21156860739656,-5.5626));
#40405=CARTESIAN_POINT('Ctrl Pts',(-4.83028869377251E-16,1.49049417781831,
-5.5626));
#40406=CARTESIAN_POINT('Ctrl Pts',(-5.10169900206839E-16,0.,-5.5626));
#40407=CARTESIAN_POINT('Origin',(0.,0.,0.));
#40408=CARTESIAN_POINT('',(0.496831392605573,-3.21156860739453,-5.5626));
#40409=CARTESIAN_POINT('Ctrl Pts',(0.49683139260641,-3.21156860739314,-5.56260000000187));
#40410=CARTESIAN_POINT('Ctrl Pts',(1.46512849432153E-15,-4.07210582218221,
-4.07210582218339));
#40411=CARTESIAN_POINT('Ctrl Pts',(1.40296722556881E-15,-4.81735291109132,
-2.7813));
#40412=CARTESIAN_POINT('Ctrl Pts',(-5.10169900206839E-16,0.,-5.5626));
#40413=CARTESIAN_POINT('Ctrl Pts',(-3.33066907387547E-16,-1.49049417781841,
-5.5626));
#40414=CARTESIAN_POINT('Ctrl Pts',(0.496831392606533,-3.21156860739681,
-5.5626));
#40415=CARTESIAN_POINT('Origin',(4.1402,3.21156860739421,-5.5626));
#40416=CARTESIAN_POINT('',(4.1402,-3.21156860739422,-5.5626));
#40417=CARTESIAN_POINT('',(4.1402,3.21156860739421,-5.5626));
#40418=CARTESIAN_POINT('Origin',(4.1402,-3.21156860739422,-5.5626));
#40419=CARTESIAN_POINT('',(4.1402,-6.42313721478842,0.));
#40420=CARTESIAN_POINT('Origin',(4.1402,-6.42313721478842,0.));
#40421=CARTESIAN_POINT('',(4.1402,-3.21156860739419,5.5626));
#40422=CARTESIAN_POINT('Origin',(4.1402,3.21156860739421,5.5626));
#40423=CARTESIAN_POINT('',(4.1402,3.21156860739421,5.5626));
#40424=CARTESIAN_POINT('Origin',(4.1402,6.42313721478843,0.));
#40425=CARTESIAN_POINT('',(4.1402,6.42313721478843,0.));
#40426=CARTESIAN_POINT('Origin',(4.1402,3.21156860739421,-5.5626));
#40427=CARTESIAN_POINT('Origin',(42.2402,0.,0.));
#40428=CARTESIAN_POINT('',(0.,0.,0.));
#40429=CARTESIAN_POINT('Origin',(-1.64999999999999,1.04982846856907E-14,
-28.575));
#40430=CARTESIAN_POINT('',(-1.64999999999999,1.01094593269614E-14,-25.4));
#40431=CARTESIAN_POINT('Origin',(-1.64999999999999,1.04982846856907E-14,
-28.575));
#40432=CARTESIAN_POINT('',(4.70000000000001,1.01094593269614E-14,-25.4));
#40433=CARTESIAN_POINT('',(-1.64999999999999,1.01094593269614E-14,-25.4));
#40434=CARTESIAN_POINT('Origin',(4.70000000000001,1.04982846856907E-14,
-28.575));
#40435=CARTESIAN_POINT('Origin',(-1.64999999999999,1.04982846856907E-14,
-28.575));
#40436=CARTESIAN_POINT('',(-1.64999999999999,-7.94,-28.575));
#40437=CARTESIAN_POINT('',(-1.64999999999999,7.94000000000002,-28.575));
#40438=CARTESIAN_POINT('Origin',(-1.64999999999999,1.04982846856907E-14,
-28.575));
#40439=CARTESIAN_POINT('',(4.70000000000001,7.94000000000002,-28.575));
#40440=CARTESIAN_POINT('',(-1.64999999999999,7.94000000000002,-28.575));
#40441=CARTESIAN_POINT('',(4.70000000000001,-7.94,-28.575));
#40442=CARTESIAN_POINT('Origin',(4.70000000000001,1.04982846856907E-14,
-28.575));
#40443=CARTESIAN_POINT('',(-1.64999999999999,-7.94,-28.575));
#40444=CARTESIAN_POINT('Origin',(-6.35,0.,28.575));
#40445=CARTESIAN_POINT('',(-6.35,-3.88825358729285E-16,31.75));
#40446=CARTESIAN_POINT('Origin',(-6.35,0.,28.575));
#40447=CARTESIAN_POINT('',(0.,-3.88825358729285E-16,31.75));
#40448=CARTESIAN_POINT('',(-6.35,-3.88825358729285E-16,31.75));
#40449=CARTESIAN_POINT('Origin',(0.,0.,28.575));
#40450=CARTESIAN_POINT('Origin',(-14.7008415550852,0.,26.2892875975978));
#40451=CARTESIAN_POINT('',(0.0986856875723831,-7.94000000000001,0.655754485315154));
#40452=CARTESIAN_POINT('',(3.75057562645881,-7.94,-5.66950443248573));
#40453=CARTESIAN_POINT('',(-14.7008415550852,-7.94000000000001,26.2892875975978));
#40454=CARTESIAN_POINT('',(3.75057562645882,7.94000000000002,-5.66950443248573));
#40455=CARTESIAN_POINT('',(3.75057562645881,0.,-5.66950443248573));
#40456=CARTESIAN_POINT('',(0.0986856875723831,7.94000000000002,0.655754485315154));
#40457=CARTESIAN_POINT('',(-14.7008415550852,7.94000000000001,26.2892875975978));
#40458=CARTESIAN_POINT('',(0.0986856875723831,0.,0.655754485315154));
#40459=CARTESIAN_POINT('Origin',(-20.2001028691164,-7.94000000000001,23.1142875975978));
#40460=CARTESIAN_POINT('',(-5.4005756264588,-7.94000000000001,-2.51924551468485));
#40461=CARTESIAN_POINT('',(-1.74868568757237,-7.94000000000001,-8.84450443248573));
#40462=CARTESIAN_POINT('',(-20.2001028691164,-7.94000000000001,23.1142875975978));
#40463=CARTESIAN_POINT('',(-1.74868568757237,-7.94,-8.84450443248573));
#40464=CARTESIAN_POINT('',(-5.4005756264588,-7.94000000000001,-2.51924551468485));
#40465=CARTESIAN_POINT('Origin',(-20.2001028691164,7.94000000000001,23.1142875975978));
#40466=CARTESIAN_POINT('',(-1.74868568757237,7.94000000000002,-8.84450443248573));
#40467=CARTESIAN_POINT('',(-1.74868568757237,7.94000000000002,-8.84450443248573));
#40468=CARTESIAN_POINT('',(-5.4005756264588,7.94000000000002,-2.51924551468485));
#40469=CARTESIAN_POINT('',(-20.2001028691164,7.94000000000001,23.1142875975978));
#40470=CARTESIAN_POINT('',(-5.4005756264588,7.94000000000002,-2.51924551468485));
#40471=CARTESIAN_POINT('Origin',(-20.2001028691164,0.,23.1142875975978));
#40472=CARTESIAN_POINT('',(-1.74868568757237,0.,-8.84450443248573));
#40473=CARTESIAN_POINT('',(-5.4005756264588,0.,-2.51924551468485));
#40474=CARTESIAN_POINT('Origin',(-6.35,0.,28.575));
#40475=CARTESIAN_POINT('',(0.,7.94000000000001,28.575));
#40476=CARTESIAN_POINT('',(0.,-7.94000000000001,28.575));
#40477=CARTESIAN_POINT('Origin',(0.,0.,28.575));
#40478=CARTESIAN_POINT('',(-6.35,7.94000000000001,28.575));
#40479=CARTESIAN_POINT('',(-6.35,7.94000000000001,28.575));
#40480=CARTESIAN_POINT('',(-6.35,-7.94000000000001,28.575));
#40481=CARTESIAN_POINT('Origin',(-6.35,0.,28.575));
#40482=CARTESIAN_POINT('',(-6.35,-7.94000000000001,28.575));
#40483=CARTESIAN_POINT('Origin',(-6.35,0.,28.575));
#40484=CARTESIAN_POINT('',(-6.35,-7.94000000000001,1.02405448531516));
#40485=CARTESIAN_POINT('',(-6.35,7.94000000000002,1.02405448531516));
#40486=CARTESIAN_POINT('',(-6.35,0.,1.02405448531516));
#40487=CARTESIAN_POINT('',(-6.35,-7.94000000000001,28.575));
#40488=CARTESIAN_POINT('',(-6.35,7.94000000000001,28.575));
#40489=CARTESIAN_POINT('Origin',(-6.35,-7.94000000000001,28.575));
#40490=CARTESIAN_POINT('',(0.,-7.94000000000001,1.02405448531516));
#40491=CARTESIAN_POINT('',(-6.35,-7.94000000000001,1.02405448531516));
#40492=CARTESIAN_POINT('',(0.,-7.94000000000001,28.575));
#40493=CARTESIAN_POINT('Origin',(0.,0.,28.575));
#40494=CARTESIAN_POINT('',(0.,7.94000000000002,1.02405448531516));
#40495=CARTESIAN_POINT('',(0.,0.,1.02405448531516));
#40496=CARTESIAN_POINT('',(0.,7.94000000000001,28.575));
#40497=CARTESIAN_POINT('Origin',(-6.35,7.94000000000001,28.575));
#40498=CARTESIAN_POINT('',(-6.35,7.94000000000002,1.02405448531516));
#40499=CARTESIAN_POINT('Origin',(0.7366,-7.94000000000001,1.02405448531516));
#40500=CARTESIAN_POINT('Origin',(0.7366,-7.94000000000001,1.02405448531516));
#40501=CARTESIAN_POINT('Origin',(0.7366,-7.94000000000001,1.02405448531516));
#40502=CARTESIAN_POINT('Origin',(0.7366,7.94000000000002,1.02405448531516));
#40503=CARTESIAN_POINT('Origin',(0.7366,7.94000000000002,1.02405448531516));
#40504=CARTESIAN_POINT('Origin',(0.7366,7.94000000000002,1.02405448531516));
#40505=CARTESIAN_POINT('Origin',(0.7366,17.2247394858551,1.02405448531516));
#40506=CARTESIAN_POINT('Origin',(0.7366,17.2247394858551,1.02405448531516));
#40507=CARTESIAN_POINT('Origin',(-2.38659999999999,-7.94000000000001,-9.21280443248573));
#40508=CARTESIAN_POINT('',(-1.64999999999998,-7.94,-9.21280443248573));
#40509=CARTESIAN_POINT('',(4.70000000000002,-7.94,-9.21280443248573));
#40510=CARTESIAN_POINT('',(-1.64999999999999,-7.94,-9.21280443248573));
#40511=CARTESIAN_POINT('Origin',(-2.38659999999999,-7.94000000000001,-9.21280443248573));
#40512=CARTESIAN_POINT('Origin',(-2.38659999999999,-7.94000000000001,-9.21280443248573));
#40513=CARTESIAN_POINT('Origin',(-2.38659999999999,7.94000000000002,-9.21280443248573));
#40514=CARTESIAN_POINT('',(4.70000000000002,7.94000000000002,-9.21280443248573));
#40515=CARTESIAN_POINT('Origin',(-2.38659999999999,7.94000000000002,-9.21280443248573));
#40516=CARTESIAN_POINT('',(-1.64999999999999,7.94000000000002,-9.21280443248573));
#40517=CARTESIAN_POINT('',(-1.64999999999999,7.94000000000002,-9.21280443248573));
#40518=CARTESIAN_POINT('Origin',(-2.38659999999999,7.94000000000002,-9.21280443248573));
#40519=CARTESIAN_POINT('Origin',(-2.38659999999999,17.8666679381969,-9.21280443248573));
#40520=CARTESIAN_POINT('',(-1.64999999999998,0.,-9.21280443248573));
#40521=CARTESIAN_POINT('Origin',(-2.38659999999999,17.8666679381969,-9.21280443248573));
#40522=CARTESIAN_POINT('',(4.70000000000002,0.,-9.21280443248573));
#40523=CARTESIAN_POINT('Origin',(-1.64999999999999,0.,29.7381389012326));
#40524=CARTESIAN_POINT('',(-1.64999999999998,-7.94000000000001,29.7381389012326));
#40525=CARTESIAN_POINT('',(-1.64999999999998,7.94000000000001,29.7381389012326));
#40526=CARTESIAN_POINT('Origin',(-1.64999999999998,7.94000000000001,29.7381389012326));
#40527=CARTESIAN_POINT('',(4.70000000000002,7.94000000000001,29.7381389012326));
#40528=CARTESIAN_POINT('Origin',(4.70000000000002,0.,29.7381389012326));
#40529=CARTESIAN_POINT('',(4.70000000000002,-7.94000000000001,29.7381389012326));
#40530=CARTESIAN_POINT('Origin',(-1.64999999999998,-7.94000000000001,29.7381389012326));
#40531=CARTESIAN_POINT('',(0.,0.,0.));
#40532=CARTESIAN_POINT('Origin',(152.4,23.371783782548,7.5));
#40533=CARTESIAN_POINT('',(168.776131634213,23.7277510548322,8.));
#40534=CARTESIAN_POINT('',(152.4,6.99178378254796,8.));
#40535=CARTESIAN_POINT('Origin',(152.4,23.371783782548,8.));
#40536=CARTESIAN_POINT('',(168.27794537285,23.6272260202514,7.5));
#40537=CARTESIAN_POINT('Ctrl Pts',(168.776131634213,23.7277510548321,8.));
#40538=CARTESIAN_POINT('Ctrl Pts',(168.775078472326,23.727537009893,8.));
#40539=CARTESIAN_POINT('Ctrl Pts',(168.774025310872,23.7273229746447,7.99999664467033));
#40540=CARTESIAN_POINT('Ctrl Pts',(168.707149864385,23.7137324075318,7.99957051796987));
#40541=CARTESIAN_POINT('Ctrl Pts',(168.641973161379,23.7005259564475,7.98604806346216));
#40542=CARTESIAN_POINT('Ctrl Pts',(168.521018609496,23.6760802664691,7.93442027877329));
#40543=CARTESIAN_POINT('Ctrl Pts',(168.466249273604,23.6650436658758,7.89698073370765));
#40544=CARTESIAN_POINT('Ctrl Pts',(168.374932604161,23.6466749169578,7.80338879792307));
#40545=CARTESIAN_POINT('Ctrl Pts',(168.338969416124,23.6394586601229,7.74845769049294));
#40546=CARTESIAN_POINT('Ctrl Pts',(168.290420014211,23.629723437839,7.6284017905508));
#40547=CARTESIAN_POINT('Ctrl Pts',(168.277978201841,23.6272325959581,7.56467314065448));
#40548=CARTESIAN_POINT('Ctrl Pts',(168.277945394473,23.6272260245827,7.50017006215143));
#40549=CARTESIAN_POINT('Ctrl Pts',(168.27794537285,23.6272260202515,7.5000850304854));
#40550=CARTESIAN_POINT('Ctrl Pts',(168.27794537285,23.6272260202515,7.5));
#40551=CARTESIAN_POINT('',(152.4,7.49178378254796,7.5));
#40552=CARTESIAN_POINT('Origin',(152.4,23.371783782548,7.5));
#40553=CARTESIAN_POINT('Origin',(152.4,6.99178378254796,7.5));
#40554=CARTESIAN_POINT('Origin',(152.4,23.371783782548,7.5));
#40555=CARTESIAN_POINT('',(181.411385485872,36.2960675998495,7.5));
#40556=CARTESIAN_POINT('',(152.4,-8.38821621745206,7.5));
#40557=CARTESIAN_POINT('Origin',(152.4,23.371783782548,7.5));
#40558=CARTESIAN_POINT('',(180.954657124948,36.0925996556225,8.));
#40559=CARTESIAN_POINT('Origin',(180.954657124948,36.0925996556225,7.5));
#40560=CARTESIAN_POINT('',(152.4,-7.88821621745207,8.));
#40561=CARTESIAN_POINT('Origin',(152.4,23.371783782548,8.));
#40562=CARTESIAN_POINT('Origin',(152.4,-7.88821621745206,7.5));
#40563=CARTESIAN_POINT('Origin',(152.4,23.371783782548,-7.5));
#40564=CARTESIAN_POINT('',(168.27794537285,23.6272260202514,-7.5));
#40565=CARTESIAN_POINT('',(152.4,7.49178378254796,-7.5));
#40566=CARTESIAN_POINT('Origin',(152.4,23.371783782548,-7.5));
#40567=CARTESIAN_POINT('',(168.776131634213,23.7277510548321,-8.));
#40568=CARTESIAN_POINT('Ctrl Pts',(168.27794537285,23.6272260202514,-7.5));
#40569=CARTESIAN_POINT('Ctrl Pts',(168.27794537285,23.6272260202514,-7.50008503046509));
#40570=CARTESIAN_POINT('Ctrl Pts',(168.277945394473,23.6272260245825,-7.5001700621108));
#40571=CARTESIAN_POINT('Ctrl Pts',(168.277978201833,23.6272325959564,-7.56467314059333));
#40572=CARTESIAN_POINT('Ctrl Pts',(168.290420014195,23.6297234378358,-7.62840179049102));
#40573=CARTESIAN_POINT('Ctrl Pts',(168.338969416094,23.6394586601167,-7.74845769043869));
#40574=CARTESIAN_POINT('Ctrl Pts',(168.374932604124,23.6466749169502,-7.80338879787307));
#40575=CARTESIAN_POINT('Ctrl Pts',(168.466249273555,23.6650436658658,-7.89698073366876));
#40576=CARTESIAN_POINT('Ctrl Pts',(168.521018609442,23.6760802664581,-7.93442027874115));
#40577=CARTESIAN_POINT('Ctrl Pts',(168.641973161336,23.7005259564387,-7.98604806345277));
#40578=CARTESIAN_POINT('Ctrl Pts',(168.70714986435,23.7137324075447,-7.99957051796967));
#40579=CARTESIAN_POINT('Ctrl Pts',(168.774025310873,23.7273229746435,-7.99999664467033));
#40580=CARTESIAN_POINT('Ctrl Pts',(168.775078472325,23.7275370098928,-8.));
#40581=CARTESIAN_POINT('Ctrl Pts',(168.776131634213,23.727751054832,-8.));
#40582=CARTESIAN_POINT('',(152.4,6.99178378254796,-8.));
#40583=CARTESIAN_POINT('Origin',(152.4,23.371783782548,-8.));
#40584=CARTESIAN_POINT('Origin',(152.4,6.99178378254796,-7.5));
#40585=CARTESIAN_POINT('Origin',(152.4,23.371783782548,-7.5));
#40586=CARTESIAN_POINT('',(180.954657124948,36.0925996556225,-8.));
#40587=CARTESIAN_POINT('',(152.4,-7.88821621745207,-8.));
#40588=CARTESIAN_POINT('Origin',(152.4,23.371783782548,-8.));
#40589=CARTESIAN_POINT('',(181.411385485872,36.2960675998495,-7.5));
#40590=CARTESIAN_POINT('Origin',(180.954657124948,36.0925996556225,-7.5));
#40591=CARTESIAN_POINT('',(152.4,-8.38821621745206,-7.5));
#40592=CARTESIAN_POINT('Origin',(152.4,23.371783782548,-7.5));
#40593=CARTESIAN_POINT('Origin',(152.4,-7.88821621745206,-7.5));
#40594=CARTESIAN_POINT('Origin',(0.,0.,7.49999999999996));
#40595=CARTESIAN_POINT('',(3.5,4.28626379701574E-16,7.49999999999996));
#40596=CARTESIAN_POINT('',(-3.5,-4.28626379701574E-16,7.49999999999996));
#40597=CARTESIAN_POINT('Origin',(0.,0.,7.49999999999996));
#40598=CARTESIAN_POINT('Origin',(0.,0.,7.49999999999996));
#40599=CARTESIAN_POINT('',(-4.00000000000003,-4.89858719658945E-16,8.));
#40600=CARTESIAN_POINT('',(-3.5,-4.28626379701574E-16,7.49999999999996));
#40601=CARTESIAN_POINT('Origin',(0.,0.,8.));
#40602=CARTESIAN_POINT('Origin',(0.,0.,-8.));
#40603=CARTESIAN_POINT('',(3.5,-4.28626379701574E-16,-7.49999999999998));
#40604=CARTESIAN_POINT('Origin',(0.,0.,-7.49999999999998));
#40605=CARTESIAN_POINT('',(3.99999999999998,-4.89858719658938E-16,-8.));
#40606=CARTESIAN_POINT('',(3.99999999999998,-4.89858719658938E-16,-8.));
#40607=CARTESIAN_POINT('Origin',(0.,0.,-8.));
#40608=CARTESIAN_POINT('Origin',(25.4,0.,7.49999999999996));
#40609=CARTESIAN_POINT('',(28.9,4.28626379701574E-16,7.49999999999996));
#40610=CARTESIAN_POINT('',(21.9,-4.28626379701574E-16,7.49999999999996));
#40611=CARTESIAN_POINT('Origin',(25.4,0.,7.49999999999996));
#40612=CARTESIAN_POINT('Origin',(25.4,0.,7.49999999999996));
#40613=CARTESIAN_POINT('',(21.4,-4.89858719658945E-16,8.));
#40614=CARTESIAN_POINT('',(21.9,-4.28626379701574E-16,7.49999999999996));
#40615=CARTESIAN_POINT('Origin',(25.4,0.,8.));
#40616=CARTESIAN_POINT('Origin',(25.4,0.,-8.));
#40617=CARTESIAN_POINT('',(28.9,-4.28626379701574E-16,-7.49999999999998));
#40618=CARTESIAN_POINT('Origin',(25.4,0.,-7.49999999999998));
#40619=CARTESIAN_POINT('',(29.4,-4.89858719658942E-16,-8.));
#40620=CARTESIAN_POINT('',(29.4,-4.89858719658942E-16,-8.));
#40621=CARTESIAN_POINT('Origin',(25.4,0.,-8.));
#40622=CARTESIAN_POINT('Origin',(50.8,0.,7.49999999999996));
#40623=CARTESIAN_POINT('',(54.3,4.28626379701573E-16,7.49999999999996));
#40624=CARTESIAN_POINT('',(47.3,-4.28626379701574E-16,7.49999999999996));
#40625=CARTESIAN_POINT('Origin',(50.8,0.,7.49999999999996));
#40626=CARTESIAN_POINT('Origin',(50.8,0.,7.49999999999996));
#40627=CARTESIAN_POINT('',(46.8,-4.89858719658945E-16,8.));
#40628=CARTESIAN_POINT('',(47.3,-4.28626379701574E-16,7.49999999999996));
#40629=CARTESIAN_POINT('Origin',(50.8,0.,8.));
#40630=CARTESIAN_POINT('Origin',(50.8,0.,-8.));
#40631=CARTESIAN_POINT('',(54.3,-4.28626379701574E-16,-7.49999999999999));
#40632=CARTESIAN_POINT('Origin',(50.8,0.,-7.49999999999998));
#40633=CARTESIAN_POINT('',(54.8,-4.89858719658942E-16,-8.));
#40634=CARTESIAN_POINT('',(54.8,-4.89858719658942E-16,-8.));
#40635=CARTESIAN_POINT('Origin',(50.8,0.,-8.));
#40636=CARTESIAN_POINT('Origin',(76.2,0.,7.49999999999995));
#40637=CARTESIAN_POINT('',(79.7,4.28626379701573E-16,7.49999999999995));
#40638=CARTESIAN_POINT('',(72.7,-4.28626379701572E-16,7.49999999999995));
#40639=CARTESIAN_POINT('Origin',(76.2,0.,7.49999999999995));
#40640=CARTESIAN_POINT('Origin',(76.2,0.,7.49999999999995));
#40641=CARTESIAN_POINT('',(72.2,-4.89858719658946E-16,8.00000000000001));
#40642=CARTESIAN_POINT('',(72.7,-4.28626379701572E-16,7.49999999999995));
#40643=CARTESIAN_POINT('Origin',(76.2,0.,8.));
#40644=CARTESIAN_POINT('Origin',(76.2,0.,-8.));
#40645=CARTESIAN_POINT('',(79.7,-4.28626379701572E-16,-7.49999999999997));
#40646=CARTESIAN_POINT('Origin',(76.2,0.,-7.49999999999998));
#40647=CARTESIAN_POINT('',(80.2,-4.89858719658942E-16,-8.));
#40648=CARTESIAN_POINT('',(80.2,-4.89858719658942E-16,-8.));
#40649=CARTESIAN_POINT('Origin',(76.2,0.,-8.));
#40650=CARTESIAN_POINT('Origin',(101.6,0.,7.49999999999995));
#40651=CARTESIAN_POINT('',(105.1,4.28626379701573E-16,7.49999999999995));
#40652=CARTESIAN_POINT('',(98.1,-4.28626379701572E-16,7.49999999999995));
#40653=CARTESIAN_POINT('Origin',(101.6,0.,7.49999999999995));
#40654=CARTESIAN_POINT('Origin',(101.6,0.,7.49999999999995));
#40655=CARTESIAN_POINT('',(97.6,-4.89858719658945E-16,8.00000000000001));
#40656=CARTESIAN_POINT('',(98.1,-4.28626379701572E-16,7.49999999999995));
#40657=CARTESIAN_POINT('Origin',(101.6,0.,8.));
#40658=CARTESIAN_POINT('Origin',(101.6,0.,-8.));
#40659=CARTESIAN_POINT('',(105.1,-4.28626379701573E-16,-7.50000000000003));
#40660=CARTESIAN_POINT('Origin',(101.6,0.,-7.50000000000003));
#40661=CARTESIAN_POINT('',(105.6,-4.89858719658938E-16,-8.));
#40662=CARTESIAN_POINT('',(105.6,-4.89858719658938E-16,-8.));
#40663=CARTESIAN_POINT('Origin',(101.6,0.,-8.));
#40664=CARTESIAN_POINT('Origin',(101.6,0.,8.));
#40665=CARTESIAN_POINT('',(105.1,-4.28626379701572E-16,8.));
#40666=CARTESIAN_POINT('Origin',(76.2,0.,8.));
#40667=CARTESIAN_POINT('',(79.7,-4.28626379701572E-16,8.));
#40668=CARTESIAN_POINT('Origin',(50.8,0.,8.));
#40669=CARTESIAN_POINT('',(54.3,-4.28626379701574E-16,8.));
#40670=CARTESIAN_POINT('Origin',(25.4,0.,8.));
#40671=CARTESIAN_POINT('',(28.9,-4.28626379701574E-16,8.));
#40672=CARTESIAN_POINT('Origin',(0.,0.,8.));
#40673=CARTESIAN_POINT('',(3.5,-4.28626379701574E-16,8.));
#40674=CARTESIAN_POINT('Origin',(169.138185555828,29.5714781038137,8.));
#40675=CARTESIAN_POINT('',(166.351396773299,28.4607088741485,7.5));
#40676=CARTESIAN_POINT('',(167.638185555828,32.169554315167,7.5));
#40677=CARTESIAN_POINT('Origin',(169.138185555828,29.5714781038137,7.5));
#40678=CARTESIAN_POINT('',(167.638185555828,32.169554315167,-7.5));
#40679=CARTESIAN_POINT('',(167.638185555828,32.169554315167,8.));
#40680=CARTESIAN_POINT('',(166.351396773299,28.4607088741485,-7.5));
#40681=CARTESIAN_POINT('Origin',(169.138185555828,29.5714781038137,-7.5));
#40682=CARTESIAN_POINT('',(166.351396773299,28.4607088741485,8.));
#40683=CARTESIAN_POINT('Origin',(-42.86,-0.448216217452066,8.));
#40684=CARTESIAN_POINT('',(-42.86,-8.38821621745207,7.5));
#40685=CARTESIAN_POINT('',(-42.86,7.49178378254793,7.5));
#40686=CARTESIAN_POINT('Origin',(-42.86,-0.448216217452066,7.5));
#40687=CARTESIAN_POINT('',(-42.86,7.49178378254793,-7.5));
#40688=CARTESIAN_POINT('',(-42.86,7.49178378254793,8.));
#40689=CARTESIAN_POINT('',(-42.86,-8.38821621745207,-7.5));
#40690=CARTESIAN_POINT('Origin',(-42.86,-0.448216217452066,-7.5));
#40691=CARTESIAN_POINT('',(-42.86,-8.38821621745207,8.));
#40692=CARTESIAN_POINT('Origin',(-42.86,-0.448216217452066,8.));
#40693=CARTESIAN_POINT('',(166.815861570388,28.6458370790927,8.));
#40694=CARTESIAN_POINT('',(168.742410169938,23.8123542251956,8.));
#40695=CARTESIAN_POINT('',(-42.86,6.99178378254793,8.));
#40696=CARTESIAN_POINT('',(-42.86,6.99178378254793,8.));
#40697=CARTESIAN_POINT('',(-42.86,-7.88821621745207,8.));
#40698=CARTESIAN_POINT('Origin',(-42.86,-0.448216217452066,8.));
#40699=CARTESIAN_POINT('',(152.4,-7.88821621745207,8.));
#40700=CARTESIAN_POINT('',(177.42101532033,37.2403234439484,8.));
#40701=CARTESIAN_POINT('Origin',(178.67101532033,35.0752599344873,8.));
#40702=CARTESIAN_POINT('',(167.888185555828,31.7365416132748,8.));
#40703=CARTESIAN_POINT('',(167.888185555829,31.7365416132748,8.));
#40704=CARTESIAN_POINT('Origin',(169.138185555828,29.5714781038137,8.));
#40705=CARTESIAN_POINT('Origin',(-42.86,-0.448216217452066,-8.));
#40706=CARTESIAN_POINT('',(-42.86,6.99178378254793,-8.));
#40707=CARTESIAN_POINT('',(-42.86,6.99178378254793,-8.));
#40708=CARTESIAN_POINT('',(166.815861570388,28.6458370790927,-8.));
#40709=CARTESIAN_POINT('',(148.078108595041,75.6566458113737,-8.));
#40710=CARTESIAN_POINT('',(167.888185555828,31.7365416132748,-8.));
#40711=CARTESIAN_POINT('Origin',(169.138185555828,29.5714781038137,-8.));
#40712=CARTESIAN_POINT('',(177.42101532033,37.2403234439484,-8.));
#40713=CARTESIAN_POINT('',(-4.10936255907258,-67.5662890908191,-8.));
#40714=CARTESIAN_POINT('Origin',(178.67101532033,35.0752599344873,-8.));
#40715=CARTESIAN_POINT('',(-42.86,-7.88821621745207,-8.));
#40716=CARTESIAN_POINT('',(-42.86,-7.88821621745207,-8.));
#40717=CARTESIAN_POINT('Origin',(-42.86,-0.448216217452066,-8.));
#40718=CARTESIAN_POINT('Origin',(-42.86,-8.38821621745207,8.));
#40719=CARTESIAN_POINT('',(152.4,-8.38821621745206,8.));
#40720=CARTESIAN_POINT('',(-42.86,-8.38821621745207,7.5));
#40721=CARTESIAN_POINT('',(-42.86,-8.38821621745207,-7.5));
#40722=CARTESIAN_POINT('Origin',(152.4,23.371783782548,8.));
#40723=CARTESIAN_POINT('',(181.411385485872,36.2960675998495,8.));
#40724=CARTESIAN_POINT('Origin',(178.67101532033,35.0752599344873,8.));
#40725=CARTESIAN_POINT('',(177.17101532033,37.6733361458406,-7.5));
#40726=CARTESIAN_POINT('Origin',(178.67101532033,35.0752599344873,-7.5));
#40727=CARTESIAN_POINT('',(177.17101532033,37.6733361458406,7.5));
#40728=CARTESIAN_POINT('',(177.17101532033,37.6733361458406,8.));
#40729=CARTESIAN_POINT('Origin',(178.67101532033,35.0752599344873,7.5));
#40730=CARTESIAN_POINT('Origin',(167.638185555828,32.169554315167,8.));
#40731=CARTESIAN_POINT('',(167.638185555828,32.169554315167,-7.5));
#40732=CARTESIAN_POINT('',(177.17101532033,37.6733361458406,7.5));
#40733=CARTESIAN_POINT('Origin',(168.27794537285,23.6272260202514,8.));
#40734=CARTESIAN_POINT('',(168.27794537285,23.6272260202514,-7.5));
#40735=CARTESIAN_POINT('',(168.27794537285,23.6272260202514,8.));
#40736=CARTESIAN_POINT('',(166.351396773299,28.4607088741485,7.5));
#40737=CARTESIAN_POINT('Origin',(152.4,23.371783782548,8.));
#40738=CARTESIAN_POINT('',(152.4,7.49178378254796,8.));
#40739=CARTESIAN_POINT('Origin',(152.4,7.49178378254796,8.));
#40740=CARTESIAN_POINT('',(152.4,7.49178378254796,-7.5));
#40741=CARTESIAN_POINT('',(152.4,7.49178378254796,7.5));
#40742=CARTESIAN_POINT('Origin',(178.67101532033,35.0752599344873,-7.5));
#40743=CARTESIAN_POINT('Origin',(177.42101532033,37.2403234439484,-7.5));
#40744=CARTESIAN_POINT('Origin',(167.888185555828,31.7365416132748,-7.5));
#40745=CARTESIAN_POINT('Origin',(167.888185555828,31.7365416132748,-7.5));
#40746=CARTESIAN_POINT('Origin',(-42.86,-7.88821621745207,-7.5));
#40747=CARTESIAN_POINT('Origin',(-42.86,-7.88821621745207,-7.5));
#40748=CARTESIAN_POINT('Origin',(169.138185555828,29.5714781038137,-7.5));
#40749=CARTESIAN_POINT('Origin',(166.815861570388,28.6458370790927,-7.5));
#40750=CARTESIAN_POINT('Origin',(-42.86,-0.448216217452066,-7.5));
#40751=CARTESIAN_POINT('Origin',(-42.86,6.99178378254793,-7.5));
#40752=CARTESIAN_POINT('Origin',(168.742410169938,23.8123542251956,-7.5));
#40753=CARTESIAN_POINT('Origin',(152.4,6.99178378254796,-7.5));
#40754=CARTESIAN_POINT('Origin',(178.67101532033,35.0752599344873,7.5));
#40755=CARTESIAN_POINT('Origin',(177.42101532033,37.2403234439484,7.5));
#40756=CARTESIAN_POINT('Origin',(-4.10936255907258,-67.5662890908191,7.5));
#40757=CARTESIAN_POINT('Origin',(167.888185555828,31.7365416132748,7.5));
#40758=CARTESIAN_POINT('Origin',(-42.86,-7.88821621745207,7.5));
#40759=CARTESIAN_POINT('Origin',(-42.86,-7.88821621745207,7.5));
#40760=CARTESIAN_POINT('Origin',(169.138185555828,29.5714781038137,7.5));
#40761=CARTESIAN_POINT('Origin',(166.815861570388,28.6458370790927,7.5));
#40762=CARTESIAN_POINT('Origin',(-42.86,-0.448216217452066,7.5));
#40763=CARTESIAN_POINT('Origin',(-42.86,6.99178378254793,7.5));
#40764=CARTESIAN_POINT('Origin',(148.078108595041,75.6566458113737,7.5));
#40765=CARTESIAN_POINT('Origin',(-42.86,6.99178378254793,7.5));
#40766=CARTESIAN_POINT('',(687.437953078557,884.821799834261,1338.37406559768));
#40767=CARTESIAN_POINT('',(710.524741121748,900.659820659997,1364.10390512225));
#40768=CARTESIAN_POINT('',(679.396519570846,899.236570464519,1272.01068278906));
#40769=CARTESIAN_POINT('',(685.437498628351,1010.67434947621,1269.28079269916));
#40770=CARTESIAN_POINT('',(712.341727135413,891.127172021311,1301.15555342554));
#40771=CARTESIAN_POINT('',(684.261876936784,988.987687592588,1269.81205062519));
#40772=CARTESIAN_POINT('',(690.214897579682,876.787325037233,1366.26300310009));
#40773=CARTESIAN_POINT('',(725.197162668008,874.602124326474,1354.47249796656));
#40774=CARTESIAN_POINT('',(711.465533452033,883.320894001657,1330.27575323782));
#40775=CARTESIAN_POINT('',(670.053185678087,893.768766286753,1315.40858317885));
#40776=CARTESIAN_POINT('',(612.064685470445,887.279792168539,1271.91896352332));
#40777=CARTESIAN_POINT('',(712.130546721313,880.460447156797,1214.98008132799));
#40778=CARTESIAN_POINT('',(637.329772355579,894.835907219438,1286.55700434221));
#40779=CARTESIAN_POINT('',(687.37761148166,890.708823213982,1228.83485358174));
#40780=CARTESIAN_POINT('',(583.771324279274,880.258548927219,1272.41383411343));
#40781=CARTESIAN_POINT('',(725.30393336762,870.589690944876,1190.91585274861));
#40782=CARTESIAN_POINT('',(646.096397225552,893.287493820459,1242.7483713992));
#40783=CARTESIAN_POINT('',(720.899528069002,889.615642347399,1258.39045677141));
#40784=CARTESIAN_POINT('',(591.023321736823,878.977658025757,1236.17410680295));
#40785=CARTESIAN_POINT('',(753.03420099843,869.685381135511,1215.36507492552));
#40786=CARTESIAN_POINT('',(617.045722328335,886.400011828146,1247.0276948057));
#40787=CARTESIAN_POINT('',(731.177090236866,879.839321664351,1231.77303768571));
#40788=CARTESIAN_POINT('',(584.257194616421,904.777522747334,1252.77633557451));
#40789=CARTESIAN_POINT('',(743.54612910195,894.827386814886,1199.08921740127));
#40790=UNCERTAINTY_MEASURE_WITH_UNIT(LENGTH_MEASURE(0.01),#40810,
'DISTANCE_ACCURACY_VALUE',
'Maximum model space distance between geometric entities at asserted c
onnectivities');
#40791=UNCERTAINTY_MEASURE_WITH_UNIT(LENGTH_MEASURE(0.01),#40810,
'DISTANCE_ACCURACY_VALUE',
'Maximum model space distance between geometric entities at asserted c
onnectivities');
#40792=UNCERTAINTY_MEASURE_WITH_UNIT(LENGTH_MEASURE(0.01),#40810,
'DISTANCE_ACCURACY_VALUE',
'Maximum model space distance between geometric entities at asserted c
onnectivities');
#40793=UNCERTAINTY_MEASURE_WITH_UNIT(LENGTH_MEASURE(0.01),#40810,
'DISTANCE_ACCURACY_VALUE',
'Maximum model space distance between geometric entities at asserted c
onnectivities');
#40794=UNCERTAINTY_MEASURE_WITH_UNIT(LENGTH_MEASURE(0.01),#40810,
'DISTANCE_ACCURACY_VALUE',
'Maximum model space distance between geometric entities at asserted c
onnectivities');
#40795=UNCERTAINTY_MEASURE_WITH_UNIT(LENGTH_MEASURE(0.01),#40810,
'DISTANCE_ACCURACY_VALUE',
'Maximum model space distance between geometric entities at asserted c
onnectivities');
#40796=UNCERTAINTY_MEASURE_WITH_UNIT(LENGTH_MEASURE(0.01),#40810,
'DISTANCE_ACCURACY_VALUE',
'Maximum model space distance between geometric entities at asserted c
onnectivities');
#40797=UNCERTAINTY_MEASURE_WITH_UNIT(LENGTH_MEASURE(0.01),#40810,
'DISTANCE_ACCURACY_VALUE',
'Maximum model space distance between geometric entities at asserted c
onnectivities');
#40798=UNCERTAINTY_MEASURE_WITH_UNIT(LENGTH_MEASURE(0.01),#40810,
'DISTANCE_ACCURACY_VALUE',
'Maximum model space distance between geometric entities at asserted c
onnectivities');
#40799=UNCERTAINTY_MEASURE_WITH_UNIT(LENGTH_MEASURE(0.01),#40810,
'DISTANCE_ACCURACY_VALUE',
'Maximum model space distance between geometric entities at asserted c
onnectivities');
#40800=(
GEOMETRIC_REPRESENTATION_CONTEXT(3)
GLOBAL_UNCERTAINTY_ASSIGNED_CONTEXT((#40790))
GLOBAL_UNIT_ASSIGNED_CONTEXT((#40810,#40812,#40813))
REPRESENTATION_CONTEXT('','3D')
);
#40801=(
GEOMETRIC_REPRESENTATION_CONTEXT(3)
GLOBAL_UNCERTAINTY_ASSIGNED_CONTEXT((#40791))
GLOBAL_UNIT_ASSIGNED_CONTEXT((#40810,#40812,#40813))
REPRESENTATION_CONTEXT('','3D')
);
#40802=(
GEOMETRIC_REPRESENTATION_CONTEXT(3)
GLOBAL_UNCERTAINTY_ASSIGNED_CONTEXT((#40792))
GLOBAL_UNIT_ASSIGNED_CONTEXT((#40810,#40812,#40813))
REPRESENTATION_CONTEXT('','3D')
);
#40803=(
GEOMETRIC_REPRESENTATION_CONTEXT(3)
GLOBAL_UNCERTAINTY_ASSIGNED_CONTEXT((#40793))
GLOBAL_UNIT_ASSIGNED_CONTEXT((#40810,#40812,#40813))
REPRESENTATION_CONTEXT('','3D')
);
#40804=(
GEOMETRIC_REPRESENTATION_CONTEXT(3)
GLOBAL_UNCERTAINTY_ASSIGNED_CONTEXT((#40794))
GLOBAL_UNIT_ASSIGNED_CONTEXT((#40810,#40812,#40813))
REPRESENTATION_CONTEXT('','3D')
);
#40805=(
GEOMETRIC_REPRESENTATION_CONTEXT(3)
GLOBAL_UNCERTAINTY_ASSIGNED_CONTEXT((#40795))
GLOBAL_UNIT_ASSIGNED_CONTEXT((#40810,#40812,#40813))
REPRESENTATION_CONTEXT('','3D')
);
#40806=(
GEOMETRIC_REPRESENTATION_CONTEXT(3)
GLOBAL_UNCERTAINTY_ASSIGNED_CONTEXT((#40796))
GLOBAL_UNIT_ASSIGNED_CONTEXT((#40810,#40812,#40813))
REPRESENTATION_CONTEXT('','3D')
);
#40807=(
GEOMETRIC_REPRESENTATION_CONTEXT(3)
GLOBAL_UNCERTAINTY_ASSIGNED_CONTEXT((#40797))
GLOBAL_UNIT_ASSIGNED_CONTEXT((#40810,#40812,#40813))
REPRESENTATION_CONTEXT('','3D')
);
#40808=(
GEOMETRIC_REPRESENTATION_CONTEXT(3)
GLOBAL_UNCERTAINTY_ASSIGNED_CONTEXT((#40798))
GLOBAL_UNIT_ASSIGNED_CONTEXT((#40810,#40812,#40813))
REPRESENTATION_CONTEXT('','3D')
);
#40809=(
GEOMETRIC_REPRESENTATION_CONTEXT(3)
GLOBAL_UNCERTAINTY_ASSIGNED_CONTEXT((#40799))
GLOBAL_UNIT_ASSIGNED_CONTEXT((#40810,#40812,#40813))
REPRESENTATION_CONTEXT('','3D')
);
#40810=(
LENGTH_UNIT()
NAMED_UNIT(*)
SI_UNIT(.MILLI.,.METRE.)
);
#40811=(
LENGTH_UNIT()
NAMED_UNIT(*)
SI_UNIT($,.METRE.)
);
#40812=(
NAMED_UNIT(*)
PLANE_ANGLE_UNIT()
SI_UNIT($,.RADIAN.)
);
#40813=(
NAMED_UNIT(*)
SI_UNIT($,.STERADIAN.)
SOLID_ANGLE_UNIT()
);
#40814=SHAPE_DEFINITION_REPRESENTATION(#40823,#40856);
#40815=SHAPE_DEFINITION_REPRESENTATION(#40824,#40857);
#40816=SHAPE_DEFINITION_REPRESENTATION(#40825,#40858);
#40817=SHAPE_DEFINITION_REPRESENTATION(#40826,#40859);
#40818=SHAPE_DEFINITION_REPRESENTATION(#40827,#40860);
#40819=SHAPE_DEFINITION_REPRESENTATION(#40828,#40861);
#40820=SHAPE_DEFINITION_REPRESENTATION(#40829,#40862);
#40821=SHAPE_DEFINITION_REPRESENTATION(#40830,#40863);
#40822=SHAPE_DEFINITION_REPRESENTATION(#40831,#40864);
#40823=PRODUCT_DEFINITION_SHAPE('',$,#40866);
#40824=PRODUCT_DEFINITION_SHAPE('',$,#40867);
#40825=PRODUCT_DEFINITION_SHAPE('',$,#40868);
#40826=PRODUCT_DEFINITION_SHAPE('',$,#40869);
#40827=PRODUCT_DEFINITION_SHAPE('',$,#40870);
#40828=PRODUCT_DEFINITION_SHAPE('',$,#40871);
#40829=PRODUCT_DEFINITION_SHAPE('',$,#40872);
#40830=PRODUCT_DEFINITION_SHAPE('',$,#40873);
#40831=PRODUCT_DEFINITION_SHAPE('',$,#40874);
#40832=PRODUCT_DEFINITION_SHAPE($,$,#83);
#40833=PRODUCT_DEFINITION_SHAPE($,$,#84);
#40834=PRODUCT_DEFINITION_SHAPE($,$,#85);
#40835=PRODUCT_DEFINITION_SHAPE($,$,#86);
#40836=PRODUCT_DEFINITION_SHAPE($,$,#87);
#40837=PRODUCT_DEFINITION_SHAPE($,$,#88);
#40838=PRODUCT_DEFINITION_SHAPE($,$,#89);
#40839=PRODUCT_DEFINITION_SHAPE($,$,#90);
#40840=PRODUCT_DEFINITION_SHAPE($,$,#91);
#40841=PRODUCT_DEFINITION_SHAPE($,$,#92);
#40842=PRODUCT_DEFINITION_SHAPE($,$,#93);
#40843=PRODUCT_DEFINITION_SHAPE($,$,#94);
#40844=PRODUCT_DEFINITION_SHAPE($,$,#95);
#40845=PRODUCT_DEFINITION_SHAPE($,$,#96);
#40846=PRODUCT_DEFINITION_SHAPE($,$,#97);
#40847=PRODUCT_DEFINITION_SHAPE($,$,#98);
#40848=PRODUCT_DEFINITION_SHAPE($,$,#99);
#40849=PRODUCT_DEFINITION_SHAPE($,$,#100);
#40850=PRODUCT_DEFINITION_SHAPE($,$,#101);
#40851=PRODUCT_DEFINITION_SHAPE($,$,#102);
#40852=PRODUCT_DEFINITION_SHAPE($,$,#103);
#40853=PRODUCT_DEFINITION_SHAPE($,$,#104);
#40854=PRODUCT_DEFINITION_SHAPE($,$,#105);
#40855=PRODUCT_DEFINITION_SHAPE($,$,#106);
#40856=SHAPE_REPRESENTATION('',(#6395,#7161,#7162,#7163,#7164,#7165,#7166,
#7167,#7168,#7169,#7170,#7171,#7172,#7173,#7174,#7175,#7176,#7177,#7178,
#7179,#7180,#7181,#7182,#7183,#7184),#40800);
#40857=SHAPE_REPRESENTATION('',(#6396),#40801);
#40858=SHAPE_REPRESENTATION('',(#6698),#40802);
#40859=SHAPE_REPRESENTATION('',(#6744),#40803);
#40860=SHAPE_REPRESENTATION('',(#6754),#40804);
#40861=SHAPE_REPRESENTATION('',(#6828),#40805);
#40862=SHAPE_REPRESENTATION('',(#6836),#40806);
#40863=SHAPE_REPRESENTATION('',(#7014),#40807);
#40864=SHAPE_REPRESENTATION('',(#7055),#40808);
#40865=PRODUCT_DEFINITION_CONTEXT('part definition',#40894,'design');
#40866=PRODUCT_DEFINITION('MAT-001','MAT-001',#40875,#40865);
#40867=PRODUCT_DEFINITION('Spider Wheel','Spider Wheel',#40876,#40865);
#40868=PRODUCT_DEFINITION('Rod','Rod',#40877,#40865);
#40869=PRODUCT_DEFINITION('Handle','Handle',#40878,#40865);
#40870=PRODUCT_DEFINITION('Hex Jam Nut 0.2500-20-D-S',
'Hex Jam Nut 0.2500-20-D-S',#40879,#40865);
#40871=PRODUCT_DEFINITION('rivet','Rivet',#40880,#40865);
#40872=PRODUCT_DEFINITION('Hex Finished Bolt 0.25-20x1.5x0.75-S',
'Hex Finished Bolt 0.25-20x1.5x0.75-S',#40881,#40865);
#40873=PRODUCT_DEFINITION('Carrier Arm Wheel','Carrier Arm Wheel',#40882,
#40865);
#40874=PRODUCT_DEFINITION('Puller Link','Puller Link',#40883,#40865);
#40875=PRODUCT_DEFINITION_FORMATION('',$,#40896);
#40876=PRODUCT_DEFINITION_FORMATION('',$,#40897);
#40877=PRODUCT_DEFINITION_FORMATION('',$,#40898);
#40878=PRODUCT_DEFINITION_FORMATION('',$,#40899);
#40879=PRODUCT_DEFINITION_FORMATION('',$,#40900);
#40880=PRODUCT_DEFINITION_FORMATION('',$,#40901);
#40881=PRODUCT_DEFINITION_FORMATION('',$,#40902);
#40882=PRODUCT_DEFINITION_FORMATION('',$,#40903);
#40883=PRODUCT_DEFINITION_FORMATION('',$,#40904);
#40884=PRODUCT_RELATED_PRODUCT_CATEGORY('MAT-001','MAT-001',(#40896));
#40885=PRODUCT_RELATED_PRODUCT_CATEGORY('Spider Wheel','Spider Wheel',(#40897));
#40886=PRODUCT_RELATED_PRODUCT_CATEGORY('Rod','Rod',(#40898));
#40887=PRODUCT_RELATED_PRODUCT_CATEGORY('Handle','Handle',(#40899));
#40888=PRODUCT_RELATED_PRODUCT_CATEGORY('Hex Jam Nut 0.2500-20-D-S',
'Hex Jam Nut 0.2500-20-D-S',(#40900));
#40889=PRODUCT_RELATED_PRODUCT_CATEGORY('Rivet','Rivet',(#40901));
#40890=PRODUCT_RELATED_PRODUCT_CATEGORY(
'Hex Finished Bolt 0.25-20x1.5x0.75-S',
'Hex Finished Bolt 0.25-20x1.5x0.75-S',(#40902));
#40891=PRODUCT_RELATED_PRODUCT_CATEGORY('Carrier Arm Wheel',
'Carrier Arm Wheel',(#40903));
#40892=PRODUCT_RELATED_PRODUCT_CATEGORY('Puller Link','Puller Link',(#40904));
#40893=APPLICATION_PROTOCOL_DEFINITION('international standard',
'automotive_design',2009,#40894);
#40894=APPLICATION_CONTEXT(
'Core Data for Automotive Mechanical Design Process');
#40895=PRODUCT_CONTEXT('part definition',#40894,'mechanical');
#40896=PRODUCT('MAT-001','MAT-001','STEP AP214',(#40895));
#40897=PRODUCT('Spider Wheel','Spider Wheel',$,(#40895));
#40898=PRODUCT('Rod','Rod',$,(#40895));
#40899=PRODUCT('Handle','Handle','Handle',(#40895));
#40900=PRODUCT('Hex Jam Nut 0.2500-20-D-S','Hex Jam Nut 0.2500-20-D-S',
$,(#40895));
#40901=PRODUCT('rivet','Rivet',$,(#40895));
#40902=PRODUCT('Hex Finished Bolt 0.25-20x1.5x0.75-S',
'Hex Finished Bolt 0.25-20x1.5x0.75-S',$,(#40895));
#40903=PRODUCT('Carrier Arm Wheel','Carrier Arm Wheel',$,(#40895));
#40904=PRODUCT('Puller Link','Puller Link',$,(#40895));
#40905=PRESENTATION_STYLE_ASSIGNMENT((#40910));
#40906=PRESENTATION_STYLE_ASSIGNMENT((#40911));
#40907=PRESENTATION_STYLE_ASSIGNMENT((#40912));
#40908=PRESENTATION_STYLE_ASSIGNMENT((#40913));
#40909=PRESENTATION_STYLE_ASSIGNMENT((#40914));
#40910=SURFACE_STYLE_USAGE(.BOTH.,#40915);
#40911=SURFACE_STYLE_USAGE(.BOTH.,#40916);
#40912=SURFACE_STYLE_USAGE(.BOTH.,#40917);
#40913=SURFACE_STYLE_USAGE(.BOTH.,#40918);
#40914=SURFACE_STYLE_USAGE(.BOTH.,#40919);
#40915=SURFACE_SIDE_STYLE('',(#40920));
#40916=SURFACE_SIDE_STYLE('',(#40921));
#40917=SURFACE_SIDE_STYLE('',(#40922));
#40918=SURFACE_SIDE_STYLE('',(#40923));
#40919=SURFACE_SIDE_STYLE('',(#40924));
#40920=SURFACE_STYLE_FILL_AREA(#40925);
#40921=SURFACE_STYLE_FILL_AREA(#40926);
#40922=SURFACE_STYLE_FILL_AREA(#40927);
#40923=SURFACE_STYLE_FILL_AREA(#40928);
#40924=SURFACE_STYLE_FILL_AREA(#40929);
#40925=FILL_AREA_STYLE('Steel - Satin',(#40930));
#40926=FILL_AREA_STYLE('Opaque(227,224,212)',(#40931));
#40927=FILL_AREA_STYLE('Opaque(122,133,145)',(#40932));
#40928=FILL_AREA_STYLE('Opaque(61,176,222)',(#40933));
#40929=FILL_AREA_STYLE('Opaque(31,36,43)',(#40934));
#40930=FILL_AREA_STYLE_COLOUR('Steel - Satin',#40935);
#40931=FILL_AREA_STYLE_COLOUR('Opaque(227,224,212)',#40936);
#40932=FILL_AREA_STYLE_COLOUR('Opaque(122,133,145)',#40937);
#40933=FILL_AREA_STYLE_COLOUR('Opaque(61,176,222)',#40938);
#40934=FILL_AREA_STYLE_COLOUR('Opaque(31,36,43)',#40939);
#40935=COLOUR_RGB('Steel - Satin',0.627450980392157,0.627450980392157,0.627450980392157);
#40936=COLOUR_RGB('Opaque(227,224,212)',0.890196078431372,0.87843137254902,
0.831372549019608);
#40937=COLOUR_RGB('Opaque(122,133,145)',0.47843137254902,0.52156862745098,
0.568627450980392);
#40938=COLOUR_RGB('Opaque(61,176,222)',0.23921568627451,0.690196078431373,
0.870588235294118);
#40939=COLOUR_RGB('Opaque(31,36,43)',0.12156862745098,0.141176470588235,
0.168627450980392);
ENDSEC;
END-ISO-10303-21;
